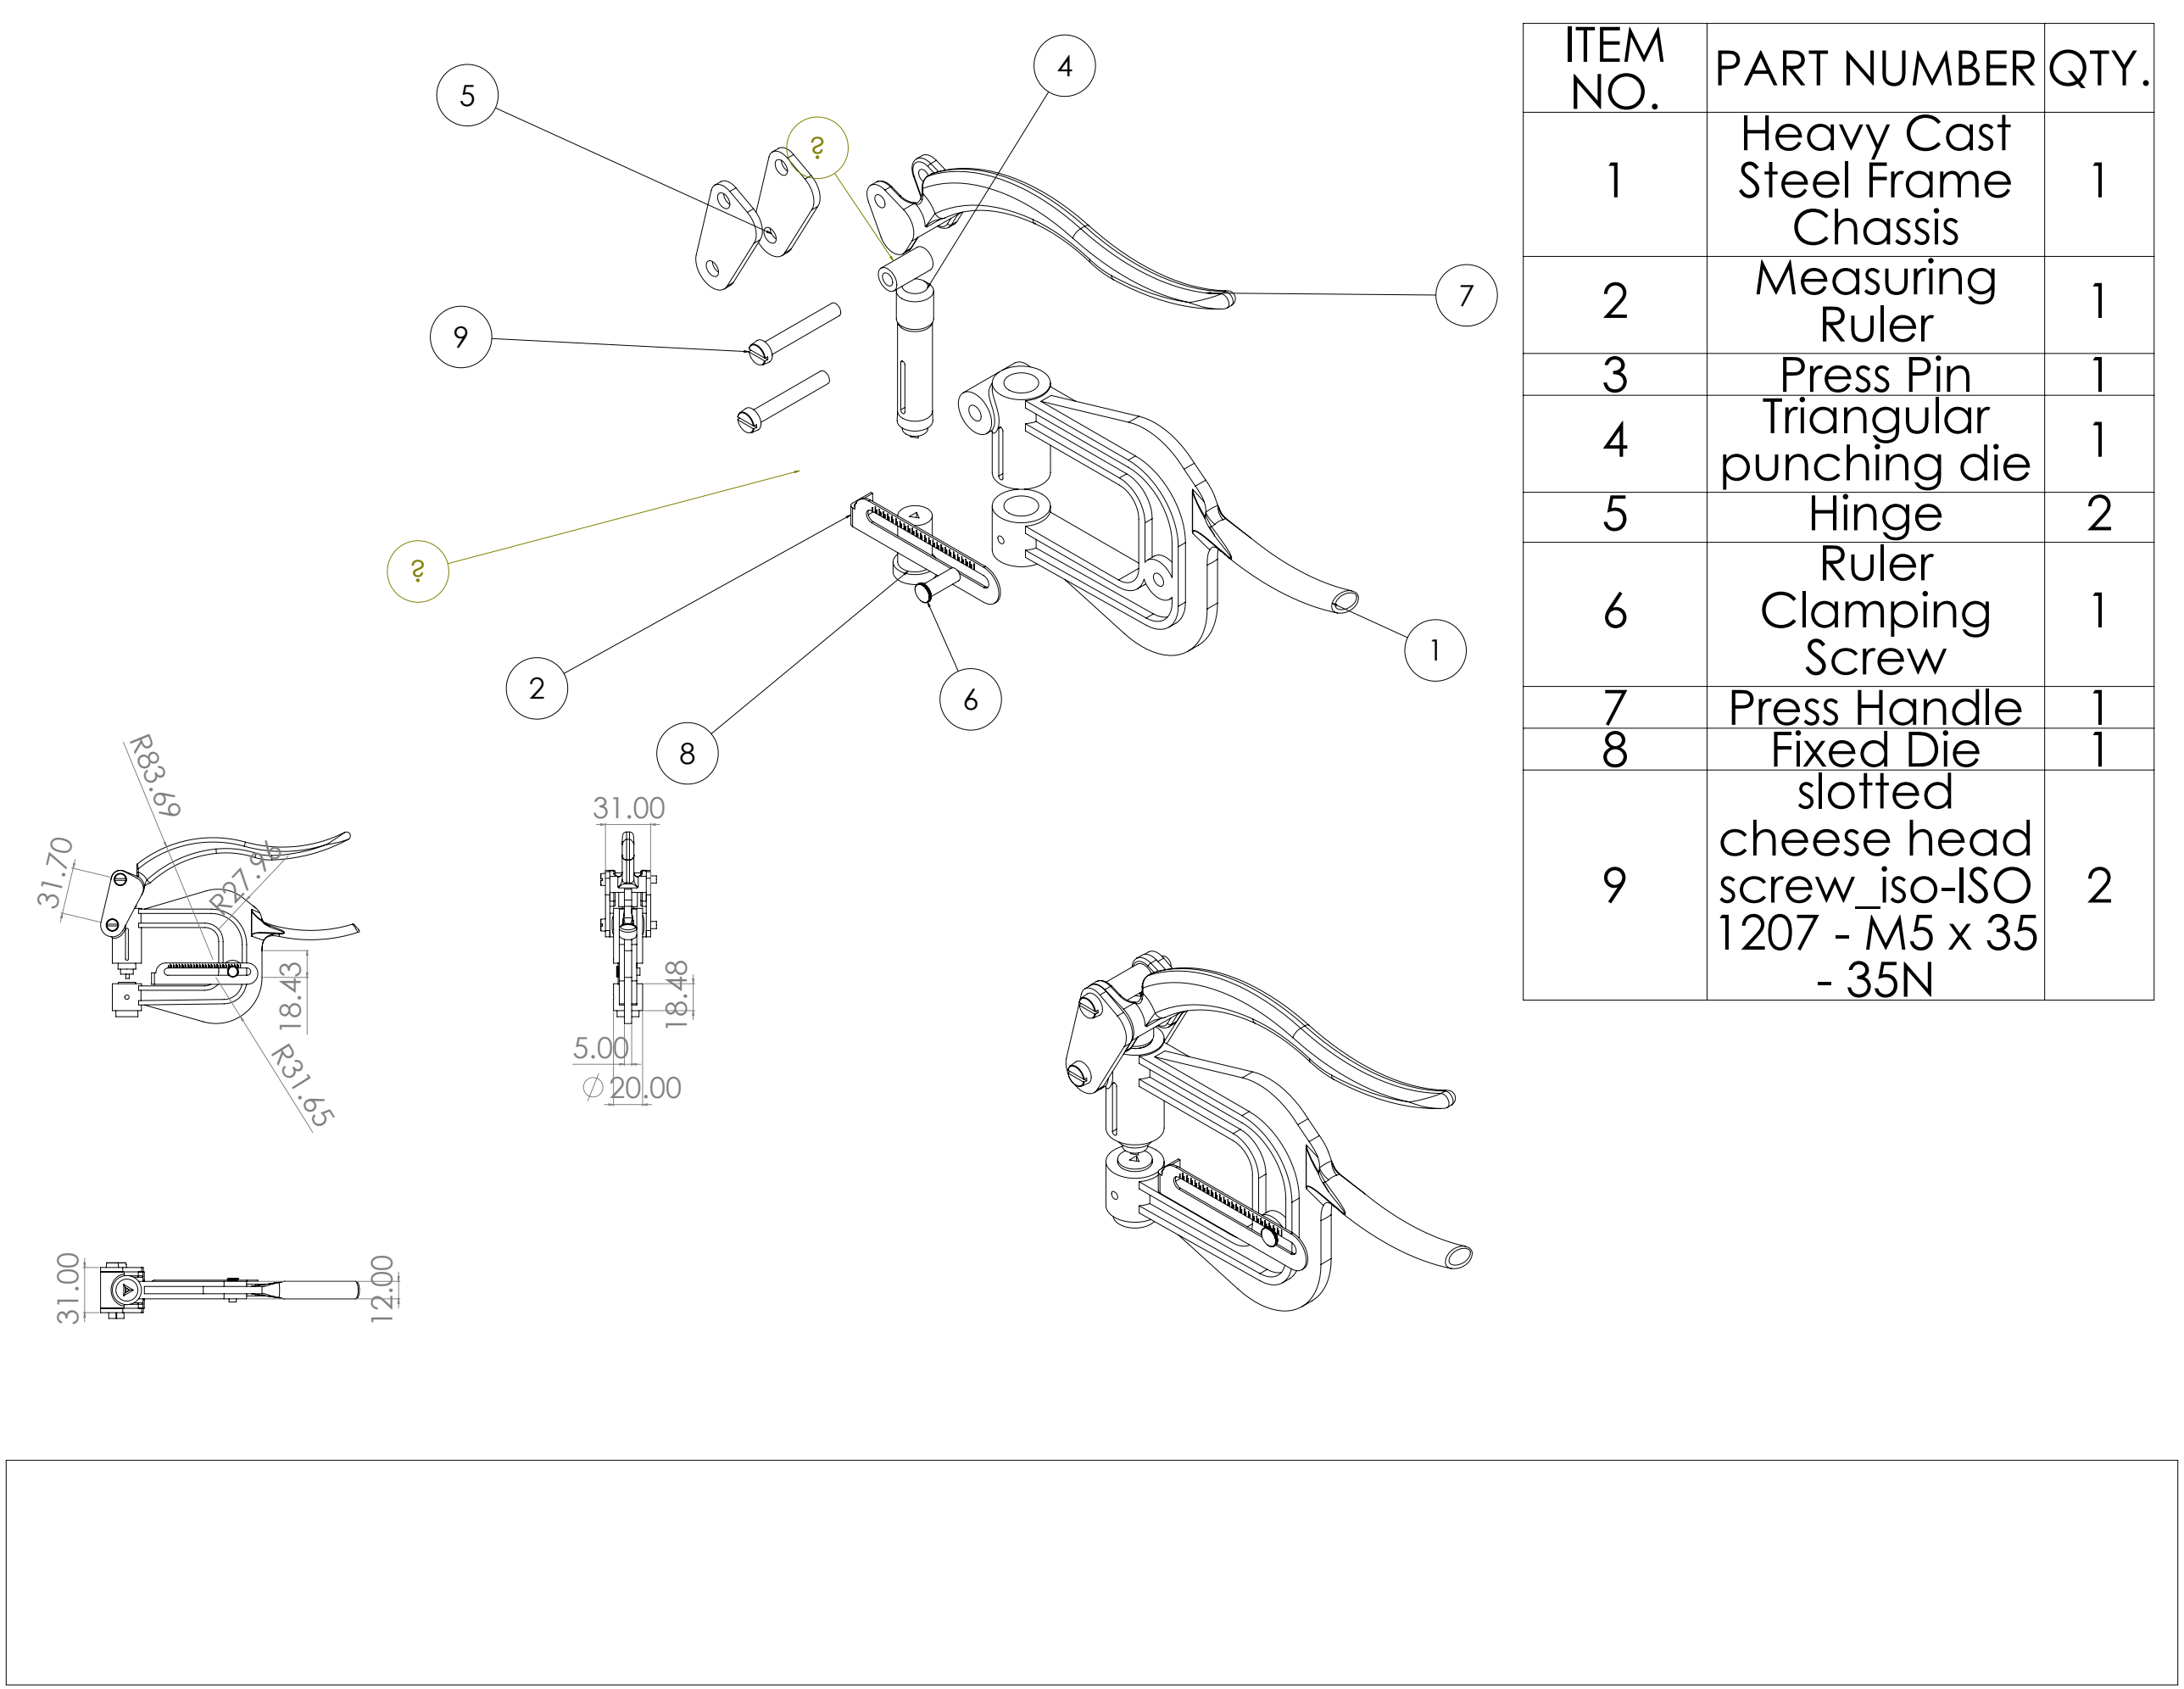
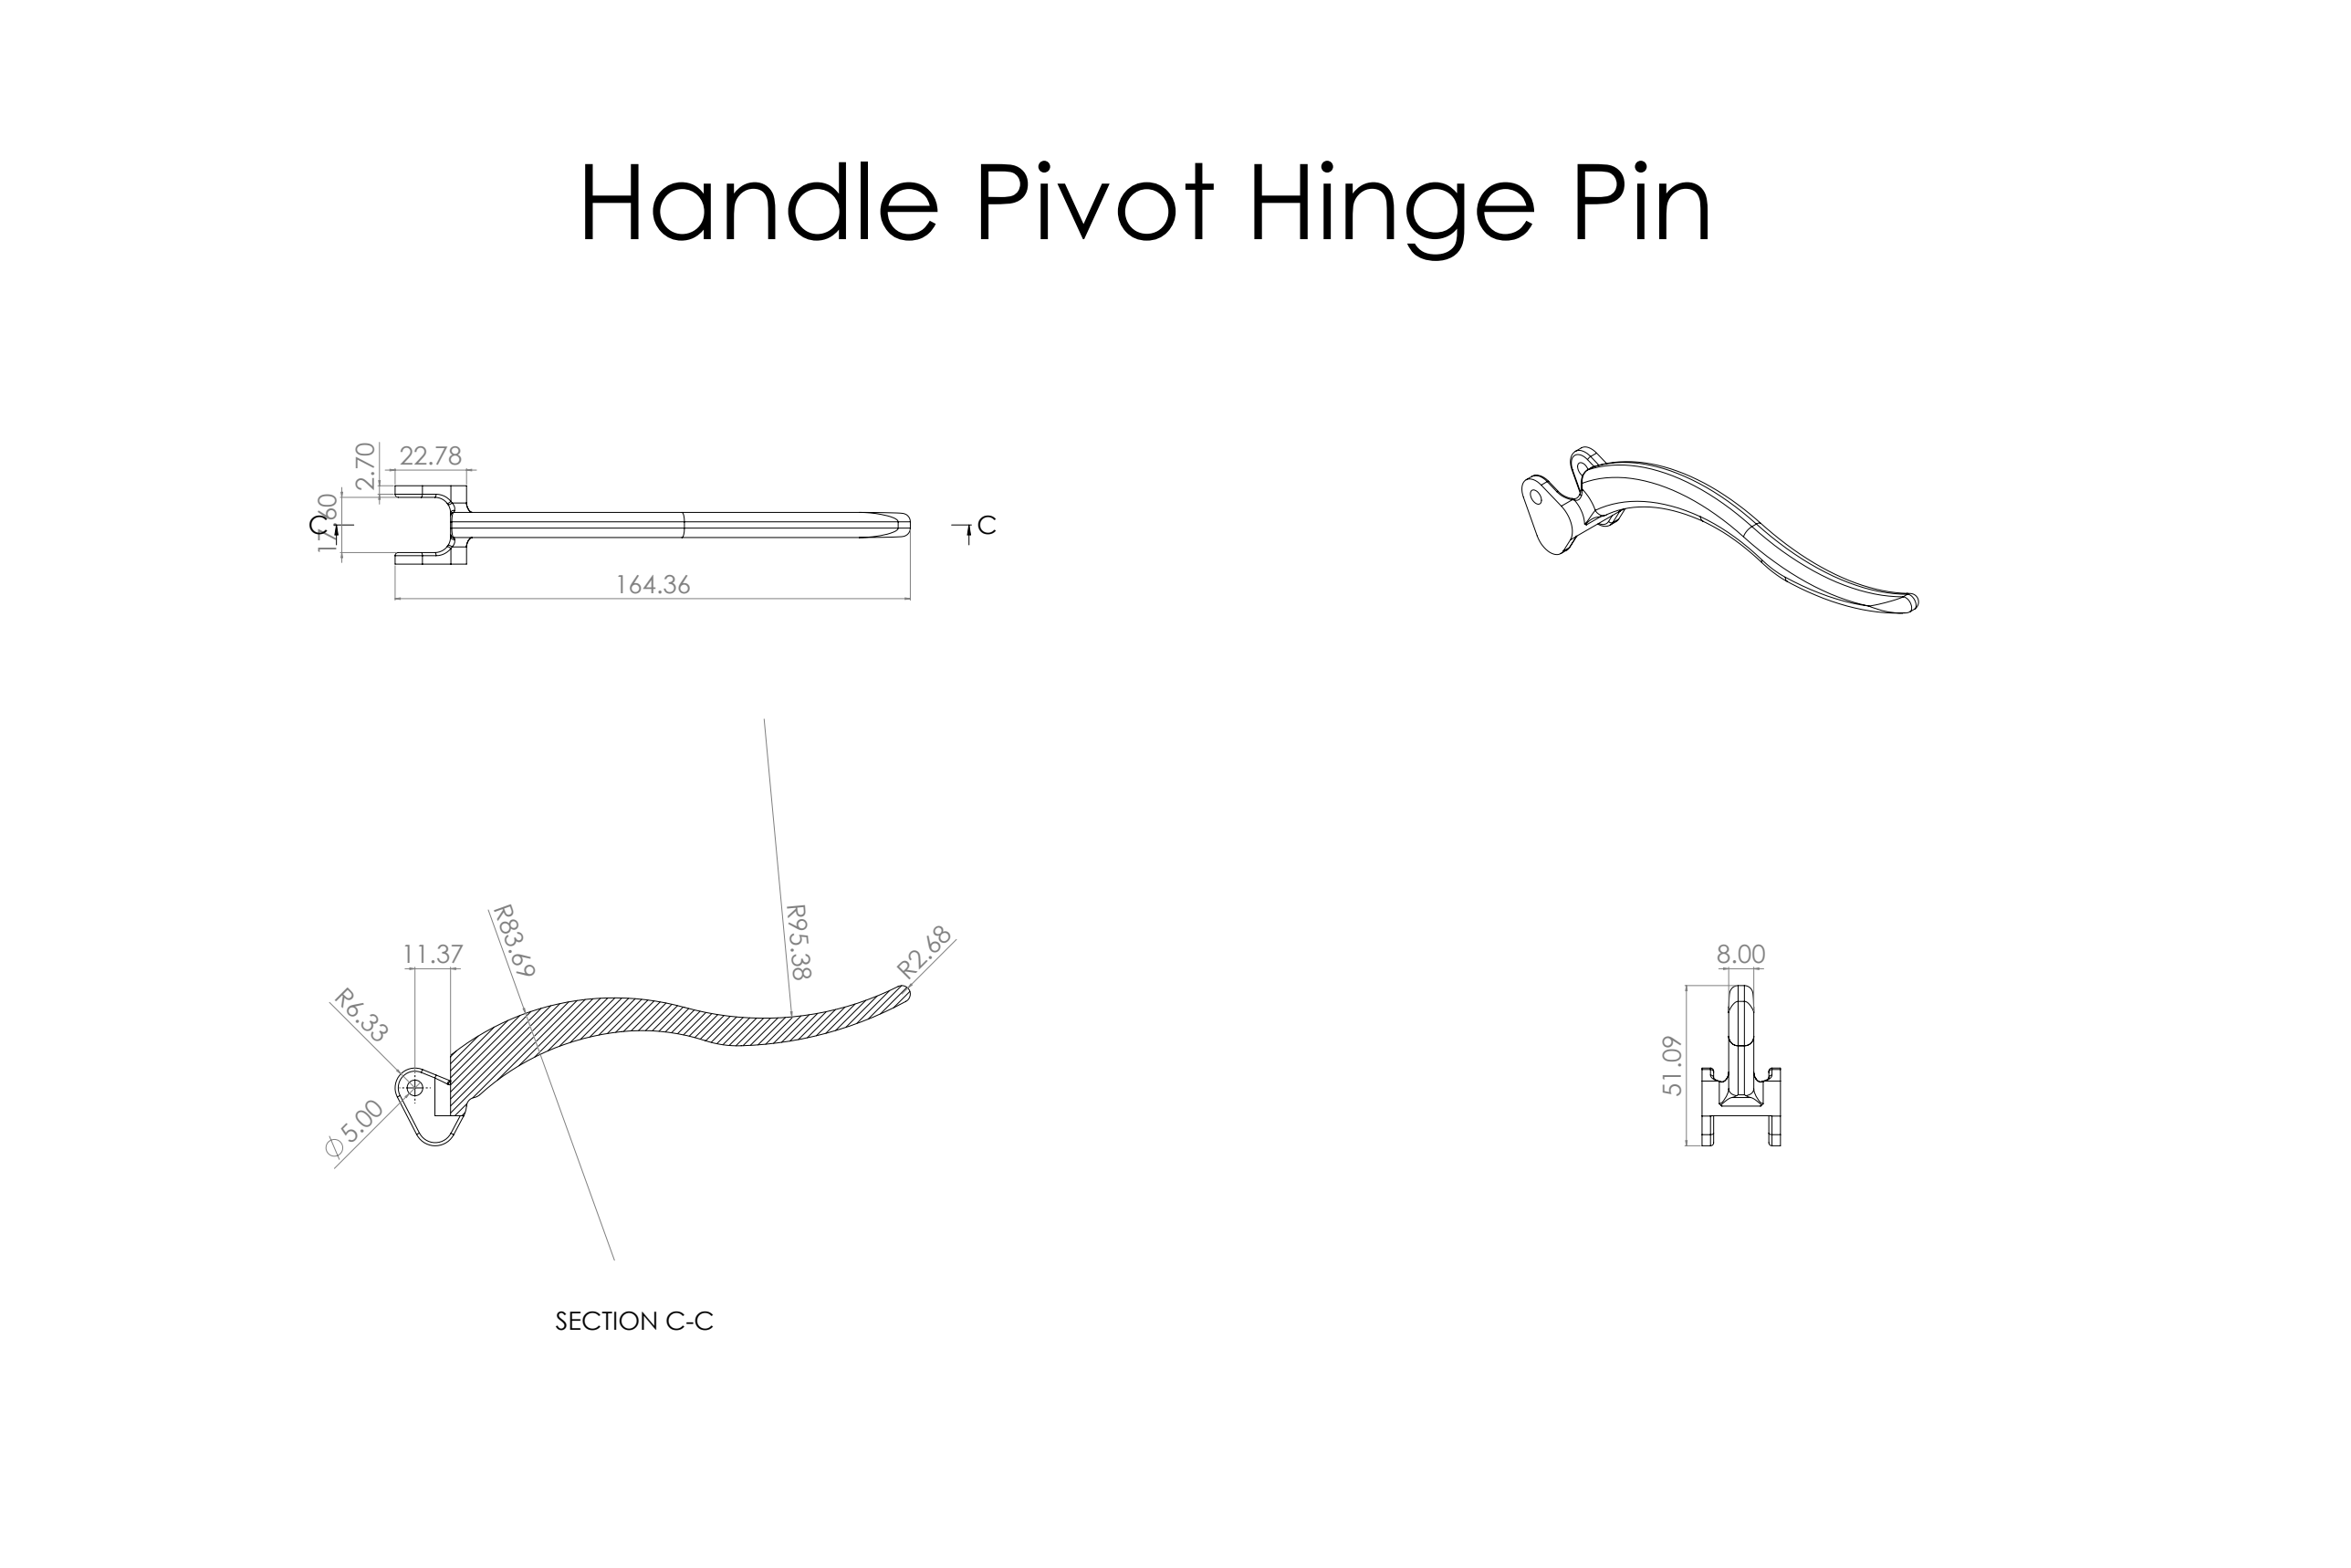
ISO-10303-21;
HEADER;
FILE_DESCRIPTION (('STEP AP214'),
    '1' );
FILE_NAME ('MAS-318',
    '2026-10-24T22:54:28',
    ( '' ),
    ( '' ),
    'SwSTEP 2.0',
    'SolidWorks 2025',
    '' );
FILE_SCHEMA (( 'AUTOMOTIVE_DESIGN' ));
ENDSEC;

DATA;
#1 = ORIENTED_EDGE ( 'NONE', *, *, #34988, .F. ) ;
#2 = CARTESIAN_POINT ( 'NONE',  ( 80.93548213101077238, 62.17232332437959030, -2.988136994358703724 ) ) ;
#3 = CARTESIAN_POINT ( 'NONE',  ( 35.84136525188217348, -3.161327592290550825, 5.800309892887216989 ) ) ;
#4 = EDGE_LOOP ( 'NONE', ( #11290, #35593, #8233, #19286 ) ) ;
#6 = DIRECTION ( 'NONE',  ( 0.000000000000000000, -1.000000000000000000, 0.000000000000000000 ) ) ;
#5 = CARTESIAN_POINT ( 'NONE',  ( 21.85645829928708039, 3.222455659797274663, 4.920547929353077166 ) ) ;
#7 = VERTEX_POINT ( 'NONE', #10173 ) ;
#8 = AXIS2_PLACEMENT_3D ( 'NONE', #5733, #22003, #2874 ) ;
#9 = CARTESIAN_POINT ( 'NONE',  ( -69.92837670882107659, -20.78299143688747819, 3.916079783099623679 ) ) ;
#10 =( BOUNDED_CURVE ( )  B_SPLINE_CURVE ( 3, ( #30460, #11695, #20771, #8817 ),
 .UNSPECIFIED., .F., .T. ) 
 B_SPLINE_CURVE_WITH_KNOTS ( ( 4, 4 ),
 ( 1.347909859412855349, 1.534781240595300522 ),
 .UNSPECIFIED. ) 
 CURVE ( )  GEOMETRIC_REPRESENTATION_ITEM ( )  RATIONAL_B_SPLINE_CURVE ( ( 1.000000000000000000, 0.9970920404276226723, 0.9970920404276226723, 1.000000000000000000 ) ) 
 REPRESENTATION_ITEM ( '' )  );
#11 = PRODUCT_DEFINITION_SHAPE ( 'NONE', 'NONE',  #40728 ) ;
#13 = CARTESIAN_POINT ( 'NONE',  ( -63.96477757089261473, 34.57625524247897175, 12.50000000000000000 ) ) ;
#12 = CARTESIAN_POINT ( 'NONE',  ( -71.92837670882107659, -20.78299143688747819, 38.00000000000000711 ) ) ;
#14 = LINE ( 'NONE', #31910, #38253 ) ;
#15 = CARTESIAN_POINT ( 'NONE',  ( -64.08758708074093136, 42.07456177326923097, -2.837280263138449943 ) ) ;
#16 = CARTESIAN_POINT ( 'NONE',  ( 73.82474952339838126, 59.08733682254641195, 3.476886323308218341 ) ) ;
#17 = EDGE_CURVE ( 'NONE', #19674, #35253, #14622, .T. ) ;
#18 = ORIENTED_EDGE ( 'NONE', *, *, #8070, .F. ) ;
#19 = CARTESIAN_POINT ( 'NONE',  ( 21.85695786933250062, 3.618345527896555058, -4.619311229777957273 ) ) ;
#20 = ORIENTED_EDGE ( 'NONE', *, *, #32884, .T. ) ;
#21 = CARTESIAN_POINT ( 'NONE',  ( 21.85643539959774273, 10.54442680926682208, -0.8960936389291185300 ) ) ;
#22 = CIRCLE ( 'NONE', #10506, 0.1000000000000028644 ) ;
#23 = CARTESIAN_POINT ( 'NONE',  ( 3.455257086698204194, -26.54807830652391587, 7.773839561854632763 ) ) ;
#24 = ORIENTED_EDGE ( 'NONE', *, *, #28416, .F. ) ;
#25 = ORIENTED_EDGE ( 'NONE', *, *, #12233, .F. ) ;
#26 = CARTESIAN_POINT ( 'NONE',  ( 1.060267149064800352, -26.12896262584469298, 7.720710062488891801 ) ) ;
#27 = CARTESIAN_POINT ( 'NONE',  ( 81.24504193829311305, 64.75648403698987465, 3.071899782094678066 ) ) ;
#28 = CARTESIAN_POINT ( 'NONE',  ( 84.98726364908050357, 2.895996327189970021, 0.3032432708941606436 ) ) ;
#29 = ORIENTED_EDGE ( 'NONE', *, *, #33251, .T. ) ;
#30 = EDGE_CURVE ( 'NONE', #25319, #33264, #34800, .T. ) ;
#31 = CARTESIAN_POINT ( 'NONE',  ( 0.5348300231373435132, -32.76390415370035214, 7.769368695748487319 ) ) ;
#32 = ORIENTED_EDGE ( 'NONE', *, *, #7574, .F. ) ;
#33 = CARTESIAN_POINT ( 'NONE',  ( 15.61026443024166888, -3.737113800699907618, 2.632854455050967157 ) ) ;
#34 = ADVANCED_FACE ( 'NONE', ( #40006 ), #27046, .T. ) ;
#35 = CARTESIAN_POINT ( 'NONE',  ( 34.13602976376383680, -3.136024335859604495, -5.534151046271431618 ) ) ;
#36 = CARTESIAN_POINT ( 'NONE',  ( 5.099449461929271621, -29.65043611971386639, 7.782034975670477195 ) ) ;
#37 = DIRECTION ( 'NONE',  ( 1.000000000000000000, 0.000000000000000000, 0.000000000000000000 ) ) ;
#38 = AXIS2_PLACEMENT_3D ( 'NONE', #3449, #15964, #28321 ) ;
#39 = CARTESIAN_POINT ( 'NONE',  ( -1.226608418644374421, -31.29986830985462376, 7.712764235869104645 ) ) ;
#40 = EDGE_CURVE ( 'NONE', #7218, #20784, #16731, .T. ) ;
#41 = ORIENTED_EDGE ( 'NONE', *, *, #18908, .F. ) ;
#42 = ORIENTED_EDGE ( 'NONE', *, *, #27798, .T. ) ;
#43 = CARTESIAN_POINT ( 'NONE',  ( 37.00808470818950013, -3.245065655003315896, 5.947274188226997715 ) ) ;
#44 = DIRECTION ( 'NONE',  ( -0.000000000000000000, -0.000000000000000000, 1.000000000000000000 ) ) ;
#45 = CARTESIAN_POINT ( 'NONE',  ( 66.41901733680204245, 57.79934748174496661, -4.000000000000019540 ) ) ;
#46 = CARTESIAN_POINT ( 'NONE',  ( 87.70627581785944926, -2.246752060737267964, -2.595469083058261184 ) ) ;
#47 = ORIENTED_EDGE ( 'NONE', *, *, #36430, .F. ) ;
#48 = CIRCLE ( 'NONE', #2012, 0.1000000000000028644 ) ;
#49 = CARTESIAN_POINT ( 'NONE',  ( -32.87867591359218977, -26.64985754041175525, 6.700000000000000178 ) ) ;
#50 = CARTESIAN_POINT ( 'NONE',  ( -70.92837670882107659, -23.80776546975053520, 0.000000000000000000 ) ) ;
#51 = ORIENTED_EDGE ( 'NONE', *, *, #25814, .F. ) ;
#52 = FACE_BOUND ( 'NONE', #30582, .T. ) ;
#53 = CARTESIAN_POINT ( 'NONE',  ( 3.926249267005272436, -32.27095793936597090, 6.894806418505347700 ) ) ;
#54 = EDGE_LOOP ( 'NONE', ( #15981, #402, #1244, #38858 ) ) ;
#55 = CARTESIAN_POINT ( 'NONE',  ( 24.04452188815935898, 3.332949059894338983, 3.268005727657652404 ) ) ;
#56 = CARTESIAN_POINT ( 'NONE',  ( 80.36293583174420974, 66.30725055998094319, -1.299258709309398130 ) ) ;
#57 = EDGE_CURVE ( 'NONE', #6790, #7577, #6515, .T. ) ;
#58 = CARTESIAN_POINT ( 'NONE',  ( 79.04990754624076033, 65.77731930041099417, 2.468641556982019925 ) ) ;
#59 = CARTESIAN_POINT ( 'NONE',  ( 2.829405163535268386, -26.36285597610873310, 7.703977250142849620 ) ) ;
#60 = ORIENTED_EDGE ( 'NONE', *, *, #39491, .F. ) ;
#61 = CARTESIAN_POINT ( 'NONE',  ( 76.46949791074162306, 63.77707083977483649, -3.308002540424319626 ) ) ;
#63 = CARTESIAN_POINT ( 'NONE',  ( -19.07867591359219972, -24.55319635012989110, 6.800000000000000711 ) ) ;
#62 = CARTESIAN_POINT ( 'NONE',  ( -71.02647992656017095, -45.61702805680359774, 6.000000000000006217 ) ) ;
#64 = CARTESIAN_POINT ( 'NONE',  ( 17.44489164598297748, 8.923283497490654526, -2.906184072486747816 ) ) ;
#65 = CARTESIAN_POINT ( 'NONE',  ( 81.32291525751645622, 62.59435864775878144, -3.036434590848177795 ) ) ;
#66 = CARTESIAN_POINT ( 'NONE',  ( 78.75717319332348154, 60.46956391627949756, 2.498359881428524609 ) ) ;
#67 = ORIENTED_EDGE ( 'NONE', *, *, #17962, .F. ) ;
#68 = VECTOR ( 'NONE', #23704, 1000.000000000000114 ) ;
#69 = DIRECTION ( 'NONE',  ( 0.000000000000000000, 0.000000000000000000, 1.000000000000000000 ) ) ;
#70 = CARTESIAN_POINT ( 'NONE',  ( 1.700390093233090871, -29.56993018339339940, 7.800000000000000711 ) ) ;
#71 = CARTESIAN_POINT ( 'NONE',  ( 80.25084519670748762, 66.24728552308215512, 1.725837398062988415 ) ) ;
#73 = CARTESIAN_POINT ( 'NONE',  ( -1.583170569706177977, -30.78163712919650052, 7.638132480492516585 ) ) ;
#72 = DIRECTION ( 'NONE',  ( -0.000000000000000000, 1.000000000000000000, -0.000000000000000000 ) ) ;
#74 = CARTESIAN_POINT ( 'NONE',  ( 27.93970670347097851, 2.313158937601060838, 2.612756796560576689 ) ) ;
#75 = ADVANCED_FACE ( 'NONE', ( #21079, #21280 ), #17552, .T. ) ;
#76 = EDGE_CURVE ( 'NONE', #14380, #23841, #36922, .T. ) ;
#77 = CARTESIAN_POINT ( 'NONE',  ( -1.419381273142192645, -31.15644416743037937, 6.921725064902950031 ) ) ;
#78 = CARTESIAN_POINT ( 'NONE',  ( 21.32819773538203734, -0.9284710762945487250, 4.803740791084685213 ) ) ;
#79 = CARTESIAN_POINT ( 'NONE',  ( -64.37872067649581709, 36.58503142451505141, 5.660009492437676037 ) ) ;
#80 = EDGE_CURVE ( 'NONE', #2391, #5443, #34066, .T. ) ;
#81 = DIRECTION ( 'NONE',  ( -0.000000000000000000, -0.000000000000000000, -1.000000000000000000 ) ) ;
#82 = ORIENTED_EDGE ( 'NONE', *, *, #9020, .T. ) ;
#83 = CARTESIAN_POINT ( 'NONE',  ( -0.6417018516168193631, -32.03460162637909292, 6.959317978105162616 ) ) ;
#84 = DIRECTION ( 'NONE',  ( 0.8660254037844393737, 0.000000000000000000, 0.4999999999999985567 ) ) ;
#85 = PLANE ( 'NONE',  #11053 ) ;
#86 = CARTESIAN_POINT ( 'NONE',  ( 33.43749314767592296, -3.587398716883661631, -5.336340041065867901 ) ) ;
#87 = CARTESIAN_POINT ( 'NONE',  ( -0.8882241849766865371, -31.77426936318072848, 7.740055089680403455 ) ) ;
#88 = CARTESIAN_POINT ( 'NONE',  ( 0.4809511200452799562, -32.83872382006634894, 7.781480525794716385 ) ) ;
#89 = DIRECTION ( 'NONE',  ( -0.000000000000000000, -0.000000000000000000, 1.000000000000000000 ) ) ;
#90 = CARTESIAN_POINT ( 'NONE',  ( 87.15505355144220800, 0.4610318193416703680, -5.246243280819175681 ) ) ;
#91 = CARTESIAN_POINT ( 'NONE',  ( 23.06594672544511582, -8.086844732617873177, 2.500000000000001332 ) ) ;
#92 = CARTESIAN_POINT ( 'NONE',  ( -14.44874870218064089, -26.64985754041175525, 6.700000000000000178 ) ) ;
#93 = ORIENTED_EDGE ( 'NONE', *, *, #2114, .F. ) ;
#94 = DIRECTION ( 'NONE',  ( -0.000000000000000000, -0.000000000000000000, -1.000000000000000000 ) ) ;
#95 = CARTESIAN_POINT ( 'NONE',  ( 68.04343099365841852, 58.34291608657256489, -3.996230182412897403 ) ) ;
#96 = AXIS2_PLACEMENT_3D ( 'NONE', #13585, #39295, #10487 ) ;
#97 = CARTESIAN_POINT ( 'NONE',  ( 2.985793545108982983, -26.31449737714283543, 6.863805608295730387 ) ) ;
#98 = ORIENTED_EDGE ( 'NONE', *, *, #35067, .F. ) ;
#99 = CARTESIAN_POINT ( 'NONE',  ( 8.290806648384990041, -33.63722727088462250, 6.000000000000001776 ) ) ;
#100 = CARTESIAN_POINT ( 'NONE',  ( 5.698101969243359655, -32.85371976261941285, 7.695279973900954751 ) ) ;
#101 = PRODUCT ( 'Press Handle', 'Press Handle', '', ( #4245 ) ) ;
#102 = CARTESIAN_POINT ( 'NONE',  ( 1.179471205431445346, -26.21005746276246029, 7.784476445165072533 ) ) ;
#103 = CARTESIAN_POINT ( 'NONE',  ( 5.054793046568992310, -30.12489038615697012, 7.703977250142847844 ) ) ;
#104 = ORIENTED_EDGE ( 'NONE', *, *, #1781, .F. ) ;
#105 = CARTESIAN_POINT ( 'NONE',  ( 24.41733686895641853, 3.169751135957838084, 3.243633740826553424 ) ) ;
#106 = CARTESIAN_POINT ( 'NONE',  ( 1.651639975615219580, -32.96958066925694908, 6.894806418505345036 ) ) ;
#107 = VECTOR ( 'NONE', #13832, 1000.000000000000000 ) ;
#108 = CARTESIAN_POINT ( 'NONE',  ( -1.333134932519906446, -31.10541900397473825, 7.013842709614101167 ) ) ;
#109 = VERTEX_POINT ( 'NONE', #17965 ) ;
#110 = CARTESIAN_POINT ( 'NONE',  ( 78.59948840878007559, 65.10367658859402695, -3.015657119755322579 ) ) ;
#112 = CARTESIAN_POINT ( 'NONE',  ( -40.44874870218063734, -26.64985754041175525, 6.700000000000000178 ) ) ;
#111 = CARTESIAN_POINT ( 'NONE',  ( 23.09356329134889663, 0.3660385851480518205, 5.918987391801470821 ) ) ;
#113 = B_SPLINE_CURVE_WITH_KNOTS ( 'NONE', 3,
 ( #29364, #35364, #7331, #3877, #28763, #574, #25671, #10213, #29561, #28964 ),
 .UNSPECIFIED., .F., .F.,
 ( 4, 3, 3, 4 ),
 ( 8.388765757908052086E-05, 0.0001053129305727058042, 0.0001360598016347105499, 0.0001612931755702039531 ),
 .UNSPECIFIED. ) ;
#114 = CARTESIAN_POINT ( 'NONE',  ( 81.64185025298566245, 61.96196063151609223, -2.170472567296702682 ) ) ;
#115 = CARTESIAN_POINT ( 'NONE',  ( 80.76516742887832834, 61.34548671587045021, 2.174061886842027391 ) ) ;
#116 = EDGE_CURVE ( 'NONE', #25222, #15928, #15693, .T. ) ;
#117 = EDGE_CURVE ( 'NONE', #23904, #23738, #12152, .T. ) ;
#118 = CARTESIAN_POINT ( 'NONE',  ( 82.55792188592127445, 63.20960171500894376, 1.000000000000000000 ) ) ;
#119 = CARTESIAN_POINT ( 'NONE',  ( 2.752162513012757827, -32.80316080117250266, 7.759451378593094084 ) ) ;
#120 = CARTESIAN_POINT ( 'NONE',  ( 21.85643539959779602, 4.838159542671753854, -10.55000746994157979 ) ) ;
#121 = EDGE_LOOP ( 'NONE', ( #23412, #22869, #10746, #16528 ) ) ;
#122 = CARTESIAN_POINT ( 'NONE',  ( -73.76321677170048474, 8.370041474172571938, 9.593160009199120708 ) ) ;
#123 = CARTESIAN_POINT ( 'NONE',  ( 37.18496992949054913, -2.918767381260244154, 5.998331359843706245 ) ) ;
#124 = ORIENTED_EDGE ( 'NONE', *, *, #26461, .T. ) ;
#125 = EDGE_CURVE ( 'NONE', #38679, #29790, #4804, .T. ) ;
#126 = CARTESIAN_POINT ( 'NONE',  ( -1.313163417236760111, -31.34995842213618999, 7.678495282201405203 ) ) ;
#127 = CARTESIAN_POINT ( 'NONE',  ( -80.34626650618338317, 10.54088118240301775, -3.386839445737261034 ) ) ;
#128 = CARTESIAN_POINT ( 'NONE',  ( 28.64320648638592104, -3.206774183960824587, -4.676863129512683237 ) ) ;
#129 = CARTESIAN_POINT ( 'NONE',  ( 37.18689723876565978, -2.963747097358016003, -6.000011646107364705 ) ) ;
#130 = CARTESIAN_POINT ( 'NONE',  ( -4.890026461918814071, -8.228598103685714525E-16, 6.000000000000000000 ) ) ;
#131 = SHAPE_REPRESENTATION ( 'Heavy Cast Steel Frame Chassis', ( #30744 ), #7710 ) ;
#132 = CARTESIAN_POINT ( 'NONE',  ( 21.48907598089328630, 5.617352746613489600, 3.514627525551620391 ) ) ;
#133 = CARTESIAN_POINT ( 'NONE',  ( -1.740904132959085304, -28.93157757802832819, 6.894806418505347700 ) ) ;
#134 = DIRECTION ( 'NONE',  ( 7.826543628040252284E-17, -1.000000000000000000, 0.000000000000000000 ) ) ;
#135 = DIRECTION ( 'NONE',  ( 0.000000000000000000, 0.000000000000000000, -1.000000000000000000 ) ) ;
#136 = DIRECTION ( 'NONE',  ( -1.000000000000000000, 0.000000000000000000, 0.000000000000000000 ) ) ;
#137 = CARTESIAN_POINT ( 'NONE',  ( 21.75356392267549310, 0.6818289899092313533, -8.045969637709488254 ) ) ;
#138 = VECTOR ( 'NONE', #4313, 1000.000000000000000 ) ;
#139 = CARTESIAN_POINT ( 'NONE',  ( 32.63483486068848549, -3.790703822822770075, -4.926795467402606654 ) ) ;
#140 = CARTESIAN_POINT ( 'NONE',  ( 25.39710067966193918, 2.282707499838438459, -4.082506721808119465 ) ) ;
#141 = VERTEX_POINT ( 'NONE', #15910 ) ;
#142 = VERTEX_POINT ( 'NONE', #21892 ) ;
#143 = CARTESIAN_POINT ( 'NONE',  ( 66.81418162778464875, 58.07599004166701206, 3.996206253860483226 ) ) ;
#144 = CARTESIAN_POINT ( 'NONE',  ( 35.79015163951060430, -3.279169341215469213, 5.792316770070685017 ) ) ;
#145 = DIRECTION ( 'NONE',  ( 0.7055275666422168301, -0.2567910337120241637, -0.6605219282605403475 ) ) ;
#146 = CARTESIAN_POINT ( 'NONE',  ( 87.19696342060086636, -0.1553247823698818142, -5.755373573531420206 ) ) ;
#148 = DIRECTION ( 'NONE',  ( 0.000000000000000000, 1.000000000000000000, 0.000000000000000000 ) ) ;
#147 = CARTESIAN_POINT ( 'NONE',  ( -83.92837670882109080, 2.429809908903242555, 15.50000000000000000 ) ) ;
#149 = ORIENTED_EDGE ( 'NONE', *, *, #27849, .F. ) ;
#150 = CARTESIAN_POINT ( 'NONE',  ( 24.34527755301806451, 2.925195485058063927, 3.749207160500627634 ) ) ;
#151 =( NAMED_UNIT ( * ) PLANE_ANGLE_UNIT ( ) SI_UNIT ( $, .RADIAN. ) );
#152 = CARTESIAN_POINT ( 'NONE',  ( -1.531573891984414848, -33.61112889622174293, 7.754798119455333705 ) ) ;
#153 = VERTEX_POINT ( 'NONE', #35081 ) ;
#154 = CARTESIAN_POINT ( 'NONE',  ( 3.979840844262043209, -26.93328804621895145, 7.785344483711591934 ) ) ;
#155 = ORIENTED_EDGE ( 'NONE', *, *, #18670, .T. ) ;
#156 = CARTESIAN_POINT ( 'NONE',  ( 80.09094484276194237, 63.40703332228277134, -3.714073935154547978 ) ) ;
#157 = CARTESIAN_POINT ( 'NONE',  ( 4.045228995182856835, -26.97152095390259063, 7.750000000000000888 ) ) ;
#158 = CARTESIAN_POINT ( 'NONE',  ( 80.96252947514877008, 61.71397308826822581, 2.561782662428527146 ) ) ;
#160 = VERTEX_POINT ( 'NONE', #28468 ) ;
#159 = CARTESIAN_POINT ( 'NONE',  ( -1.333134932519906446, -31.10541900397473825, 7.013842709614101167 ) ) ;
#161 = CARTESIAN_POINT ( 'NONE',  ( -56.74902312943272165, 30.60926302035622371, 3.177788716294913218 ) ) ;
#162 = DIRECTION ( 'NONE',  ( 1.000000000000000000, 0.000000000000000000, 0.000000000000000000 ) ) ;
#163 = CARTESIAN_POINT ( 'NONE',  ( -71.80187163192030653, -21.28714814314140469, 9.961904852117910991 ) ) ;
#164 = CARTESIAN_POINT ( 'NONE',  ( 5.401390093233090717, -29.58343279012807159, 7.635761828346577573 ) ) ;
#165 = CARTESIAN_POINT ( 'NONE',  ( 22.18865037645032601, 5.257466153314783064, -3.084642082178049360 ) ) ;
#166 = ORIENTED_EDGE ( 'NONE', *, *, #31920, .F. ) ;
#167 = CIRCLE ( 'NONE', #21192, 3.000000000000002665 ) ;
#168 = EDGE_CURVE ( 'NONE', #27559, #13108, #28679, .T. ) ;
#169 = VERTEX_POINT ( 'NONE', #9734 ) ;
#170 = ADVANCED_FACE ( 'NONE', ( #3587 ), #276, .T. ) ;
#171 = CARTESIAN_POINT ( 'NONE',  ( -1.621161547238496814, -30.32835594263312018, 7.139196562012270597 ) ) ;
#172 = ADVANCED_FACE ( 'NONE', ( #34882 ), #28059, .T. ) ;
#173 = CARTESIAN_POINT ( 'NONE',  ( -80.59724102483603758, -5.646254625739555166, -5.338710406051827562 ) ) ;
#174 = DIRECTION ( 'NONE',  ( 0.1736481776669273336, 0.9848077530122085754, -0.000000000000000000 ) ) ;
#175 = CARTESIAN_POINT ( 'NONE',  ( 80.63945418285952371, 64.43655742540516940, 3.486376426170536114 ) ) ;
#176 = CARTESIAN_POINT ( 'NONE',  ( 87.91343731185466481, -2.496140582104141359, -0.8634702502314072214 ) ) ;
#177 = CARTESIAN_POINT ( 'NONE',  ( -0.5626977249550375593, -26.90001753928526540, 7.750000000000002665 ) ) ;
#178 = ORIENTED_EDGE ( 'NONE', *, *, #20772, .F. ) ;
#179 = LINE ( 'NONE', #33956, #26669 ) ;
#180 = CARTESIAN_POINT ( 'NONE',  ( -2.184219888937934950, -32.98850935093154391, 7.754798119455333705 ) ) ;
#181 = CARTESIAN_POINT ( 'NONE',  ( 4.091040325523227494, -27.01360636453728503, 6.980586498568968956 ) ) ;
#182 = CARTESIAN_POINT ( 'NONE',  ( -32.44874870218063734, -26.64985754041175525, 6.700000000000000178 ) ) ;
#183 = CARTESIAN_POINT ( 'NONE',  ( 4.697270888919727660, -27.96407818295915249, 7.768425012602590662 ) ) ;
#184 = ORIENTED_EDGE ( 'NONE', *, *, #32019, .F. ) ;
#185 = CARTESIAN_POINT ( 'NONE',  ( 35.86808974331964350, -2.088826501973227057, 5.804480896110276511 ) ) ;
#186 = CARTESIAN_POINT ( 'NONE',  ( 4.308434419475116961, -31.75125399145456484, 7.763628509615286610 ) ) ;
#187 = CARTESIAN_POINT ( 'NONE',  ( 87.73528170195316989, -0.1907079786014589107, -4.255344914058586170 ) ) ;
#188 = EDGE_LOOP ( 'NONE', ( #27353, #29698, #8514, #37884 ) ) ;
#190 = CARTESIAN_POINT ( 'NONE',  ( -63.71197174466732349, 35.78007194159061299, 7.175960652854955768 ) ) ;
#189 = CARTESIAN_POINT ( 'NONE',  ( 81.06839910345442490, 62.80152057670051846, -3.286127602909473033 ) ) ;
#191 = DIRECTION ( 'NONE',  ( 1.000000000000000000, 0.000000000000000000, 0.000000000000000000 ) ) ;
#192 = AXIS2_PLACEMENT_3D ( 'NONE', #26818, #39356, #4992 ) ;
#193 = ORIENTED_EDGE ( 'NONE', *, *, #36678, .T. ) ;
#194 = DIRECTION ( 'NONE',  ( -0.000000000000000000, -1.000000000000000000, -0.000000000000000000 ) ) ;
#195 = ORIENTED_EDGE ( 'NONE', *, *, #21675, .F. ) ;
#196 = CARTESIAN_POINT ( 'NONE',  ( -72.40112826922974421, 5.951953399866846794, 9.891857903246553008 ) ) ;
#197 = ORIENTED_EDGE ( 'NONE', *, *, #37878, .T. ) ;
#198 = CARTESIAN_POINT ( 'NONE',  ( 81.07009230622234952, 61.73904331373559984, -2.506402126386314322 ) ) ;
#199 = CARTESIAN_POINT ( 'NONE',  ( 21.94883752246645514, 5.596572238070317340, 3.078924485188955895 ) ) ;
#201 = CARTESIAN_POINT ( 'NONE',  ( 27.23730700677205618, 2.045195204592743288, 3.801859922671973369 ) ) ;
#200 = CARTESIAN_POINT ( 'NONE',  ( 25.44397797946202289, 1.878947632829091274, 4.230557655479292301 ) ) ;
#203 = ORIENTED_EDGE ( 'NONE', *, *, #13724, .F. ) ;
#202 = ORIENTED_EDGE ( 'NONE', *, *, #26812, .F. ) ;
#204 = CARTESIAN_POINT ( 'NONE',  ( 4.710286264421988278, -27.98859379816425985, 6.865312560952602894 ) ) ;
#206 = CARTESIAN_POINT ( 'NONE',  ( 85.45774792847294066, 2.367526054045318240, -2.907096912194419236 ) ) ;
#205 = CARTESIAN_POINT ( 'NONE',  ( -31.07867591359219617, -26.64985754041175525, 6.700000000000000178 ) ) ;
#207 = CARTESIAN_POINT ( 'NONE',  ( -71.92837670882106238, -36.87473357531881391, 0.000000000000000000 ) ) ;
#208 = CARTESIAN_POINT ( 'NONE',  ( 1.090397816225958216, -0.6000000000000004219, 4.012069227840649788 ) ) ;
#209 = CARTESIAN_POINT ( 'NONE',  ( 69.48201546320520094, 59.78788955577742570, 3.863726395435664873 ) ) ;
#210 = VECTOR ( 'NONE', #7329, 1000.000000000000000 ) ;
#211 = CARTESIAN_POINT ( 'NONE',  ( 23.22388547762907507, 3.341220446849921366, -3.796200845986580141 ) ) ;
#212 = VERTEX_POINT ( 'NONE', #19008 ) ;
#213 = CARTESIAN_POINT ( 'NONE',  ( 21.85643539959774273, -10.14878426894149221, 9.991042268249278990 ) ) ;
#215 = EDGE_CURVE ( 'NONE', #29684, #24175, #38700, .T. ) ;
#214 = CARTESIAN_POINT ( 'NONE',  ( -58.99259650353461382, 28.71101865976197587, -6.736149549807849191 ) ) ;
#216 = CARTESIAN_POINT ( 'NONE',  ( 81.76017987128392406, 63.49575590176132067, 2.919551171211350216 ) ) ;
#217 = CARTESIAN_POINT ( 'NONE',  ( 88.07575545775937087, -0.5731442609823791390, 3.387043347726935050 ) ) ;
#218 = VERTEX_POINT ( 'NONE', #31772 ) ;
#219 = VECTOR ( 'NONE', #28713, 1000.000000000000000 ) ;
#220 = CARTESIAN_POINT ( 'NONE',  ( 14.77315594796442966, 13.19392823276588089, 2.499999999999996891 ) ) ;
#221 = ORIENTED_EDGE ( 'NONE', *, *, #39543, .T. ) ;
#222 = CARTESIAN_POINT ( 'NONE',  ( 26.28033317518049472, -2.868937434659071695, 4.308079602883402970 ) ) ;
#223 = CARTESIAN_POINT ( 'NONE',  ( 33.68713372036676645, -3.101946962961664500, -5.464089962110080911 ) ) ;
#224 = DIRECTION ( 'NONE',  ( 0.8660254037844378194, 0.000000000000000000, -0.5000000000000015543 ) ) ;
#225 = CARTESIAN_POINT ( 'NONE',  ( 0.9702812410957980527, -32.99293223504097483, 7.751599049952198506 ) ) ;
#226 = CARTESIAN_POINT ( 'NONE',  ( 4.404516770028685357, -31.79202354683301834, 7.697032948437507294 ) ) ;
#227 = CYLINDRICAL_SURFACE ( 'NONE', #21754, 6.681288188914807691 ) ;
#228 = CARTESIAN_POINT ( 'NONE',  ( -38.34874870218063592, -25.49307895267003587, 6.800000000000000711 ) ) ;
#229 = VECTOR ( 'NONE', #9739, 1000.000000000000000 ) ;
#230 = AXIS2_PLACEMENT_3D ( 'NONE', #30843, #30009, #20734 ) ;
#231 = CARTESIAN_POINT ( 'NONE',  ( 31.99965334531182393, -3.138902966780172665, 5.200717837716557490 ) ) ;
#232 = ORIENTED_EDGE ( 'NONE', *, *, #27570, .F. ) ;
#233 = EDGE_LOOP ( 'NONE', ( #32322, #27036, #31978, #32263 ) ) ;
#234 = CARTESIAN_POINT ( 'NONE',  ( 20.91779494910925052, 4.579615739114438533, 2.660980063663031636 ) ) ;
#235 = DIRECTION ( 'NONE',  ( 1.000000000000000000, -1.982541115402065307E-15, 0.000000000000000000 ) ) ;
#236 = EDGE_CURVE ( 'NONE', #37067, #38999, #489, .T. ) ;
#237 = CARTESIAN_POINT ( 'NONE',  ( 66.56396446968585678, 57.85070090013417854, -3.999903336036485957 ) ) ;
#238 = CARTESIAN_POINT ( 'NONE',  ( -0.4939712552137372481, -26.86236983215355778, 7.785593909369612931 ) ) ;
#239 = ORIENTED_EDGE ( 'NONE', *, *, #18400, .F. ) ;
#240 = CARTESIAN_POINT ( 'NONE',  ( 87.52056228721085063, 0.05047505923521825727, -4.363535012332786955 ) ) ;
#241 = CARTESIAN_POINT ( 'NONE',  ( -0.9807834779648342272, -31.66069757387703731, 7.754798119455333705 ) ) ;
#242 = CARTESIAN_POINT ( 'NONE',  ( 4.950332314942309964, -28.57099297037561314, 6.882085323592685988 ) ) ;
#243 = CARTESIAN_POINT ( 'NONE',  ( -0.8662471634088840799, -27.19035536265291242, 7.009310105710486738 ) ) ;
#244 =( BOUNDED_CURVE ( )  B_SPLINE_CURVE ( 3, ( #39857, #2200, #21130, #40056 ),
 .UNSPECIFIED., .F., .T. ) 
 B_SPLINE_CURVE_WITH_KNOTS ( ( 4, 4 ),
 ( 4.708531083176466403, 4.895802057644187855 ),
 .UNSPECIFIED. ) 
 CURVE ( )  GEOMETRIC_REPRESENTATION_ITEM ( )  RATIONAL_B_SPLINE_CURVE ( ( 1.000000000000000000, 0.9970795998553221295, 0.9970795998553221295, 1.000000000000000000 ) ) 
 REPRESENTATION_ITEM ( '' )  );
#245 = FACE_BOUND ( 'NONE', #8668, .T. ) ;
#246 = CARTESIAN_POINT ( 'NONE',  ( -59.00110696496997775, 28.68040728033255249, -6.999999999999999112 ) ) ;
#247 = ORIENTED_EDGE ( 'NONE', *, *, #38016, .F. ) ;
#248 = CARTESIAN_POINT ( 'NONE',  ( 23.42285139394776650, 3.710806655037595547, 3.268438641518027765 ) ) ;
#249 = CARTESIAN_POINT ( 'NONE',  ( 82.38651420471377662, 62.84168609110417236, -1.553473047276889840 ) ) ;
#250 = EDGE_CURVE ( 'NONE', #11656, #22420, #37713, .T. ) ;
#251 = CARTESIAN_POINT ( 'NONE',  ( 79.70909206057019958, 64.65202245283560956, 3.503057693382588322 ) ) ;
#252 = CARTESIAN_POINT ( 'NONE',  ( 2.835692379953925535, -26.36507494999243306, 7.730758795053811028 ) ) ;
#253 = ORIENTED_EDGE ( 'NONE', *, *, #18491, .F. ) ;
#254 = CARTESIAN_POINT ( 'NONE',  ( 76.25248298134039260, 64.19605381821561707, -2.844364419910041519 ) ) ;
#256 = CARTESIAN_POINT ( 'NONE',  ( -20.24874870218063805, -26.64985754041175525, 6.800000000000000711 ) ) ;
#255 = CARTESIAN_POINT ( 'NONE',  ( -72.12756863348978698, -46.19478142241662511, 5.880635833492268816 ) ) ;
#257 = CARTESIAN_POINT ( 'NONE',  ( 15.15950051851460145, 11.94258596470134215, -2.548869419651209611 ) ) ;
#258 = CARTESIAN_POINT ( 'NONE',  ( 80.74417485493692936, 64.10566034184273576, -3.509897338575004522 ) ) ;
#259 = CARTESIAN_POINT ( 'NONE',  ( 79.36485406729205749, 60.67242113316877550, 2.285396881590402440 ) ) ;
#260 = ORIENTED_EDGE ( 'NONE', *, *, #6620, .T. ) ;
#261 = CARTESIAN_POINT ( 'NONE',  ( -31.07867591359219617, -26.64985754041175525, 6.700000000000000178 ) ) ;
#262 = VECTOR ( 'NONE', #5403, 1000.000000000000000 ) ;
#264 = EDGE_CURVE ( 'NONE', #4144, #39141, #13023, .T. ) ;
#263 = CARTESIAN_POINT ( 'NONE',  ( -59.00110696496997775, 28.68040728033253473, 6.999999999999999112 ) ) ;
#265 = CARTESIAN_POINT ( 'NONE',  ( 81.68900298540742710, 61.66555023304469785, 1.322881339814628632 ) ) ;
#267 = CARTESIAN_POINT ( 'NONE',  ( 17.02720445904918023, 12.19482440094239273, 2.500000000000000444 ) ) ;
#266 = CARTESIAN_POINT ( 'NONE',  ( 4.319862405889217882, -31.89123791683478970, 6.863805608295729499 ) ) ;
#268 = CARTESIAN_POINT ( 'NONE',  ( 31.47838864403340509, -3.170179483860372738, -5.357953045474171283 ) ) ;
#269 = CARTESIAN_POINT ( 'NONE',  ( 0.000000000000000000, 0.000000000000000000, -2.500000000000000000 ) ) ;
#270 = DIRECTION ( 'NONE',  ( -0.000000000000000000, -0.000000000000000000, -1.000000000000000000 ) ) ;
#271 = CARTESIAN_POINT ( 'NONE',  ( -62.77932549131172379, 36.45562188509706658, 4.736925958236329670 ) ) ;
#272 = CIRCLE ( 'NONE', #25922, 10.00000000000000888 ) ;
#273 = VERTEX_POINT ( 'NONE', #6042 ) ;
#274 = CARTESIAN_POINT ( 'NONE',  ( -0.6367654070295342139, -32.03928316901375695, 6.988553391373221402 ) ) ;
#275 = DIRECTION ( 'NONE',  ( -0.000000000000000000, -0.000000000000000000, 1.000000000000000000 ) ) ;
#276 = PLANE ( 'NONE',  #38056 ) ;
#277 = CARTESIAN_POINT ( 'NONE',  ( 36.44537822125108306, -3.301946079842590365, -5.889618514196052423 ) ) ;
#278 = CARTESIAN_POINT ( 'NONE',  ( 76.65113373804888397, 59.82741887089902377, -3.005488744293225878 ) ) ;
#279 = DIRECTION ( 'NONE',  ( -0.3420201433256601642, -0.9396926207859115365, -0.000000000000000000 ) ) ;
#280 = CARTESIAN_POINT ( 'NONE',  ( 14.75904227071888108, -4.442295602227281037, -2.509903513768624972 ) ) ;
#281 = CARTESIAN_POINT ( 'NONE',  ( -0.6411629333918610341, -32.17099039281331585, 7.754798119455333705 ) ) ;
#282 = CARTESIAN_POINT ( 'NONE',  ( 2.085863669803346365, -32.94801029878254184, 6.979335674598006634 ) ) ;
#283 = CYLINDRICAL_SURFACE ( 'NONE', #22172, 0.09010775117052897965 ) ;
#284 = ADVANCED_FACE ( 'NONE', ( #25588 ), #38132, .T. ) ;
#285 = CARTESIAN_POINT ( 'NONE',  ( -1.450854365928797352, -28.29334945402236556, 7.754798119455333705 ) ) ;
#286 = CARTESIAN_POINT ( 'NONE',  ( 31.57897186779749887, -2.953369379551184171, 5.135060318927252787 ) ) ;
#287 = ORIENTED_EDGE ( 'NONE', *, *, #2540, .F. ) ;
#288 = CARTESIAN_POINT ( 'NONE',  ( -74.92283640148291113, 18.87330372387140187, 9.800414904976365804 ) ) ;
#289 = CARTESIAN_POINT ( 'NONE',  ( 67.79930094788625183, 58.10454462619039617, -3.992148460412407118 ) ) ;
#290 = B_SPLINE_CURVE_WITH_KNOTS ( 'NONE', 3,
 ( #31493, #201, #40324, #12739, #21411, #2492, #33986, #15014, #5760, #12117, #37245, #27977, #18300, #40525, #12334, #9037, #21615, #18711, #24908, #12538, #37442, #9240, #21817, #6170, #3114, #15632, #25110, #4461, #3513, #22239, #20275, #20084, #35749, #37849, #13504, #16983, #1375, #1769, #7523, #29956, #25318, #17182, #6583, #39002, #9654, #29158 ),
 .UNSPECIFIED., .F., .F.,
 ( 4, 2, 1, 1, 2, 2, 1, 1, 1, 2, 2, 2, 1, 1, 1, 2, 2, 1, 2, 2, 2, 2, 1, 1, 2, 2, 1, 2, 4 ),
 ( 0.1281237029900336166, 0.4747198910002122796, 0.4963821527508484044, 0.4990899354696787804, 0.4997668811493873875, 0.5004438268290958280, 0.5017977181885129312, 0.5072132836261800115, 0.5180444145015135060, 0.5613689380028479281, 0.6480179850055166613, 0.7346670320081853944, 0.7454981628835195551, 0.7482059456023534283, 0.7495598369617704204, 0.7498983098016249738, 0.7502367826414796381, 0.7509137283211883007, 0.7563292937588557141, 0.7779915555095239243, 0.7996538172601921346, 0.8104849481355265173, 0.8118388394949429543, 0.8121773123347969525, 0.8123465487547236741, 0.8125157851746505067, 0.8131927308543577260, 0.8159005135731869363, 0.8213160790108455789 ),
 .UNSPECIFIED. ) ;
#291 = VECTOR ( 'NONE', #8251, 1000.000000000000000 ) ;
#292 = ORIENTED_EDGE ( 'NONE', *, *, #32328, .T. ) ;
#293 = AXIS2_PLACEMENT_3D ( 'NONE', #5150, #36441, #8215 ) ;
#294 = CARTESIAN_POINT ( 'NONE',  ( -0.9541984736338051665, -27.30603911067314726, 7.781480525794718162 ) ) ;
#295 = CARTESIAN_POINT ( 'NONE',  ( -28.44874870218064444, -26.64985754041175525, 6.700000000000000178 ) ) ;
#296 = CARTESIAN_POINT ( 'NONE',  ( 23.06570227960076025, 3.126885040524279624, 4.061145912289076954 ) ) ;
#297 = EDGE_CURVE ( 'NONE', #31547, #18087, #3886, .T. ) ;
#298 = ADVANCED_FACE ( 'NONE', ( #28261 ), #85, .F. ) ;
#299 = CARTESIAN_POINT ( 'NONE',  ( 3.540652623597135840, -26.59276059082981547, 6.863784140767622333 ) ) ;
#300 = CARTESIAN_POINT ( 'NONE',  ( -1.499157785959173594, -28.41975916621540321, 7.635761828346577573 ) ) ;
#301 = VERTEX_POINT ( 'NONE', #29083 ) ;
#302 = EDGE_CURVE ( 'NONE', #31037, #37836, #19719, .T. ) ;
#303 = CARTESIAN_POINT ( 'NONE',  ( 23.43463349670878415, 3.790763441738238537, 3.110222249176512133 ) ) ;
#304 = CARTESIAN_POINT ( 'NONE',  ( 2.778259044425222868, -32.89982485500929954, 7.750000000000000888 ) ) ;
#305 = VECTOR ( 'NONE', #27454, 1000.000000000000000 ) ;
#306 = ORIENTED_EDGE ( 'NONE', *, *, #22254, .F. ) ;
#307 = CARTESIAN_POINT ( 'NONE',  ( 27.60344192425479193, 81.15229837709949834, -1.000000000000000000 ) ) ;
#308 = AXIS2_PLACEMENT_3D ( 'NONE', #26975, #18099, #31499 ) ;
#309 = VERTEX_POINT ( 'NONE', #39328 ) ;
#310 = CARTESIAN_POINT ( 'NONE',  ( 80.31443933487477693, 61.76769068803228180, -3.015657119755351889 ) ) ;
#312 = CARTESIAN_POINT ( 'NONE',  ( -1.482088180267139066, -30.76652202637871625, 7.693875151218754205 ) ) ;
#311 = CARTESIAN_POINT ( 'NONE',  ( 21.84880020533123002, 0.3448032378364013772, 8.036168467369821045 ) ) ;
#313 = CARTESIAN_POINT ( 'NONE',  ( 81.74528107327192572, 62.23958694028459604, -2.368810654844693442 ) ) ;
#314 = CARTESIAN_POINT ( 'NONE',  ( 80.80164418317316688, 61.17044828488889152, 1.584170212883420081 ) ) ;
#315 = EDGE_CURVE ( 'NONE', #9594, #14002, #20041, .T. ) ;
#316 = CARTESIAN_POINT ( 'NONE',  ( -20.24874870218063805, -25.49307895267003587, 6.800000000000000711 ) ) ;
#317 = CARTESIAN_POINT ( 'NONE',  ( 4.666500650180242182, -31.42793668606411117, 7.750000000000000888 ) ) ;
#318 = CARTESIAN_POINT ( 'NONE',  ( 22.67874324181232737, -4.030091496876125667, 7.802482278901700319 ) ) ;
#319 = CARTESIAN_POINT ( 'NONE',  ( 5.100040579096636328, -29.61868030101130245, 6.894806418505348589 ) ) ;
#320 = VERTEX_POINT ( 'NONE', #7642 ) ;
#321 = CARTESIAN_POINT ( 'NONE',  ( -75.51466614119452458, 10.05014096851642158, 8.892739820773797987 ) ) ;
#322 = CARTESIAN_POINT ( 'NONE',  ( 21.96835285544658944, 0.2152711931543893065, -7.743667062754403752 ) ) ;
#323 = ORIENTED_EDGE ( 'NONE', *, *, #28033, .F. ) ;
#324 = CIRCLE ( 'NONE', #4910, 0.1000000000000028644 ) ;
#325 = AXIS2_PLACEMENT_3D ( 'NONE', #22553, #3830, #34311 ) ;
#326 = CARTESIAN_POINT ( 'NONE',  ( 1.679836435472961131, -32.96988196360472756, 7.779495906702013741 ) ) ;
#327 = FACE_OUTER_BOUND ( 'NONE', #20175, .T. ) ;
#328 = CARTESIAN_POINT ( 'NONE',  ( 36.87196059928034941, -2.085890912122125407, -5.863601101037241747 ) ) ;
#329 = CYLINDRICAL_SURFACE ( 'NONE', #3480, 2.500000000000000444 ) ;
#330 = CARTESIAN_POINT ( 'NONE',  ( 3.410240285952196970, -32.62386096090719434, 6.880608371227951992 ) ) ;
#331 = DIRECTION ( 'NONE',  ( -0.7660444431189813441, 0.6427876096865353661, -0.000000000000000000 ) ) ;
#332 = CARTESIAN_POINT ( 'NONE',  ( 5.195448342531864050, -29.75585445294578690, 6.921725064902942925 ) ) ;
#333 = CARTESIAN_POINT ( 'NONE',  ( -40.87867591359218977, -26.64985754041175525, 6.700000000000000178 ) ) ;
#334 = LINE ( 'NONE', #37983, #38784 ) ;
#335 = VECTOR ( 'NONE', #17674, 1000.000000000000000 ) ;
#336 = EDGE_CURVE ( 'NONE', #19965, #16079, #3389, .T. ) ;
#337 = DIRECTION ( 'NONE',  ( -0.000000000000000000, -0.000000000000000000, 1.000000000000000000 ) ) ;
#338 = CARTESIAN_POINT ( 'NONE',  ( 30.66378199172083896, -3.777849468416345502, -4.533872787636463286 ) ) ;
#339 = CARTESIAN_POINT ( 'NONE',  ( -18.44874870218064089, -26.64985754041175525, 6.800000000000000711 ) ) ;
#340 = ORIENTED_EDGE ( 'NONE', *, *, #35850, .F. ) ;
#341 = CARTESIAN_POINT ( 'NONE',  ( 67.12475893546654504, 58.13278081555189658, 3.997693602769900156 ) ) ;
#342 = ADVANCED_FACE ( 'NONE', ( #36253 ), #23687, .F. ) ;
#343 = DIRECTION ( 'NONE',  ( 0.7877517966954343809, -0.6159927814537400348, 0.000000000000000000 ) ) ;
#345 = EDGE_CURVE ( 'NONE', #17688, #33823, #20191, .T. ) ;
#344 = CARTESIAN_POINT ( 'NONE',  ( 88.38642666631945133, -2.374919807968325358, 0.2172961577596721761 ) ) ;
#346 = CARTESIAN_POINT ( 'NONE',  ( 2.121967401070180337, -33.04444778638764291, 6.980586498568968068 ) ) ;
#347 = VERTEX_POINT ( 'NONE', #17486 ) ;
#348 = CARTESIAN_POINT ( 'NONE',  ( 24.52494981597524770, 2.752700276650007716, 3.867455811991591386 ) ) ;
#349 =( NAMED_UNIT ( * ) PLANE_ANGLE_UNIT ( ) SI_UNIT ( $, .RADIAN. ) );
#350 = CARTESIAN_POINT ( 'NONE',  ( -72.95330471031414277, 33.71485196875532608, 8.800414904976364028 ) ) ;
#351 = EDGE_CURVE ( 'NONE', #2784, #15795, #11729, .T. ) ;
#352 = CARTESIAN_POINT ( 'NONE',  ( 0.02261628322158271143, -32.52713990352308571, 7.652160403243382980 ) ) ;
#353 = ORIENTED_EDGE ( 'NONE', *, *, #28391, .T. ) ;
#354 = SURFACE_SIDE_STYLE ('',( #15787 ) ) ;
#355 = AXIS2_PLACEMENT_3D ( 'NONE', #34375, #21798, #3297 ) ;
#356 = AXIS2_PLACEMENT_3D ( 'NONE', #19003, #36206, #4906 ) ;
#357 = VERTEX_POINT ( 'NONE', #8227 ) ;
#358 = ORIENTED_EDGE ( 'NONE', *, *, #26602, .T. ) ;
#359 = CARTESIAN_POINT ( 'NONE',  ( 79.50008710437273862, 64.50769319364300713, -3.547878946066220340 ) ) ;
#360 = AXIS2_PLACEMENT_3D ( 'NONE', #5847, #22109, #33859 ) ;
#361 = CARTESIAN_POINT ( 'NONE',  ( -1.698669275463088990, -29.48942424707293242, 7.782034975670477195 ) ) ;
#362 = CARTESIAN_POINT ( 'NONE',  ( 79.01373585440697411, 65.47072129778472060, 2.830664096605183921 ) ) ;
#365 = ORIENTED_EDGE ( 'NONE', *, *, #29479, .F. ) ;
#364 = ORIENTED_EDGE ( 'NONE', *, *, #24881, .F. ) ;
#363 = CARTESIAN_POINT ( 'NONE',  ( -1.688708477085993920, -29.88419193628291382, 7.576089344240128476 ) ) ;
#366 = PLANE ( 'NONE',  #31779 ) ;
#367 =( BOUNDED_SURFACE ( )  B_SPLINE_SURFACE ( 3, 2, ( 
 ( #9527, #37331, #24992 ),
 ( #34282, #3403, #24575 ),
 ( #28067, #3199, #6052 ),
 ( #11995, #40408, #19015 ),
 ( #21902, #34688, #15098 ),
 ( #12423, #34889, #9127 ) ),
 .UNSPECIFIED., .F., .F., .F. ) 
 B_SPLINE_SURFACE_WITH_KNOTS ( ( 4, 2, 4 ),
 ( 3, 3 ),
 ( 0.000000000000000000, 0.001067213068434984691, 0.002134426136869969383 ),
 ( 0.000000000000000000, 1.000000000000000000 ),
 .UNSPECIFIED. ) 
 GEOMETRIC_REPRESENTATION_ITEM ( )  RATIONAL_B_SPLINE_SURFACE ( (
 ( 1.000000000000000000, 0.6872206705711639829, 1.000000000000000000),
 ( 1.000000000000000000, 0.6752582546153387266, 1.000000000000000000),
 ( 1.000000000000000000, 0.6623616715684274014, 1.000000000000000000),
 ( 1.000000000000000000, 0.6342435107462650601, 1.000000000000000000),
 ( 1.000000000000000000, 0.6188407181626371933, 1.000000000000000000),
 ( 1.000000000000000000, 0.6029302108204154242, 1.000000000000000000) ) ) 
 REPRESENTATION_ITEM ( '' )  SURFACE ( )  );
#368 = CARTESIAN_POINT ( 'NONE',  ( -0.5359795030213230227, -32.26226207767182785, 7.750000000000001776 ) ) ;
#369 = CARTESIAN_POINT ( 'NONE',  ( 3.424610526961022305, -26.52410162464354215, 7.660770905198775793 ) ) ;
#370 = CARTESIAN_POINT ( 'NONE',  ( 33.89815560913680059, -5.472034195326516581, 0.3552926572089393775 ) ) ;
#371 = CARTESIAN_POINT ( 'NONE',  ( 22.19574982338894031, 5.228104102381771590, -3.102888934201143201 ) ) ;
#372 = ORIENTED_EDGE ( 'NONE', *, *, #28540, .T. ) ;
#373 = DIRECTION ( 'NONE',  ( 0.3420201433256662704, 0.9396926207859093161, -0.000000000000000000 ) ) ;
#374 = EDGE_LOOP ( 'NONE', ( #7724, #13238, #35896, #104 ) ) ;
#375 = LINE ( 'NONE', #9824, #24005 ) ;
#376 = CARTESIAN_POINT ( 'NONE',  ( 4.296241352401964697, -27.37412594797728715, 7.635761828346577573 ) ) ;
#377 = CARTESIAN_POINT ( 'NONE',  ( -81.11285676435983305, -5.649961960633484104, -4.124376956758348811 ) ) ;
#378 = FACE_OUTER_BOUND ( 'NONE', #3984, .T. ) ;
#379 = CARTESIAN_POINT ( 'NONE',  ( 29.20860690094596634, 2.240472738085125037, 1.050758983225395848 ) ) ;
#380 = CARTESIAN_POINT ( 'NONE',  ( 81.32291525751649885, 62.59435864775880987, 3.036434590848157367 ) ) ;
#381 = CARTESIAN_POINT ( 'NONE',  ( 87.68638643695580015, -2.222987235672965411, -2.753905389729575326 ) ) ;
#382 = CARTESIAN_POINT ( 'NONE',  ( -0.01842261143103093163, -32.61881242066402820, 7.698786668945016842 ) ) ;
#383 = ORIENTED_EDGE ( 'NONE', *, *, #7114, .F. ) ;
#384 = CARTESIAN_POINT ( 'NONE',  ( 4.025803068412391106, -27.08951600530382464, 7.013842709614101167 ) ) ;
#385 = CARTESIAN_POINT ( 'NONE',  ( 24.97673583131591712, 3.396458356181121019, -1.647695864654638909 ) ) ;
#386 = EDGE_CURVE ( 'NONE', #34099, #38151, #20947, .T. ) ;
#387 = AXIS2_PLACEMENT_3D ( 'NONE', #30030, #29821, #1845 ) ;
#388 = AXIS2_PLACEMENT_3D ( 'NONE', #3065, #40471, #13104 ) ;
#389 = CARTESIAN_POINT ( 'NONE',  ( 1.750706304578934613, -26.17028763529686941, 7.785868773668302545 ) ) ;
#390 = CARTESIAN_POINT ( 'NONE',  ( -19.07867591359219972, -24.55319635012989110, 6.700000000000000178 ) ) ;
#391 = CARTESIAN_POINT ( 'NONE',  ( 25.11437021580303863, 164.7550792202006562, -1.000000000000000000 ) ) ;
#392 = DIRECTION ( 'NONE',  ( -1.000000000000000000, 0.000000000000000000, 0.000000000000000000 ) ) ;
#393 = VERTEX_POINT ( 'NONE', #4566 ) ;
#394 = CARTESIAN_POINT ( 'NONE',  ( 21.25246165869702253, 3.318379160498120761, 3.523358653204108570 ) ) ;
#395 = CIRCLE ( 'NONE', #29328, 6.406751979251626317 ) ;
#396 = CARTESIAN_POINT ( 'NONE',  ( 86.26657670271889344, 1.459011185482768314, -4.895973709007312991 ) ) ;
#397 = ORIENTED_EDGE ( 'NONE', *, *, #11518, .F. ) ;
#399 = CARTESIAN_POINT ( 'NONE',  ( 0.000000000000000000, -0.6000000000000003109, 3.730072921939604047 ) ) ;
#398 = CARTESIAN_POINT ( 'NONE',  ( 79.64354988242321554, 65.32830775696902492, -3.122598816540614663 ) ) ;
#400 = CARTESIAN_POINT ( 'NONE',  ( 5.197301300333582397, -29.56993018336890700, 7.767301406056524193 ) ) ;
#401 = CARTESIAN_POINT ( 'NONE',  ( 4.298799322723926508, -31.91476908534313850, 7.750000000000000888 ) ) ;
#402 = ORIENTED_EDGE ( 'NONE', *, *, #15855, .F. ) ;
#403 = CARTESIAN_POINT ( 'NONE',  ( -10.97867591359219475, -24.55319635012989110, 6.800000000000000711 ) ) ;
#404 = EDGE_CURVE ( 'NONE', #16945, #2799, #36230, .T. ) ;
#405 = ORIENTED_EDGE ( 'NONE', *, *, #6491, .T. ) ;
#406 = CARTESIAN_POINT ( 'NONE',  ( 0.9213240864078056092, -26.64985754041175525, 6.800000000000000711 ) ) ;
#407 = EDGE_CURVE ( 'NONE', #9686, #33055, #7841, .T. ) ;
#408 = VERTEX_POINT ( 'NONE', #26392 ) ;
#409 = CARTESIAN_POINT ( 'NONE',  ( 78.68112288793685138, 66.00442204571392324, -1.607835478472330548 ) ) ;
#410 = DIRECTION ( 'NONE',  ( 0.000000000000000000, -0.5555716052200797561, 0.8314686954258614371 ) ) ;
#411 = CARTESIAN_POINT ( 'NONE',  ( 23.70424450760806323, 1.818959193472196922, 4.681574839466135174 ) ) ;
#412 = CARTESIAN_POINT ( 'NONE',  ( 81.67793621607867749, 64.59267988934871596, -2.776691787112390397 ) ) ;
#413 = CIRCLE ( 'NONE', #30646, 12.38600677260393113 ) ;
#414 = VECTOR ( 'NONE', #27211, 1000.000000000000000 ) ;
#415 = CARTESIAN_POINT ( 'NONE',  ( 4.749297472835599443, -31.28869828601962766, 7.697032948437507294 ) ) ;
#417 = CARTESIAN_POINT ( 'NONE',  ( 85.87571968583984017, 1.898040338034475472, 4.108051227457266918 ) ) ;
#416 = CARTESIAN_POINT ( 'NONE',  ( 4.612110029931828059, -31.32547828874780649, 6.880147297696984410 ) ) ;
#418 = CARTESIAN_POINT ( 'NONE',  ( 4.390205000165592786, -31.80932647847912875, 7.635761828346570468 ) ) ;
#419 = CARTESIAN_POINT ( 'NONE',  ( 0.6185823884176052667, -26.24155567332487493, 7.754798119455333705 ) ) ;
#420 = CARTESIAN_POINT ( 'NONE',  ( 72.46216784064273497, 59.07243765930573431, 3.784404822033881288 ) ) ;
#421 = CARTESIAN_POINT ( 'NONE',  ( 22.18398091595247124, 4.302725770086238022, -3.814574538098304046 ) ) ;
#422 = VERTEX_POINT ( 'NONE', #38922 ) ;
#423 = VECTOR ( 'NONE', #27841, 1000.000000000000000 ) ;
#424 = EDGE_LOOP ( 'NONE', ( #10663, #22952, #33559, #23632 ) ) ;
#425 = CARTESIAN_POINT ( 'NONE',  ( 21.85643539959775339, -6.841675198209371977, -12.88699694080538549 ) ) ;
#426 = CARTESIAN_POINT ( 'NONE',  ( 3.444423122666314896, -26.53698764147170408, 7.762796336881262249 ) ) ;
#427 = CARTESIAN_POINT ( 'NONE',  ( 53.63043182916395324, -5.819003020824450978, 6.000000000000000888 ) ) ;
#428 = CARTESIAN_POINT ( 'NONE',  ( 81.28907188958037011, 64.38987696229567348, 3.179853676208927116 ) ) ;
#429 = CARTESIAN_POINT ( 'NONE',  ( 85.06055580697953644, 2.762169973306998205, -2.784126402610546780 ) ) ;
#430 = EDGE_LOOP ( 'NONE', ( #38499, #2239, #5855, #4124 ) ) ;
#431 = CARTESIAN_POINT ( 'NONE',  ( 14.69558838330753581, 12.33286846116140367, 2.499999999999996891 ) ) ;
#432 = CARTESIAN_POINT ( 'NONE',  ( 14.98566736410303868, -6.090311521776418324, 2.529564007200721054 ) ) ;
#433 = CARTESIAN_POINT ( 'NONE',  ( 33.62870426848748195, -1.228885055514358005, -5.454970633020429283 ) ) ;
#434 = PLANE ( 'NONE',  #17404 ) ;
#435 = CARTESIAN_POINT ( 'NONE',  ( -1.345091088867315765, -27.84509849030786555, 7.730015791551950954 ) ) ;
#436 = CARTESIAN_POINT ( 'NONE',  ( -74.18164544079856171, -2.036837289978346455, 10.73485733915913443 ) ) ;
#437 = EDGE_LOOP ( 'NONE', ( #28811, #8609, #22831, #13291, #24960 ) ) ;
#438 = DIRECTION ( 'NONE',  ( 1.000000000000000000, 0.000000000000000000, 0.000000000000000000 ) ) ;
#439 = FACE_OUTER_BOUND ( 'NONE', #33105, .T. ) ;
#440 = CARTESIAN_POINT ( 'NONE',  ( 33.46455574127770660, -3.089180930156425475, 5.429351285402141514 ) ) ;
#441 = ORIENTED_EDGE ( 'NONE', *, *, #31035, .T. ) ;
#442 = ORIENTED_EDGE ( 'NONE', *, *, #39133, .F. ) ;
#443 = CARTESIAN_POINT ( 'NONE',  ( 36.13178710339454369, -1.532094116269871797, 5.644416983045655201 ) ) ;
#444 = DIRECTION ( 'NONE',  ( 1.000000000000000000, 0.000000000000000000, 0.000000000000000000 ) ) ;
#445 = VECTOR ( 'NONE', #7320, 1000.000000000000000 ) ;
#446 = VERTEX_POINT ( 'NONE', #1684 ) ;
#447 = CARTESIAN_POINT ( 'NONE',  ( 66.42990020876152357, 57.76860247958598649, -4.000000000000009770 ) ) ;
#448 = VECTOR ( 'NONE', #1284, 1000.000000000000000 ) ;
#449 = EDGE_CURVE ( 'NONE', #15211, #25138, #33471, .T. ) ;
#450 = ORIENTED_EDGE ( 'NONE', *, *, #24702, .T. ) ;
#452 = EDGE_CURVE ( 'NONE', #38236, #38151, #37379, .T. ) ;
#451 = CARTESIAN_POINT ( 'NONE',  ( -80.82841455951717080, 11.46672392024627385, -1.471659699228122786 ) ) ;
#453 = CARTESIAN_POINT ( 'NONE',  ( 4.960875347057841722, -28.60596118244303199, 6.969307238440507035 ) ) ;
#454 = CARTESIAN_POINT ( 'NONE',  ( 8.290806648384990041, -10.90558813203967148, 6.000000000000000000 ) ) ;
#455 = ORIENTED_EDGE ( 'NONE', *, *, #8758, .F. ) ;
#456 = FACE_BOUND ( 'NONE', #19493, .T. ) ;
#457 = ORIENTED_EDGE ( 'NONE', *, *, #19911, .F. ) ;
#458 = CARTESIAN_POINT ( 'NONE',  ( 22.03184786808944651, 5.415838924531075627, 3.191312399929147059 ) ) ;
#459 = CARTESIAN_POINT ( 'NONE',  ( 81.58705100058459436, 65.69127060146935548, -1.444831904610020645 ) ) ;
#460 = CARTESIAN_POINT ( 'NONE',  ( 81.07747211222739736, 61.58128768033702727, 2.227525437860359947 ) ) ;
#461 = CARTESIAN_POINT ( 'NONE',  ( -1.749742372765484610, -28.98121160874161006, 7.747520101777647383 ) ) ;
#462 = VERTEX_POINT ( 'NONE', #32769 ) ;
#463 = VERTEX_POINT ( 'NONE', #26182 ) ;
#464 = CARTESIAN_POINT ( 'NONE',  ( 75.27909492816711179, 60.48191808705185224, -3.786335567263138469 ) ) ;
#466 = CARTESIAN_POINT ( 'NONE',  ( 1.123253381486050140, -26.11784194350818211, 6.894806418505347700 ) ) ;
#465 = CARTESIAN_POINT ( 'NONE',  ( 2.480201502389029589, -26.15790714162507413, 7.006248344249653037 ) ) ;
#467 = CARTESIAN_POINT ( 'NONE',  ( 19.96934150597399693, 6.745664378534328876, -3.285863046672279353 ) ) ;
#468 = CARTESIAN_POINT ( 'NONE',  ( 79.68360889523899004, 65.64663933523164019, -2.797238656122822409 ) ) ;
#469 = DIRECTION ( 'NONE',  ( 1.000000000000000000, 0.000000000000000000, -0.000000000000000000 ) ) ;
#470 = CARTESIAN_POINT ( 'NONE',  ( 75.74534653887745606, 63.84344576921726144, 2.970791854430534062 ) ) ;
#471 = ORIENTED_EDGE ( 'NONE', *, *, #26054, .F. ) ;
#472 = CARTESIAN_POINT ( 'NONE',  ( 7.021324086407807030, -26.64985754041175525, 6.800000000000000711 ) ) ;
#473 = CARTESIAN_POINT ( 'NONE',  ( -70.92837670882107659, 26.72470171467712063, 0.000000000000000000 ) ) ;
#474 = B_SPLINE_CURVE_WITH_KNOTS ( 'NONE', 3,
 ( #7514, #16768, #32255, #7119, #4054, #35545, #13493, #35147, #38993, #16570, #10598, #20074, #26464, #32851, #19480, #29350, #16376, #29150, #32651, #13092, #19682, #7315, #32054, #38600, #4451, #22979, #28950, #10792, #32446, #13285, #25857, #25653, #3860, #1170, #753, #1365 ),
 .UNSPECIFIED., .F., .F.,
 ( 4, 2, 2, 2, 2, 2, 2, 2, 2, 2, 2, 2, 2, 2, 2, 2, 2, 4 ),
 ( 0.07948797976893491601, 0.08078140541914788364, 0.08207483106936083739, 0.08336825671957380501, 0.08466168236978677264, 0.08595510801999974027, 0.08724853367021269401, 0.08854195932042566164, 0.08983538497063862927, 0.09112881062085158301, 0.09242223627106455064, 0.09371566192127751826, 0.09500908757149048589, 0.09630251322170343964, 0.09759593887191640726, 0.09888936452212937489, 0.09953607734723585176, 0.1001827901723423425 ),
 .UNSPECIFIED. ) ;
#475 = CARTESIAN_POINT ( 'NONE',  ( 82.09661666296835847, 62.69434707785895000, 2.190303691588293855 ) ) ;
#477 = CARTESIAN_POINT ( 'NONE',  ( -36.44874870218064444, -26.64985754041175525, 6.800000000000000711 ) ) ;
#476 = CARTESIAN_POINT ( 'NONE',  ( -0.1957518678886271957, -32.51180877674722325, 7.011627023500184741 ) ) ;
#478 = CARTESIAN_POINT ( 'NONE',  ( 26.73479038929921359, 2.133517298515754668, 4.055905576634827092 ) ) ;
#479 = CIRCLE ( 'NONE', #7686, 6.329987104167475565 ) ;
#480 = EDGE_CURVE ( 'NONE', #34939, #11908, #22301, .T. ) ;
#481 = CARTESIAN_POINT ( 'NONE',  ( -1.421733872515562824, -31.15181216911474493, 6.971170733404102648 ) ) ;
#482 = VECTOR ( 'NONE', #26893, 1000.000000000000000 ) ;
#483 = CARTESIAN_POINT ( 'NONE',  ( 3.559755418260376114, -26.72339534466646427, 7.013842709614101167 ) ) ;
#484 = AXIS2_PLACEMENT_3D ( 'NONE', #25294, #37829, #22816 ) ;
#485 = FACE_OUTER_BOUND ( 'NONE', #18032, .T. ) ;
#486 = VERTEX_POINT ( 'NONE', #10706 ) ;
#487 = CARTESIAN_POINT ( 'NONE',  ( -0.6086181687031891885, -32.06563633890338139, 6.876076431790004939 ) ) ;
#488 = FACE_OUTER_BOUND ( 'NONE', #13400, .T. ) ;
#489 = LINE ( 'NONE', #19409, #17633 ) ;
#490 = CARTESIAN_POINT ( 'NONE',  ( 30.66842703005120185, 0.2949493320676357944, -4.962900476310909248 ) ) ;
#491 = CARTESIAN_POINT ( 'NONE',  ( 2.850561110411099275, -26.37038230420113649, 7.635761828346577573 ) ) ;
#492 = CARTESIAN_POINT ( 'NONE',  ( 3.121324086407806231, -24.55319635012989110, 6.800000000000000711 ) ) ;
#493 = DIRECTION ( 'NONE',  ( -0.000000000000000000, -0.000000000000000000, -1.000000000000000000 ) ) ;
#494 = CARTESIAN_POINT ( 'NONE',  ( 1.123253381486050140, -26.11784194350818211, 6.894806418505347700 ) ) ;
#495 = CARTESIAN_POINT ( 'NONE',  ( 22.49821043992852410, -9.358482552309803637, -2.500000000000000000 ) ) ;
#496 = EDGE_CURVE ( 'NONE', #31349, #11061, #19543, .T. ) ;
#497 = CARTESIAN_POINT ( 'NONE',  ( 21.89440445940014257, -12.98914838499760549, 2.499999999999999556 ) ) ;
#498 = ORIENTED_EDGE ( 'NONE', *, *, #29293, .F. ) ;
#499 = ORIENTED_EDGE ( 'NONE', *, *, #31706, .F. ) ;
#500 = CARTESIAN_POINT ( 'NONE',  ( 3.037211893591657219, -26.44376520468768632, 7.013842709614101167 ) ) ;
#501 = CARTESIAN_POINT ( 'NONE',  ( 68.15116243724637002, 58.05457144382717871, -3.974537232972704892 ) ) ;
#502 = CARTESIAN_POINT ( 'NONE',  ( 2.926619159346142141, -26.29176571567377607, 6.894806418505347700 ) ) ;
#503 = VECTOR ( 'NONE', #9003, 1000.000000000000000 ) ;
#504 = ORIENTED_EDGE ( 'NONE', *, *, #40555, .F. ) ;
#505 = CARTESIAN_POINT ( 'NONE',  ( -0.9006701161811203615, -27.22837715677322379, 7.754798119455333705 ) ) ;
#507 = EDGE_CURVE ( 'NONE', #30375, #12399, #25450, .T. ) ;
#506 = CARTESIAN_POINT ( 'NONE',  ( 30.31548945822549967, -3.037691172068890388, 4.938150023066174121 ) ) ;
#508 = CARTESIAN_POINT ( 'NONE',  ( 21.85677098809243546, 3.668375465701176896, 4.582786065448858359 ) ) ;
#509 = CARTESIAN_POINT ( 'NONE',  ( 3.531565352711682149, -26.58716268337259336, 6.863805608295729499 ) ) ;
#510 = CIRCLE ( 'NONE', #40591, 0.1000000000000028644 ) ;
#511 = AXIS2_PLACEMENT_3D ( 'NONE', #33114, #5508, #36395 ) ;
#512 = DIRECTION ( 'NONE',  ( 1.000000000000000000, -0.000000000000000000, 0.000000000000000000 ) ) ;
#513 = VERTEX_POINT ( 'NONE', #23285 ) ;
#514 = CARTESIAN_POINT ( 'NONE',  ( 24.40645114936911853, 3.164002126677583959, 3.269146773302918696 ) ) ;
#515 = FACE_OUTER_BOUND ( 'NONE', #22231, .T. ) ;
#516 = CARTESIAN_POINT ( 'NONE',  ( 79.64354988242320132, 65.32830775696902492, 3.122598816540617328 ) ) ;
#517 = CARTESIAN_POINT ( 'NONE',  ( 1.105923466014343548, -33.01907637181788147, 7.635761828346575797 ) ) ;
#518 = EDGE_LOOP ( 'NONE', ( #5397, #1910, #16353, #3651, #24693, #26966, #34035 ) ) ;
#519 = CARTESIAN_POINT ( 'NONE',  ( 79.72787136111028872, 62.61980214589642202, -3.627744115730416219 ) ) ;
#521 = CARTESIAN_POINT ( 'NONE',  ( -1.668836025287037783, -30.02645519570809185, 6.865312560952603782 ) ) ;
#520 = CARTESIAN_POINT ( 'NONE',  ( 24.12512118317265930, 0.5285243960147255615, 5.092426130416875196 ) ) ;
#522 = CARTESIAN_POINT ( 'NONE',  ( 81.36150051724392540, 64.03901721961885585, -3.243459512787965515 ) ) ;
#523 = CARTESIAN_POINT ( 'NONE',  ( 78.40723131619293440, 65.41550730244513545, 2.551437666014014560 ) ) ;
#524 = CARTESIAN_POINT ( 'NONE',  ( -1.629071066768614129, -30.64913839573838317, 7.751599049952198506 ) ) ;
#525 = CARTESIAN_POINT ( 'NONE',  ( -28.44874870218064444, -26.64985754041175525, 6.800000000000000711 ) ) ;
#526 = CARTESIAN_POINT ( 'NONE',  ( -64.08758708074093136, 42.86825253631505461, 2.416740206856579753 ) ) ;
#527 = CARTESIAN_POINT ( 'NONE',  ( 24.99455384622441301, -2.608472216378299180, -6.027016329390949778 ) ) ;
#528 = EDGE_CURVE ( 'NONE', #40182, #12066, #7030, .T. ) ;
#529 = DIRECTION ( 'NONE',  ( 0.000000000000000000, 1.000000000000000000, 0.000000000000000000 ) ) ;
#530 = VERTEX_POINT ( 'NONE', #38113 ) ;
#531 = CARTESIAN_POINT ( 'NONE',  ( -72.64281072204887835, 6.529755665022496380, 9.854046603058758791 ) ) ;
#532 = CARTESIAN_POINT ( 'NONE',  ( 20.40287464734031531, 10.75613383782063970, 2.500000000000000000 ) ) ;
#533 = EDGE_LOOP ( 'NONE', ( #33702, #7118, #20763, #32067, #12346, #35016, #16297 ) ) ;
#534 = DIRECTION ( 'NONE',  ( 0.000000000000000000, 1.000000000000000000, 0.000000000000000000 ) ) ;
#535 = VECTOR ( 'NONE', #9009, 1000.000000000000114 ) ;
#536 = CARTESIAN_POINT ( 'NONE',  ( -0.3903772972505400451, -26.88875661219547553, 7.754798119455333705 ) ) ;
#537 = CARTESIAN_POINT ( 'NONE',  ( 33.45805083109267741, -3.829395647111636602, -5.093820334410049000 ) ) ;
#538 = CARTESIAN_POINT ( 'NONE',  ( 27.81621687972488033, 1.844493567162720948, -3.906584444767790654 ) ) ;
#539 = PLANE ( 'NONE',  #36059 ) ;
#540 = CARTESIAN_POINT ( 'NONE',  ( 16.53760894254279634, 10.03315526601902619, 2.737223308667571242 ) ) ;
#541 = CARTESIAN_POINT ( 'NONE',  ( 0.7201709579117279159, -51.60714625320436255, 6.000000000000000000 ) ) ;
#542 = CARTESIAN_POINT ( 'NONE',  ( 5.123097946374971734, -30.30141562551846235, 7.750000000000000888 ) ) ;
#543 = EDGE_CURVE ( 'NONE', #29781, #29208, #27533, .T. ) ;
#544 = AXIS2_PLACEMENT_3D ( 'NONE', #1556, #29351, #16977 ) ;
#545 = VECTOR ( 'NONE', #23483, 1000.000000000000114 ) ;
#546 = ADVANCED_FACE ( 'NONE', ( #1471 ), #22891, .T. ) ;
#547 = CARTESIAN_POINT ( 'NONE',  ( -31.07867591359219617, -26.64985754041175525, 6.700000000000000178 ) ) ;
#548 = CARTESIAN_POINT ( 'NONE',  ( 35.51269972589511070, -1.199312315519171834, -5.486990563529896114 ) ) ;
#549 = CARTESIAN_POINT ( 'NONE',  ( 3.364053381479577443, -33.98248085747043490, 7.695279973900954751 ) ) ;
#550 = ORIENTED_EDGE ( 'NONE', *, *, #14859, .T. ) ;
#551 = CARTESIAN_POINT ( 'NONE',  ( 66.74992980603514070, 57.79401841677491092, 3.997717836767872512 ) ) ;
#552 = CARTESIAN_POINT ( 'NONE',  ( 2.274693159464038050, -26.11736939636621813, 7.714178352335855138 ) ) ;
#553 = CARTESIAN_POINT ( 'NONE',  ( 87.30284416890829391, -1.044652313481390760, -5.185858056390752147 ) ) ;
#554 = ADVANCED_FACE ( 'NONE', ( #16885 ), #25774, .F. ) ;
#555 = VECTOR ( 'NONE', #26285, 1000.000000000000000 ) ;
#556 = ORIENTED_EDGE ( 'NONE', *, *, #29793, .F. ) ;
#557 = CARTESIAN_POINT ( 'NONE',  ( 24.53045243809206255, 2.749270639064558708, 3.869256640630484689 ) ) ;
#558 = DIRECTION ( 'NONE',  ( 1.000000000000000000, 0.000000000000000000, 0.000000000000000000 ) ) ;
#559 = DIRECTION ( 'NONE',  ( 0.000000000000000000, 1.000000000000000000, 0.000000000000000000 ) ) ;
#560 = CARTESIAN_POINT ( 'NONE',  ( 1.187115290808829382, -26.11501310037670009, 7.776484688137383472 ) ) ;
#561 = VERTEX_POINT ( 'NONE', #26383 ) ;
#562 = SURFACE_STYLE_USAGE ( .BOTH. , #354 ) ;
#563 = CIRCLE ( 'NONE', #18272, 0.1000000000000028644 ) ;
#564 = ORIENTED_EDGE ( 'NONE', *, *, #36948, .F. ) ;
#565 = CARTESIAN_POINT ( 'NONE',  ( 80.74625401487976717, 62.12052764141679262, -3.052025427726072326 ) ) ;
#566 = CARTESIAN_POINT ( 'NONE',  ( -0.9271279775035500270, -27.41211907304282036, 7.695279973900954751 ) ) ;
#567 = CARTESIAN_POINT ( 'NONE',  ( 81.02662073326128223, 61.25180701697230035, 1.364493914842159539 ) ) ;
#569 = ORIENTED_EDGE ( 'NONE', *, *, #7114, .T. ) ;
#568 = ORIENTED_EDGE ( 'NONE', *, *, #13622, .T. ) ;
#570 = AXIS2_PLACEMENT_3D ( 'NONE', #16960, #5023, #19858 ) ;
#571 = ADVANCED_FACE ( 'NONE', ( #22696 ), #35460, .T. ) ;
#572 = CARTESIAN_POINT ( 'NONE',  ( -58.88620717884589340, 28.60568668665318270, 6.105166739222743111 ) ) ;
#573 = CARTESIAN_POINT ( 'NONE',  ( 1.043287501142265317, -33.00769343636290643, 6.878641987404677138 ) ) ;
#574 = CARTESIAN_POINT ( 'NONE',  ( -1.791168270219405168, -29.47546713279042052, 7.776484688137385248 ) ) ;
#575 = CARTESIAN_POINT ( 'NONE',  ( 33.79783626363753513, -4.901490921675078383, -3.331131011404923736 ) ) ;
#576 = CARTESIAN_POINT ( 'NONE',  ( 21.84698693888098120, 5.866571965567933589, -3.176918204583274452 ) ) ;
#577 = ORIENTED_EDGE ( 'NONE', *, *, #16277, .T. ) ;
#578 = DIRECTION ( 'NONE',  ( -0.000000000000000000, -0.000000000000000000, 1.000000000000000000 ) ) ;
#579 = VERTEX_POINT ( 'NONE', #22497 ) ;
#580 = CARTESIAN_POINT ( 'NONE',  ( 2.910139986571841586, -32.85421171754464353, 7.635761828346577573 ) ) ;
#581 = CARTESIAN_POINT ( 'NONE',  ( -0.5918003806487183160, -32.19643581148406497, 7.784725160561907664 ) ) ;
#582 = CARTESIAN_POINT ( 'NONE',  ( -81.25348608327379907, -5.644728239778403989, -3.708980196009161290 ) ) ;
#583 = DIRECTION ( 'NONE',  ( -0.7541618601367610086, 0.000000000000000000, -0.6566885781822769941 ) ) ;
#584 = FACE_OUTER_BOUND ( 'NONE', #9272, .T. ) ;
#585 = CARTESIAN_POINT ( 'NONE',  ( 79.76270496343317973, 65.40180735727545880, 3.071811904357677037 ) ) ;
#586 = CARTESIAN_POINT ( 'NONE',  ( 87.11462257552980759, -1.147413441766115039, -5.140310012396687611 ) ) ;
#587 = CARTESIAN_POINT ( 'NONE',  ( -0.5766758124320290335, -26.91192889271322031, 7.700536657684223130 ) ) ;
#588 = CARTESIAN_POINT ( 'NONE',  ( 2.931185808669444448, -32.84638282411071941, 7.695279973900954751 ) ) ;
#589 = CARTESIAN_POINT ( 'NONE',  ( 4.585610243088643401, -31.36868105187616607, 7.761597726988854085 ) ) ;
#590 = ADVANCED_FACE ( 'NONE', ( #35261 ), #24902, .T. ) ;
#591 = EDGE_CURVE ( 'NONE', #40022, #24258, #30271, .T. ) ;
#592 = LINE ( 'NONE', #16805, #19092 ) ;
#593 = CARTESIAN_POINT ( 'NONE',  ( -0.3224798742589583544, -26.83716377573245637, 6.979335674598003969 ) ) ;
#594 = CARTESIAN_POINT ( 'NONE',  ( -26.87867591359219333, -26.64985754041175525, 6.700000000000000178 ) ) ;
#595 = CARTESIAN_POINT ( 'NONE',  ( 69.29807964942261833, 58.55307042757259950, 3.976370928559292750 ) ) ;
#596 = CARTESIAN_POINT ( 'NONE',  ( 36.91143285253476591, -2.638629310656217530, 5.967319821651744682 ) ) ;
#597 = CARTESIAN_POINT ( 'NONE',  ( 72.90994289418092933, 61.20204674871914818, -3.824679913472085246 ) ) ;
#598 = B_SPLINE_CURVE_WITH_KNOTS ( 'NONE', 3,
 ( #2240, #37206, #5108, #40291 ),
 .UNSPECIFIED., .F., .F.,
 ( 4, 4 ),
 ( 0.000000000000000000, 6.391136169993505180E-06 ),
 .UNSPECIFIED. ) ;
#599 = CARTESIAN_POINT ( 'NONE',  ( 87.87162303905448368, -0.3438530395839958231, 3.959040383187740542 ) ) ;
#600 = ORIENTED_EDGE ( 'NONE', *, *, #11873, .T. ) ;
#601 = CARTESIAN_POINT ( 'NONE',  ( 14.61802081865034530, -4.584627643820613052, 2.500000000000000000 ) ) ;
#602 = CARTESIAN_POINT ( 'NONE',  ( -69.43819311319896315, -46.91958326716831351, 9.888363374916961490 ) ) ;
#603 = ORIENTED_EDGE ( 'NONE', *, *, #22140, .F. ) ;
#604 = CARTESIAN_POINT ( 'NONE',  ( -1.625093378867604521, -28.86200076037926721, 7.757178535559534183 ) ) ;
#605 = ORIENTED_EDGE ( 'NONE', *, *, #39024, .T. ) ;
#606 = CARTESIAN_POINT ( 'NONE',  ( -74.34312302644391934, -4.176925768793524618, 9.403213700939037523 ) ) ;
#607 = ORIENTED_EDGE ( 'NONE', *, *, #26724, .T. ) ;
#608 = VECTOR ( 'NONE', #5163, 1000.000000000000000 ) ;
#609 = CARTESIAN_POINT ( 'NONE',  ( 80.08517677095778708, 64.13476336867732641, -3.668443954219269720 ) ) ;
#610 =( BOUNDED_SURFACE ( )  B_SPLINE_SURFACE ( 3, 2, ( 
 ( #27283, #33689, #29569 ),
 ( #11415, #17802, #7936 ),
 ( #2192, #24196, #39423 ),
 ( #20486, #1385, #20907 ),
 ( #33070, #11616, #10817 ),
 ( #23392, #32870, #8123 ),
 ( #23982, #14709, #17593 ),
 ( #36357, #35958, #20286 ),
 ( #4659, #14512, #17387 ),
 ( #26688, #11213, #36755 ),
 ( #1994, #8331, #33493 ),
 ( #17195, #39221, #4853 ),
 ( #39849, #30387, #30172 ),
 ( #1782, #29763, #21121 ),
 ( #1577, #11012, #14109 ),
 ( #23593, #33279, #14311 ),
 ( #26880, #23778, #20696 ),
 ( #5059, #27086, #39632 ) ),
 .UNSPECIFIED., .F., .F., .T. ) 
 B_SPLINE_SURFACE_WITH_KNOTS ( ( 4, 2, 2, 2, 2, 2, 2, 2, 4 ),
 ( 3, 3 ),
 ( 0.000000000000000000, 9.251198296377863305E-05, 0.0001850239659275572661, 0.0003700479318551145322, 0.0005550718977826718525, 0.0006475838807464504585, 0.0006938398722283398157, 0.0007169678679692844401, 0.0007400958637102290644 ),
 ( 0.000000000000000000, 1.000000000000000000 ),
 .UNSPECIFIED. ) 
 GEOMETRIC_REPRESENTATION_ITEM ( )  RATIONAL_B_SPLINE_SURFACE ( (
 ( 1.000000000000000000, 0.9970051441236916778, 1.000000000000000000),
 ( 1.000000000000000000, 0.9970374898934499797, 1.000000000000000000),
 ( 1.000000000000000000, 0.9972378587227352931, 1.000000000000000000),
 ( 1.000000000000000000, 0.9976285232392927416, 1.000000000000000000),
 ( 1.000000000000000000, 0.9978377992949450936, 1.000000000000000000),
 ( 1.000000000000000000, 0.9984458866281191725, 1.000000000000000000),
 ( 1.000000000000000000, 0.9988290234017360714, 1.000000000000000000),
 ( 1.000000000000000000, 0.9994403397046758286, 1.000000000000000000),
 ( 1.000000000000000000, 0.9996688303162680755, 1.000000000000000000),
 ( 1.000000000000000000, 0.9998817225008336251, 1.000000000000000000),
 ( 1.000000000000000000, 0.9999314634536117241, 1.000000000000000000),
 ( 1.000000000000000000, 0.9999767510700310336, 1.000000000000000000),
 ( 1.000000000000000000, 0.9999869665867011648, 1.000000000000000000),
 ( 1.000000000000000000, 0.9999959687235325800, 1.000000000000000000),
 ( 1.000000000000000000, 0.9999979380867456413, 1.000000000000000000),
 ( 1.000000000000000000, 0.9999998520708384131, 1.000000000000000000),
 ( 1.000000000000000000, 0.9999995175495077770, 1.000000000000000000),
 ( 1.000000000000000000, 0.9999995739621224677, 1.000000000000000000) ) ) 
 REPRESENTATION_ITEM ( '' )  SURFACE ( )  );
#611 = CARTESIAN_POINT ( 'NONE',  ( -71.90198294515647603, -0.5205283187954542479, 5.920697336060230853 ) ) ;
#612 = B_SPLINE_CURVE_WITH_KNOTS ( 'NONE', 3,
 ( #9768, #21164, #13060, #34714, #9561, #5509, #17845, #2236, #31810, #18829, #11664, #30427, #25622, #3019, #6493, #15941, #14757, #38165, #28506 ),
 .UNSPECIFIED., .F., .F.,
 ( 4, 3, 3, 3, 3, 3, 4 ),
 ( 0.000000000000000000, 2.546128104244683795E-05, 5.711050680483705015E-05, 8.113074941675759084E-05, 0.0001053129305727034461, 0.0001360598016347089778, 0.0001612931755702011070 ),
 .UNSPECIFIED. ) ;
#613 = CARTESIAN_POINT ( 'NONE',  ( 25.37055851336592838, 2.296153116583149689, 4.076656671453694258 ) ) ;
#615 = VERTEX_POINT ( 'NONE', #39728 ) ;
#614 = VERTEX_POINT ( 'NONE', #36444 ) ;
#616 = CARTESIAN_POINT ( 'NONE',  ( 4.734418770087374106, -28.03542604781803504, 6.895222827070020877 ) ) ;
#618 = DIRECTION ( 'NONE',  ( -0.000000000000000000, -0.000000000000000000, -1.000000000000000000 ) ) ;
#617 = CARTESIAN_POINT ( 'NONE',  ( -59.01448254578837549, 27.97260867553151442, -6.241456863628584095 ) ) ;
#619 = DIRECTION ( 'NONE',  ( 0.000000000000000000, 0.000000000000000000, -1.000000000000000000 ) ) ;
#620 = CARTESIAN_POINT ( 'NONE',  ( -64.08758708074093136, 43.28737448534269561, -1.986914326913568507 ) ) ;
#621 = CARTESIAN_POINT ( 'NONE',  ( 71.06822368831490166, 59.17031991972731930, 3.954977122261625233 ) ) ;
#622 = CARTESIAN_POINT ( 'NONE',  ( 24.35698045111728760, 2.890171444508740084, -3.780454612355467425 ) ) ;
#623 = EDGE_LOOP ( 'NONE', ( #17672, #40325, #5137, #17035, #31443 ) ) ;
#624 = EDGE_CURVE ( 'NONE', #9599, #28854, #17535, .T. ) ;
#625 = EDGE_LOOP ( 'NONE', ( #4883, #27978 ) ) ;
#626 = VECTOR ( 'NONE', #14878, 1000.000000000000114 ) ;
#627 = CARTESIAN_POINT ( 'NONE',  ( 21.85643539959780313, -7.722266916079949972, 9.821539774841749448 ) ) ;
#628 = EDGE_CURVE ( 'NONE', #3707, #4251, #20578, .T. ) ;
#629 = CARTESIAN_POINT ( 'NONE',  ( 21.83106932671409339, 5.061056560966107121, -3.908462188292611383 ) ) ;
#630 = EDGE_LOOP ( 'NONE', ( #15162, #24602, #9016, #12961 ) ) ;
#631 = CARTESIAN_POINT ( 'NONE',  ( 2.338742698598151204, -26.12863595720122234, 6.894806418505347700 ) ) ;
#632 = CARTESIAN_POINT ( 'NONE',  ( 81.50569694085116623, 63.36683741554951865, 3.125353918848690515 ) ) ;
#633 = CARTESIAN_POINT ( 'NONE',  ( 84.79809517660038409, 3.058972130929652256, -0.4747855469284483210 ) ) ;
#634 = ORIENTED_EDGE ( 'NONE', *, *, #35348, .T. ) ;
#635 = EDGE_CURVE ( 'NONE', #4065, #23718, #31879, .T. ) ;
#636 = CARTESIAN_POINT ( 'NONE',  ( 0.5000100785294406824, -32.75099641114868376, 7.784838882742140420 ) ) ;
#637 = VERTEX_POINT ( 'NONE', #15225 ) ;
#638 = CARTESIAN_POINT ( 'NONE',  ( 14.78598032573992072, -5.967041118660810106, 2.514107848754160823 ) ) ;
#639 = CARTESIAN_POINT ( 'NONE',  ( 37.03752275446304054, -3.000583964048129104, 5.986999200343480432 ) ) ;
#640 = CYLINDRICAL_SURFACE ( 'NONE', #18375, 0.09010775117052950700 ) ;
#641 = ADVANCED_FACE ( 'NONE', ( #18306 ), #6386, .T. ) ;
#642 = AXIS2_PLACEMENT_3D ( 'NONE', #18718, #9661, #9043 ) ;
#643 = CARTESIAN_POINT ( 'NONE',  ( 32.78033889701190873, -0.9298251412089901802, -5.322562699007520770 ) ) ;
#644 = FACE_OUTER_BOUND ( 'NONE', #40034, .T. ) ;
#645 = CARTESIAN_POINT ( 'NONE',  ( -0.7996099067669091287, -29.56993018339339940, -8.199999999999999289 ) ) ;
#646 = CARTESIAN_POINT ( 'NONE',  ( -73.95647868120518353, -1.676906216185754417, 10.78713444449159553 ) ) ;
#647 = DIRECTION ( 'NONE',  ( -1.000000000000000000, 0.000000000000000000, 0.000000000000000000 ) ) ;
#648 = CARTESIAN_POINT ( 'NONE',  ( -1.263904303455110734, -31.23517888999192138, 7.784838882742139532 ) ) ;
#649 = CARTESIAN_POINT ( 'NONE',  ( 28.64411823881500041, -3.206366735157959003, 4.677005430563262678 ) ) ;
#650 = VERTEX_POINT ( 'NONE', #31702 ) ;
#651 = VERTEX_POINT ( 'NONE', #34201 ) ;
#652 = CARTESIAN_POINT ( 'NONE',  ( 29.48743188508317914, 1.218356524489477177, 4.224828210317064681 ) ) ;
#653 = CARTESIAN_POINT ( 'NONE',  ( -8.448748702180639114, -26.64985754041175525, 6.700000000000000178 ) ) ;
#654 = CARTESIAN_POINT ( 'NONE',  ( 66.42693215277256513, 57.77698748017479602, -4.000000000000012434 ) ) ;
#655 = AXIS2_PLACEMENT_3D ( 'NONE', #39482, #36815, #24042 ) ;
#656 = EDGE_LOOP ( 'NONE', ( #16676, #14194, #23824, #26128 ) ) ;
#657 = CARTESIAN_POINT ( 'NONE',  ( 3.012471863950764828, -26.32525666483178384, 7.753200566781599079 ) ) ;
#658 = CARTESIAN_POINT ( 'NONE',  ( 2.277726599503935745, -26.11787535206076427, 7.665454363767879364 ) ) ;
#659 = ORIENTED_EDGE ( 'NONE', *, *, #28607, .F. ) ;
#660 = LINE ( 'NONE', #26374, #16175 ) ;
#661 = CARTESIAN_POINT ( 'NONE',  ( -4.978675913592189417, -26.64985754041175525, 6.800000000000000711 ) ) ;
#662 = ORIENTED_EDGE ( 'NONE', *, *, #39276, .T. ) ;
#663 = CARTESIAN_POINT ( 'NONE',  ( 81.85052347209619938, 65.46610162458726734, -1.468380750528963663 ) ) ;
#664 = VECTOR ( 'NONE', #23686, 999.9999999999998863 ) ;
#665 = LINE ( 'NONE', #13201, #39699 ) ;
#666 = ORIENTED_EDGE ( 'NONE', *, *, #24110, .T. ) ;
#667 = CARTESIAN_POINT ( 'NONE',  ( 76.46948511138614890, 60.90388096812819896, -3.723120700756775481 ) ) ;
#669 = CARTESIAN_POINT ( 'NONE',  ( 4.435798653882254250, -27.39796262386320080, 7.776484688137385248 ) ) ;
#668 = CARTESIAN_POINT ( 'NONE',  ( 9.703489126596464232, 56.50623631086179444, -4.000000000000000000 ) ) ;
#670 = CARTESIAN_POINT ( 'NONE',  ( 17.70185162816926194, 8.503195812862719194, -2.969200086112000037 ) ) ;
#671 = CARTESIAN_POINT ( 'NONE',  ( 76.39232039721480305, 61.07121484735989014, 3.784676997173924917 ) ) ;
#672 = ORIENTED_EDGE ( 'NONE', *, *, #6663, .F. ) ;
#673 = CARTESIAN_POINT ( 'NONE',  ( 4.431287826448039979, -27.54454009300915018, 6.920489980334473934 ) ) ;
#674 = CARTESIAN_POINT ( 'NONE',  ( 1.751749777469023384, -26.08494242606548141, 7.785344483711591934 ) ) ;
#675 = CARTESIAN_POINT ( 'NONE',  ( 24.20710697820493706, 2.664667655643908617, -3.984502513680244107 ) ) ;
#676 = CARTESIAN_POINT ( 'NONE',  ( 81.92450911876647979, 64.33049094056644890, 2.665107514500538066 ) ) ;
#678 = CARTESIAN_POINT ( 'NONE',  ( 15.85384028848737792, 7.981620951995479274, 3.484773800359201701 ) ) ;
#677 = CARTESIAN_POINT ( 'NONE',  ( -0.9615818451583477700, -31.84235468436096639, 7.660770905198781122 ) ) ;
#679 = CARTESIAN_POINT ( 'NONE',  ( 29.75545004716739683, -3.157578436209982353, 4.923334784591472335 ) ) ;
#680 = CARTESIAN_POINT ( 'NONE',  ( 2.278142440318064565, -26.21937241936939245, 7.756377446753164762 ) ) ;
#681 = CARTESIAN_POINT ( 'NONE',  ( -1.149815663681586608, -27.52689394563671854, 7.501983001166817822 ) ) ;
#682 = ADVANCED_FACE ( 'NONE', ( #22247 ), #28186, .F. ) ;
#683 = AXIS2_PLACEMENT_3D ( 'NONE', #24668, #40497, #3294 ) ;
#684 = ADVANCED_FACE ( 'NONE', ( #21823 ), #31095, .T. ) ;
#685 = CARTESIAN_POINT ( 'NONE',  ( 0.5325725529551263993, -26.27050565893173228, 6.894806418505347700 ) ) ;
#686 = CARTESIAN_POINT ( 'NONE',  ( -0.5871382310426926932, -32.08534543543891004, 6.865312560952603782 ) ) ;
#687 = CARTESIAN_POINT ( 'NONE',  ( 5.121324086407808451, -26.64985754041175525, 6.800000000000000711 ) ) ;
#688 = ADVANCED_FACE ( 'NONE', ( #37252 ), #40049, .T. ) ;
#689 = CARTESIAN_POINT ( 'NONE',  ( 35.33682791254538103, -3.445753084594619153, -5.710983022405980769 ) ) ;
#690 = DIRECTION ( 'NONE',  ( -0.8660254037844344888, -0.5000000000000069944, -0.000000000000000000 ) ) ;
#691 = CARTESIAN_POINT ( 'NONE',  ( 4.360293939584222400, -27.29508367342402408, 7.720710062488894465 ) ) ;
#692 = DIRECTION ( 'NONE',  ( -0.9267318687906771491, 0.3757233601570964532, -0.000000000000000000 ) ) ;
#693 = CARTESIAN_POINT ( 'NONE',  ( 2.086269118658516497, -32.94796176668813104, 6.929923840112066635 ) ) ;
#694 = B_SPLINE_CURVE_WITH_KNOTS ( 'NONE', 3,
 ( #33425, #8670, #33002, #32808, #27015, #17125, #17517, #39773, #29697, #14043 ),
 .UNSPECIFIED., .F., .F.,
 ( 4, 3, 3, 4 ),
 ( 0.0001477827378591783816, 0.0001512763324577387676, 0.0001815301820994196414, 0.0002056071264154448830 ),
 .UNSPECIFIED. ) ;
#695 = DIRECTION ( 'NONE',  ( -0.9848077530122067991, -0.1736481776669374644, -0.000000000000000000 ) ) ;
#696 = CARTESIAN_POINT ( 'NONE',  ( 21.86866938121569603, -13.71747586059087709, 2.499999999999999112 ) ) ;
#697 = AXIS2_PLACEMENT_3D ( 'NONE', #25369, #6431, #21672 ) ;
#698 = CARTESIAN_POINT ( 'NONE',  ( 31.82733904959990312, -2.965273931086898962, 5.173824024430509816 ) ) ;
#699 = VERTEX_POINT ( 'NONE', #31500 ) ;
#700 = DIRECTION ( 'NONE',  ( 1.000000000000000000, 8.966158204770716457E-16, 0.000000000000000000 ) ) ;
#701 = CARTESIAN_POINT ( 'NONE',  ( 68.67947939959147163, 58.42312895491860303, -3.988324671431326962 ) ) ;
#702 = ORIENTED_EDGE ( 'NONE', *, *, #27883, .T. ) ;
#703 = CARTESIAN_POINT ( 'NONE',  ( -0.9362520439413681839, -27.29047943236446372, 7.785344483711591934 ) ) ;
#704 = DIRECTION ( 'NONE',  ( -0.6427876096865430267, 0.7660444431189749048, -0.000000000000000000 ) ) ;
#705 = CARTESIAN_POINT ( 'NONE',  ( 23.67813930011643464, 3.094851216756080436, 3.803410633069329361 ) ) ;
#706 = CARTESIAN_POINT ( 'NONE',  ( 2.921324086407800280, -26.64985754041175525, 6.700000000000000178 ) ) ;
#707 = LINE ( 'NONE', #9951, #21414 ) ;
#708 = CARTESIAN_POINT ( 'NONE',  ( -1.771784689607549979, -30.01038707958819174, 7.013842709614101167 ) ) ;
#709 = ORIENTED_EDGE ( 'NONE', *, *, #911, .F. ) ;
#710 = CARTESIAN_POINT ( 'NONE',  ( -24.87867591359218977, -26.64985754041175525, 6.700000000000000178 ) ) ;
#711 = CARTESIAN_POINT ( 'NONE',  ( 81.26572199898306792, 62.02204868734986576, 2.661900242191197474 ) ) ;
#712 = CARTESIAN_POINT ( 'NONE',  ( 0.4869470754961160996, -26.28701135364670805, 7.750000000000001776 ) ) ;
#713 = VERTEX_POINT ( 'NONE', #13 ) ;
#714 = CARTESIAN_POINT ( 'NONE',  ( 79.75127500915171197, 61.39906162938307688, -2.976941560848460178 ) ) ;
#716 = CARTESIAN_POINT ( 'NONE',  ( -1.708141087249497758, -28.77499324473749809, 6.936703618422972006 ) ) ;
#715 = CARTESIAN_POINT ( 'NONE',  ( 22.31539195409567355, 0.2712039597043285344, 7.065721357752317466 ) ) ;
#717 = CARTESIAN_POINT ( 'NONE',  ( 81.65590348737067927, 63.08388229442042672, -2.971291902545804664 ) ) ;
#718 = CARTESIAN_POINT ( 'NONE',  ( 80.00843888008158444, 62.42993222482912330, 3.516968106976306796 ) ) ;
#719 = AXIS2_PLACEMENT_3D ( 'NONE', #16756, #1542, #11181 ) ;
#720 = CARTESIAN_POINT ( 'NONE',  ( 79.34209122208885390, 66.30884595491197331, 1.045691535380374182 ) ) ;
#721 = DIRECTION ( 'NONE',  ( -1.000000000000000000, 0.000000000000000000, 0.000000000000000000 ) ) ;
#722 = CARTESIAN_POINT ( 'NONE',  ( 25.51676067120702740, -4.685157242005201006, -0.9133679171623337867 ) ) ;
#723 = CARTESIAN_POINT ( 'NONE',  ( 1.700390093233090871, -29.56993018339339940, 7.750000000000000888 ) ) ;
#724 = ORIENTED_EDGE ( 'NONE', *, *, #737, .F. ) ;
#725 = CARTESIAN_POINT ( 'NONE',  ( -74.08736391206848282, -1.888185831823766314, 10.75649061611074764 ) ) ;
#726 = CARTESIAN_POINT ( 'NONE',  ( 4.668540769505296950, -31.42424039273510061, 7.754798119455333705 ) ) ;
#727 = B_SPLINE_CURVE_WITH_KNOTS ( 'NONE', 3,
 ( #13029, #25593, #38137, #22519, #282, #22110, #34687, #2990, #28884, #693, #38330, #6050, #15509, #6252, #28066, #12421, #18799, #3197, #6462, #19014, #31575, #38534, #7052, #26000, #32193, #10340, #29287, #13636, #29493, #1696, #16912 ),
 .UNSPECIFIED., .F., .F.,
 ( 4, 3, 3, 3, 3, 3, 3, 3, 3, 3, 4 ),
 ( 0.000000000000000000, 2.999644130997628625E-05, 6.002588995694725670E-05, 8.960886084587959242E-05, 0.0001190604700446492963, 0.0001489538463052720186, 0.0001796139255493969062, 0.0002109707048517083796, 0.0002426195318110367931, 0.0002740640997890067261, 0.0002849778069099888106 ),
 .UNSPECIFIED. ) ;
#728 = LINE ( 'NONE', #13680, #33363 ) ;
#729 = CARTESIAN_POINT ( 'NONE',  ( -73.45070404594234503, 38.65432087843067421, 8.800414904976364028 ) ) ;
#730 = EDGE_CURVE ( 'NONE', #28082, #6110, #14379, .T. ) ;
#731 = CARTESIAN_POINT ( 'NONE',  ( 32.01241132122780897, -3.694368527175160288, -4.883964182103501805 ) ) ;
#732 = CARTESIAN_POINT ( 'NONE',  ( 35.73033373643165334, -1.304506732970901028, -5.538159404137515729 ) ) ;
#733 = CARTESIAN_POINT ( 'NONE',  ( 3.376940742481379321, -32.64225469758540044, 6.865554069792297653 ) ) ;
#734 = CARTESIAN_POINT ( 'NONE',  ( 19.77034930170943738, 6.504725764514479813, 3.292039174873226060 ) ) ;
#735 = DIRECTION ( 'NONE',  ( 0.1736481776669273613, 0.9848077530122086864, -0.000000000000000000 ) ) ;
#736 = CARTESIAN_POINT ( 'NONE',  ( -57.33218521099392717, 34.44152469268617978, 4.000000000000000000 ) ) ;
#737 = EDGE_CURVE ( 'NONE', #21561, #15320, #31300, .T. ) ;
#738 = CARTESIAN_POINT ( 'NONE',  ( -59.89982099243562885, 24.84364830758654463, -9.562162450795215207 ) ) ;
#739 = VECTOR ( 'NONE', #13481, 1000.000000000000000 ) ;
#740 = DIRECTION ( 'NONE',  ( 1.000000000000000000, 0.000000000000000000, -0.000000000000000000 ) ) ;
#741 = CARTESIAN_POINT ( 'NONE',  ( 21.92110598244980935, 0.6179470853736169778, -7.522509096894697045 ) ) ;
#742 = CARTESIAN_POINT ( 'NONE',  ( 33.54628729347086846, -0.3308921759967717868, -5.040328079186997101 ) ) ;
#743 = CARTESIAN_POINT ( 'NONE',  ( -80.92837670882107659, 2.429809908903242555, 15.50000000000000000 ) ) ;
#744 = VERTEX_POINT ( 'NONE', #2705 ) ;
#745 = AXIS2_PLACEMENT_3D ( 'NONE', #8431, #24083, #11717 ) ;
#746 = ORIENTED_EDGE ( 'NONE', *, *, #18980, .F. ) ;
#747 = CARTESIAN_POINT ( 'NONE',  ( 66.69989039061726999, 57.93340768760646142, 3.999416444362183576 ) ) ;
#748 = CARTESIAN_POINT ( 'NONE',  ( -63.08758708074093136, 38.76906266698302517, 3.999999999999999112 ) ) ;
#749 = CARTESIAN_POINT ( 'NONE',  ( 85.85763368383675243, 1.114829962406831410, -5.799110970849834068 ) ) ;
#750 = TOROIDAL_SURFACE ( 'NONE', #1396, 82.54614097552274643, 3.000000000000000000 ) ;
#751 = CARTESIAN_POINT ( 'NONE',  ( 2.117690421663379841, -33.04496407602081121, 6.961115707816238007 ) ) ;
#752 = ORIENTED_EDGE ( 'NONE', *, *, #26701, .T. ) ;
#753 = CARTESIAN_POINT ( 'NONE',  ( -72.84815947045235873, 2.644610850572383320, -10.96147798754375202 ) ) ;
#754 = EDGE_CURVE ( 'NONE', #9594, #8017, #12125, .T. ) ;
#755 = DIRECTION ( 'NONE',  ( 0.000000000000000000, 0.000000000000000000, 1.000000000000000000 ) ) ;
#756 = CYLINDRICAL_SURFACE ( 'NONE', #23191, 0.1000000000000028644 ) ;
#757 = DIRECTION ( 'NONE',  ( 0.8660254037844450359, -0.4999999999999888978, -0.000000000000000000 ) ) ;
#758 = ORIENTED_EDGE ( 'NONE', *, *, #22196, .T. ) ;
#759 = CARTESIAN_POINT ( 'NONE',  ( 6.921324086407803833, -24.55319635012989110, 6.800000000000000711 ) ) ;
#760 = ORIENTED_EDGE ( 'NONE', *, *, #18864, .T. ) ;
#761 = CARTESIAN_POINT ( 'NONE',  ( 80.85057025077259141, 61.36744894077061474, -2.123311106147459437 ) ) ;
#762 = CARTESIAN_POINT ( 'NONE',  ( -1.723126226492296853, -28.85479948634039360, 7.766640943994350010 ) ) ;
#763 = CARTESIAN_POINT ( 'NONE',  ( 80.09094484276241133, 63.40703332228300582, 3.714073935154433403 ) ) ;
#765 = ORIENTED_EDGE ( 'NONE', *, *, #16076, .T. ) ;
#764 = LINE ( 'NONE', #38611, #21033 ) ;
#766 = EDGE_CURVE ( 'NONE', #17308, #38743, #18493, .T. ) ;
#767 = CARTESIAN_POINT ( 'NONE',  ( 1.531218635892081847, -33.06583936671340496, 7.013842709614101167 ) ) ;
#768 = CARTESIAN_POINT ( 'NONE',  ( 0.9171018672454774867, -32.98115864172326184, 6.906857269533146493 ) ) ;
#769 = CARTESIAN_POINT ( 'NONE',  ( 3.015109609237833332, -26.32624206733842698, 7.750000000000000888 ) ) ;
#770 = CARTESIAN_POINT ( 'NONE',  ( 21.85643539959776760, -0.9922589305345951294, -16.01828770219436393 ) ) ;
#771 = CARTESIAN_POINT ( 'NONE',  ( 24.04398671587223291, 3.332573078807886446, -3.269442169970088408 ) ) ;
#772 = EDGE_LOOP ( 'NONE', ( #34997, #39847, #32312, #40232, #11861 ) ) ;
#773 = CARTESIAN_POINT ( 'NONE',  ( 5.200265217546576224, -29.54023460135108436, 7.660770905198780234 ) ) ;
#774 = VERTEX_POINT ( 'NONE', #22842 ) ;
#775 = CARTESIAN_POINT ( 'NONE',  ( -0.9509358128338576410, -31.69844278021870210, 6.874555630061443878 ) ) ;
#776 = LINE ( 'NONE', #7142, #14906 ) ;
#777 = AXIS2_PLACEMENT_3D ( 'NONE', #21400, #36426, #4928 ) ;
#778 = CARTESIAN_POINT ( 'NONE',  ( -74.68647436060540201, -2.705062680926989316, -10.58800659810225220 ) ) ;
#779 = ADVANCED_FACE ( 'NONE', ( #28815 ), #25521, .F. ) ;
#780 = DIRECTION ( 'NONE',  ( -0.000000000000000000, -0.000000000000000000, -1.000000000000000000 ) ) ;
#781 = DIRECTION ( 'NONE',  ( 0.4999999999999979461, 0.8660254037844397068, -0.000000000000000000 ) ) ;
#782 = CARTESIAN_POINT ( 'NONE',  ( 80.84834833306135238, 63.77578157039150142, 3.533418250979425856 ) ) ;
#783 = CARTESIAN_POINT ( 'NONE',  ( 84.50243033367722489, 2.523019330700893903, 3.504063919878146027 ) ) ;
#784 = DIRECTION ( 'NONE',  ( 0.000000000000000000, -1.000000000000000000, 0.000000000000000000 ) ) ;
#785 = CARTESIAN_POINT ( 'NONE',  ( -1.272073826050460932, -27.72701560212543725, 7.766640943994650215 ) ) ;
#786 = CARTESIAN_POINT ( 'NONE',  ( -64.08758708074093136, 38.76906266698303227, 3.000000000000000000 ) ) ;
#787 = CARTESIAN_POINT ( 'NONE',  ( 32.07395207475902055, -0.6787058776523876569, 5.212313951365143083 ) ) ;
#788 = CARTESIAN_POINT ( 'NONE',  ( -64.95171866297675933, 36.28765213650434163, 6.629387290673633970 ) ) ;
#789 = CARTESIAN_POINT ( 'NONE',  ( -0.3256050783848223329, -26.83948268077026711, 6.988553391373221402 ) ) ;
#790 = CARTESIAN_POINT ( 'NONE',  ( 35.94200923520244828, 151.3264224549853907, -1.000000000000000000 ) ) ;
#791 = CARTESIAN_POINT ( 'NONE',  ( 0.6185823884176052667, -26.24155567332487493, 7.754798119455333705 ) ) ;
#792 = CARTESIAN_POINT ( 'NONE',  ( 25.29738944813237467, 1.738831336413337203, 4.154667461693681396 ) ) ;
#793 = EDGE_CURVE ( 'NONE', #37191, #15824, #9816, .T. ) ;
#794 = LINE ( 'NONE', #22821, #9570 ) ;
#795 = CARTESIAN_POINT ( 'NONE',  ( 87.05466826895010968, 0.5737893332097195875, -5.097061431219924721 ) ) ;
#796 = ORIENTED_EDGE ( 'NONE', *, *, #39201, .T. ) ;
#798 = CARTESIAN_POINT ( 'NONE',  ( 4.821723147117300989, -30.91800106084867394, 6.997764925645181044 ) ) ;
#797 = CARTESIAN_POINT ( 'NONE',  ( 81.21900516562017458, 61.35514353465740101, -1.483717294826000455 ) ) ;
#799 = B_SPLINE_CURVE_WITH_KNOTS ( 'NONE', 3,
 ( #35004, #6778, #10055, #6976, #15414, #27973, #40522, #31289, #24905, #37438 ),
 .UNSPECIFIED., .F., .F.,
 ( 4, 3, 3, 4 ),
 ( 8.940560153363745023E-19, 3.025570593003111997E-05, 6.051145698344058784E-05, 6.468151674593778733E-05 ),
 .UNSPECIFIED. ) ;
#800 = DIRECTION ( 'NONE',  ( -0.9506097019758704691, 0.3103887796125160414, 0.000000000000000000 ) ) ;
#801 = ORIENTED_EDGE ( 'NONE', *, *, #26499, .T. ) ;
#802 = CARTESIAN_POINT ( 'NONE',  ( 0.000000000000000000, 10.37661300689600097, 6.000000000000000000 ) ) ;
#803 = ORIENTED_EDGE ( 'NONE', *, *, #28324, .T. ) ;
#804 = CARTESIAN_POINT ( 'NONE',  ( -73.13398320254746920, 7.456860240122096251, 9.756630903624417428 ) ) ;
#805 = AXIS2_PLACEMENT_3D ( 'NONE', #17898, #40334, #36246 ) ;
#807 = ORIENTED_EDGE ( 'NONE', *, *, #15906, .F. ) ;
#806 = ORIENTED_EDGE ( 'NONE', *, *, #32982, .T. ) ;
#808 = CARTESIAN_POINT ( 'NONE',  ( 81.01565502672981722, 61.93906859853276359, -2.769656700700041885 ) ) ;
#809 = ADVANCED_FACE ( 'NONE', ( #1232 ), #9869, .F. ) ;
#810 = LINE ( 'NONE', #13343, #16776 ) ;
#811 = EDGE_CURVE ( 'NONE', #38080, #11405, #6983, .T. ) ;
#812 = CARTESIAN_POINT ( 'NONE',  ( 22.74182454973798073, 2.295841465708973850, 4.886361631232980507 ) ) ;
#815 = ORIENTED_EDGE ( 'NONE', *, *, #10557, .T. ) ;
#814 = ORIENTED_EDGE ( 'NONE', *, *, #31306, .F. ) ;
#813 = AXIS2_PLACEMENT_3D ( 'NONE', #2939, #28428, #28639 ) ;
#816 = EDGE_CURVE ( 'NONE', #10909, #29634, #27831, .T. ) ;
#817 = CARTESIAN_POINT ( 'NONE',  ( 5.751251297819365504, -25.49307895267003587, 6.700000000000000178 ) ) ;
#818 = CARTESIAN_POINT ( 'NONE',  ( 0.03162470699431383508, -32.53223031769636009, 7.703977250142849620 ) ) ;
#820 = CARTESIAN_POINT ( 'NONE',  ( 3.962066057316325551, -32.24103972498801340, 7.638132480492515697 ) ) ;
#819 = CARTESIAN_POINT ( 'NONE',  ( 4.580489648044480333, -31.37689880320810332, 6.863904403958575706 ) ) ;
#821 = CYLINDRICAL_SURFACE ( 'NONE', #26427, 0.1000000000000028644 ) ;
#822 = CARTESIAN_POINT ( 'NONE',  ( -64.08758708074093136, 43.19303868977686989, -2.106422863670424306 ) ) ;
#823 = CARTESIAN_POINT ( 'NONE',  ( 70.70040249450607917, 60.07892802134021792, 3.908768822720051883 ) ) ;
#824 = CARTESIAN_POINT ( 'NONE',  ( 22.00320784554085662, 4.481518016395985349, -3.871533879853490845 ) ) ;
#825 = ORIENTED_EDGE ( 'NONE', *, *, #17697, .T. ) ;
#826 = VERTEX_POINT ( 'NONE', #19549 ) ;
#827 = CARTESIAN_POINT ( 'NONE',  ( 21.85643539959772497, -13.01485165473748573, 3.478087416278500932 ) ) ;
#828 = CARTESIAN_POINT ( 'NONE',  ( 21.86697325015170890, 4.291357277895272659, 2.119771864001716910 ) ) ;
#829 = ORIENTED_EDGE ( 'NONE', *, *, #15859, .F. ) ;
#830 = CARTESIAN_POINT ( 'NONE',  ( 0.4404571835168948346, -32.72788522653752352, 6.864651958020304257 ) ) ;
#831 = CARTESIAN_POINT ( 'NONE',  ( 79.91673984738221748, 65.77987873796179485, 2.647945256410967563 ) ) ;
#832 = CARTESIAN_POINT ( 'NONE',  ( 87.01296019436635731, 0.4868102506410553754, -5.723292304581113044 ) ) ;
#833 = VERTEX_POINT ( 'NONE', #26333 ) ;
#834 = CARTESIAN_POINT ( 'NONE',  ( 0.5495968526122669839, -32.76925980410539552, 7.756377446753163873 ) ) ;
#835 = EDGE_LOOP ( 'NONE', ( #34028, #35440, #19587, #33373, #11686 ) ) ;
#836 = CARTESIAN_POINT ( 'NONE',  ( 14.77222812468937363, 12.33286846116137347, 2.511961485181785747 ) ) ;
#837 = CARTESIAN_POINT ( 'NONE',  ( 35.94401475533869927, -2.118279520774572600, 5.816330830489228276 ) ) ;
#838 = CARTESIAN_POINT ( 'NONE',  ( 5.072211240599806104, -29.13298902044168415, 6.871394612369934762 ) ) ;
#839 = CARTESIAN_POINT ( 'NONE',  ( 36.64572461763481215, -2.462317435528831755, -5.925849625417530575 ) ) ;
#840 = CYLINDRICAL_SURFACE ( 'NONE', #9559, 0.1000000000000028644 ) ;
#841 = CARTESIAN_POINT ( 'NONE',  ( 84.16515158064987645, 2.938904301663770369, -1.440371321264852122 ) ) ;
#842 = CARTESIAN_POINT ( 'NONE',  ( 4.402564028851855937, -31.79440116261879368, 7.720710062488891801 ) ) ;
#843 = ORIENTED_EDGE ( 'NONE', *, *, #8264, .F. ) ;
#844 = CARTESIAN_POINT ( 'NONE',  ( 5.751251297819365504, -26.64985754041175525, 6.700000000000000178 ) ) ;
#845 = AXIS2_PLACEMENT_3D ( 'NONE', #34297, #6066, #28080 ) ;
#846 = LINE ( 'NONE', #13981, #2059 ) ;
#847 = CARTESIAN_POINT ( 'NONE',  ( 28.41948456483106256, -4.023518219021338993, 4.166478601093604794 ) ) ;
#848 = EDGE_LOOP ( 'NONE', ( #12316, #20240, #26085, #37691 ) ) ;
#849 = ORIENTED_EDGE ( 'NONE', *, *, #22675, .F. ) ;
#850 = CARTESIAN_POINT ( 'NONE',  ( 21.73904118813925379, 4.235523336977800035, 2.801162882007421029 ) ) ;
#851 =( BOUNDED_CURVE ( )  B_SPLINE_CURVE ( 3, ( #21836, #427, #38077, #9879 ),
 .UNSPECIFIED., .F., .F. ) 
 B_SPLINE_CURVE_WITH_KNOTS ( ( 4, 4 ),
 ( 0.3200567789910438443, 0.9848974682458135899 ),
 .UNSPECIFIED. ) 
 CURVE ( )  GEOMETRIC_REPRESENTATION_ITEM ( )  RATIONAL_B_SPLINE_CURVE ( ( 0.9715283101266052324, 0.9610937201533095164, 0.9699355995880819536, 0.9980539484309227660 ) ) 
 REPRESENTATION_ITEM ( '' )  );
#852 = DIRECTION ( 'NONE',  ( 1.000000000000000000, 0.000000000000000000, 0.000000000000000000 ) ) ;
#853 = CARTESIAN_POINT ( 'NONE',  ( -70.92837670882107659, -27.85319909218681644, 0.000000000000000000 ) ) ;
#854 = EDGE_CURVE ( 'NONE', #36422, #301, #38867, .T. ) ;
#855 = CARTESIAN_POINT ( 'NONE',  ( 86.80810971983586910, -1.084991844513179204, 5.287006610588839806 ) ) ;
#856 = ORIENTED_EDGE ( 'NONE', *, *, #2258, .T. ) ;
#857 = ADVANCED_FACE ( 'NONE', ( #8582 ), #23435, .F. ) ;
#858 = CARTESIAN_POINT ( 'NONE',  ( -12.99139449055068596, 10.37661300689600097, -6.000000000000000000 ) ) ;
#859 = DIRECTION ( 'NONE',  ( 0.000000000000000000, 0.000000000000000000, -1.000000000000000000 ) ) ;
#860 = ORIENTED_EDGE ( 'NONE', *, *, #25488, .F. ) ;
#861 = FACE_BOUND ( 'NONE', #37475, .T. ) ;
#862 = CARTESIAN_POINT ( 'NONE',  ( 3.884973724021333119, -32.30444921973087702, 6.865554069792297653 ) ) ;
#863 = VERTEX_POINT ( 'NONE', #8375 ) ;
#864 = CARTESIAN_POINT ( 'NONE',  ( 21.74862740251015580, 5.983917815004713425, 3.320825558061557103 ) ) ;
#865 = EDGE_CURVE ( 'NONE', #14656, #4406, #26525, .T. ) ;
#866 = CARTESIAN_POINT ( 'NONE',  ( 80.96936403957134587, 66.06451342975866226, -1.623788564014418512 ) ) ;
#867 = CARTESIAN_POINT ( 'NONE',  ( 4.459949229015542471, -27.41706340682027232, 7.751599049952173637 ) ) ;
#868 = ORIENTED_EDGE ( 'NONE', *, *, #20775, .T. ) ;
#869 = CARTESIAN_POINT ( 'NONE',  ( 75.23821009641447688, 63.49083772021889160, -3.097219288950977312 ) ) ;
#871 = CARTESIAN_POINT ( 'NONE',  ( 4.398191130436243768, -27.36279617112402462, 7.785096263473211486 ) ) ;
#870 = FACE_OUTER_BOUND ( 'NONE', #24325, .T. ) ;
#872 = DIRECTION ( 'NONE',  ( 0.000000000000000000, 0.7126435865141270698, -0.7015262779114420644 ) ) ;
#873 = CARTESIAN_POINT ( 'NONE',  ( 76.98341904138483471, 61.29654188154451333, 3.753756190332411258 ) ) ;
#874 = PRESENTATION_LAYER_ASSIGNMENT (  '', '', ( #2880 ) ) ;
#875 = CARTESIAN_POINT ( 'NONE',  ( -81.07947155388369254, 30.81399289130168384, -9.800414904976365804 ) ) ;
#876 = LINE ( 'NONE', #31758, #28712 ) ;
#877 = EDGE_CURVE ( 'NONE', #28154, #25277, #11252, .T. ) ;
#878 = CARTESIAN_POINT ( 'NONE',  ( 22.90829551299158240, 3.597247491013313425, -3.781791572659710443 ) ) ;
#879 = CARTESIAN_POINT ( 'NONE',  ( 82.22785179944530398, 62.76084426383168591, 1.971256063808052739 ) ) ;
#880 = CARTESIAN_POINT ( 'NONE',  ( -0.1940712780794633940, -32.51289061680132875, 7.013842709614101167 ) ) ;
#881 = B_SPLINE_CURVE_WITH_KNOTS ( 'NONE', 3,
 ( #6575, #34996, #12940, #40517, #31896, #12730, #25309, #34187, #9231, #37841, #3102, #21809, #9644, #28803, #22229, #38052, #9852, #28594, #34389, #6773, #37631, #3308, #5092, #604, #13146 ),
 .UNSPECIFIED., .F., .F.,
 ( 4, 3, 3, 3, 3, 3, 3, 3, 4 ),
 ( 6.468151674593807193E-05, 9.076621574721745937E-05, 0.0001210204262067965164, 0.0001512763324577425352, 0.0001815301820994146811, 0.0002117781465860671007, 0.0002420274594459666966, 0.0002722905548971137285, 0.0002816827545175591132 ),
 .UNSPECIFIED. ) ;
#882 = CARTESIAN_POINT ( 'NONE',  ( 28.73718198699435433, 0.3327373454474676917, -5.564570571917969666 ) ) ;
#883 = CARTESIAN_POINT ( 'NONE',  ( 2.396593935003837661, -26.24196453429818732, 7.768425012602593327 ) ) ;
#884 = FACE_OUTER_BOUND ( 'NONE', #21957, .T. ) ;
#885 = DIRECTION ( 'NONE',  ( -1.000000000000000000, 0.000000000000000000, 0.000000000000000000 ) ) ;
#886 = CARTESIAN_POINT ( 'NONE',  ( -0.5483518474143298516, -32.12005952999000868, 6.870716933885664623 ) ) ;
#887 = CARTESIAN_POINT ( 'NONE',  ( 37.06596529586517619, -2.656456832825214498, -5.990207561623762444 ) ) ;
#888 = CARTESIAN_POINT ( 'NONE',  ( 1.122637746148142490, -32.92048794741741347, 7.756377446753163873 ) ) ;
#889 = PLANE ( 'NONE',  #1673 ) ;
#890 = CARTESIAN_POINT ( 'NONE',  ( 4.938390203311415748E-15, -42.37473357531882101, 6.000000000000000000 ) ) ;
#891 = CARTESIAN_POINT ( 'NONE',  ( 22.05611991773309555, -11.37525250134437016, -2.500000000000000000 ) ) ;
#892 = CARTESIAN_POINT ( 'NONE',  ( -1.466146261265031558, -28.33173257664969213, 7.782034975670477195 ) ) ;
#893 = FACE_OUTER_BOUND ( 'NONE', #28439, .T. ) ;
#894 = ORIENTED_EDGE ( 'NONE', *, *, #2902, .T. ) ;
#895 = CARTESIAN_POINT ( 'NONE',  ( 33.45000747465049074, -3.250805911200664866, 5.427080676543816651 ) ) ;
#896 = DIRECTION ( 'NONE',  ( -0.000000000000000000, -0.000000000000000000, -1.000000000000000000 ) ) ;
#897 = CARTESIAN_POINT ( 'NONE',  ( 68.47014483779531702, 58.97518246833449496, -3.964410623303926684 ) ) ;
#898 = COLOUR_RGB ( '',0.7921568627450980005, 0.8196078431372548767, 0.9333333333333333481 ) ;
#899 = CARTESIAN_POINT ( 'NONE',  ( -54.01549048184568846, -38.28842912540938670, 4.800000000000000711 ) ) ;
#900 = ORIENTED_EDGE ( 'NONE', *, *, #14039, .T. ) ;
#901 = CYLINDRICAL_SURFACE ( 'NONE', #8152, 0.1000000000000028644 ) ;
#902 = LINE ( 'NONE', #25603, #35773 ) ;
#903 = CARTESIAN_POINT ( 'NONE',  ( 23.43999384881404069, 3.253530542321768859, 3.760554638137439287 ) ) ;
#904 = CARTESIAN_POINT ( 'NONE',  ( 5.049772904672250817, -28.55423167660719841, 6.971170733404099984 ) ) ;
#905 = CARTESIAN_POINT ( 'NONE',  ( 1.120974760640235823, -26.21965457890690132, 7.775108481317163367 ) ) ;
#907 = EDGE_CURVE ( 'NONE', #5789, #22409, #33321, .T. ) ;
#906 = CARTESIAN_POINT ( 'NONE',  ( 1.226940962756493336, -26.10208781839716252, 6.870724624169668004 ) ) ;
#908 = VERTEX_POINT ( 'NONE', #17636 ) ;
#909 = CARTESIAN_POINT ( 'NONE',  ( 22.18569188669614434, 5.274102994114218568, 3.071853425151234607 ) ) ;
#910 = EDGE_CURVE ( 'NONE', #15868, #38802, #3918, .T. ) ;
#911 = EDGE_CURVE ( 'NONE', #4342, #17714, #30011, .T. ) ;
#912 = SURFACE_STYLE_USAGE ( .BOTH. , #38954 ) ;
#914 = VECTOR ( 'NONE', #6048, 1000.000000000000000 ) ;
#913 = CARTESIAN_POINT ( 'NONE',  ( 78.66037426029973290, 66.03727662354840788, 1.183438861787456942 ) ) ;
#915 = AXIS2_PLACEMENT_3D ( 'NONE', #29380, #4276, #4480 ) ;
#916 = EDGE_CURVE ( 'NONE', #8305, #24066, #39886, .T. ) ;
#917 = ORIENTED_EDGE ( 'NONE', *, *, #25735, .T. ) ;
#918 = CARTESIAN_POINT ( 'NONE',  ( 77.99157368707381011, 64.87245838797727515, -2.976941560848442414 ) ) ;
#920 = CARTESIAN_POINT ( 'NONE',  ( 14.77222415230653318, -4.492512959436772313, -2.511960865195376424 ) ) ;
#919 = CARTESIAN_POINT ( 'NONE',  ( 27.39979242429538786, 1.046165008357551329, 4.482586396029306641 ) ) ;
#921 = CARTESIAN_POINT ( 'NONE',  ( 79.28168835806300763, 66.11151980551120744, -1.907437723456246736 ) ) ;
#922 = CARTESIAN_POINT ( 'NONE',  ( 78.69960226590261243, 64.59913094042720161, 3.401284978681007765 ) ) ;
#923 = FACE_BOUND ( 'NONE', #15811, .T. ) ;
#924 = ORIENTED_EDGE ( 'NONE', *, *, #32559, .T. ) ;
#925 = CARTESIAN_POINT ( 'NONE',  ( 82.41652906543031065, 64.58603266165646062, 1.328060019257126356 ) ) ;
#927 = ORIENTED_EDGE ( 'NONE', *, *, #964, .F. ) ;
#926 = CARTESIAN_POINT ( 'NONE',  ( -64.08758708074093136, 43.97762867865598935, 1.773567450131052770 ) ) ;
#928 = CARTESIAN_POINT ( 'NONE',  ( 23.99854160108877110, 3.116918725036224025, -4.608611027060286247 ) ) ;
#929 = CARTESIAN_POINT ( 'NONE',  ( -64.12639773666757037, 35.29406715002951245, -4.430479139283492351 ) ) ;
#930 = ORIENTED_EDGE ( 'NONE', *, *, #27699, .T. ) ;
#931 = CARTESIAN_POINT ( 'NONE',  ( -79.85848762145901958, -6.650571597313232886, 4.518583439907962074 ) ) ;
#932 = FACE_OUTER_BOUND ( 'NONE', #28199, .T. ) ;
#933 = CARTESIAN_POINT ( 'NONE',  ( -0.1271964900342822669, -32.54647689963780977, 7.776484688137386136 ) ) ;
#934 = DIRECTION ( 'NONE',  ( -0.000000000000000000, -0.000000000000000000, -1.000000000000000000 ) ) ;
#935 = EDGE_LOOP ( 'NONE', ( #34001, #29049, #22823, #20751 ) ) ;
#936 = CARTESIAN_POINT ( 'NONE',  ( 37.00823095920353722, -3.245628662103481776, -5.947143878220320978 ) ) ;
#937 = DIRECTION ( 'NONE',  ( 1.165409145176970240E-16, -1.000000000000000000, 0.000000000000000000 ) ) ;
#938 = CARTESIAN_POINT ( 'NONE',  ( -4.890026461918814071, -8.228598103685714525E-16, -6.000000000000000000 ) ) ;
#939 = CARTESIAN_POINT ( 'NONE',  ( 5.119051991949654656, -30.32009737959945284, 6.875780273367530171 ) ) ;
#940 = LINE ( 'NONE', #6709, #6812 ) ;
#941 = CARTESIAN_POINT ( 'NONE',  ( -4.878675913592187108, -26.64985754041175525, 6.700000000000000178 ) ) ;
#942 = DIRECTION ( 'NONE',  ( 1.000000000000000000, 0.000000000000000000, -0.000000000000000000 ) ) ;
#943 = CIRCLE ( 'NONE', #6193, 0.1000000000000028644 ) ;
#944 = LINE ( 'NONE', #37986, #7913 ) ;
#945 = AXIS2_PLACEMENT_3D ( 'NONE', #27776, #14403, #26973 ) ;
#946 = VECTOR ( 'NONE', #20283, 1000.000000000000000 ) ;
#947 = CARTESIAN_POINT ( 'NONE',  ( 24.52892761326155835, 0.9676208338128078346, -4.779935416704812035 ) ) ;
#948 = CARTESIAN_POINT ( 'NONE',  ( 36.44367235456785892, -1.740113775189354506, -5.733408591441955693 ) ) ;
#949 = LINE ( 'NONE', #28530, #9128 ) ;
#950 = ORIENTED_EDGE ( 'NONE', *, *, #18826, .T. ) ;
#951 = CARTESIAN_POINT ( 'NONE',  ( 66.74110339505794798, 57.81860698948682398, 3.998609561963397674 ) ) ;
#952 = VECTOR ( 'NONE', #26317, 999.9999999999998863 ) ;
#953 = CYLINDRICAL_SURFACE ( 'NONE', #22759, 0.09010775117052971517 ) ;
#954 = CARTESIAN_POINT ( 'NONE',  ( 84.14932678670007249, 2.958124188176427083, -1.306863746360770184 ) ) ;
#955 = CIRCLE ( 'NONE', #2272, 6.406751979251626317 ) ;
#956 = CARTESIAN_POINT ( 'NONE',  ( -34.34874870218063592, -26.64985754041175525, 6.700000000000000178 ) ) ;
#957 = ORIENTED_EDGE ( 'NONE', *, *, #23789, .T. ) ;
#958 = CARTESIAN_POINT ( 'NONE',  ( -75.45330471031414277, 33.71485196875532608, 15.50000000000000000 ) ) ;
#959 = SHAPE_DEFINITION_REPRESENTATION ( #39464, #28236 ) ;
#960 = CARTESIAN_POINT ( 'NONE',  ( -2.628911188892000261, -29.52345495559962885, 6.954324564059724878 ) ) ;
#961 = CARTESIAN_POINT ( 'NONE',  ( 1.086859017207900235, -26.12551858065138077, 7.762796336881262249 ) ) ;
#962 = ORIENTED_EDGE ( 'NONE', *, *, #2526, .F. ) ;
#963 = CARTESIAN_POINT ( 'NONE',  ( -1.748913751257205051, -28.97637829014552580, 7.636816916992232862 ) ) ;
#964 = EDGE_CURVE ( 'NONE', #14571, #23320, #17842, .T. ) ;
#965 = ORIENTED_EDGE ( 'NONE', *, *, #8161, .F. ) ;
#966 = CARTESIAN_POINT ( 'NONE',  ( 80.30026770407522463, 62.83227110018524542, -3.557377001560567020 ) ) ;
#967 = CARTESIAN_POINT ( 'NONE',  ( -26.34874870218063947, -25.49307895267003587, 6.700000000000000178 ) ) ;
#968 = CARTESIAN_POINT ( 'NONE',  ( 80.23164863169043315, 63.12273326640292481, 3.657510014241676988 ) ) ;
#970 = EDGE_LOOP ( 'NONE', ( #15579, #17607, #22271, #8008 ) ) ;
#969 = CARTESIAN_POINT ( 'NONE',  ( -1.268168650321787716, -31.22753658603060956, 6.894806418505346812 ) ) ;
#971 = AXIS2_PLACEMENT_3D ( 'NONE', #36507, #21274, #21481 ) ;
#972 = LINE ( 'NONE', #29558, #210 ) ;
#973 = CARTESIAN_POINT ( 'NONE',  ( 1.005809635450030548, -33.00033240446269645, 6.864368109219936009 ) ) ;
#974 = CARTESIAN_POINT ( 'NONE',  ( 3.235878913814441038, -32.60345520914638939, 7.013842709614101167 ) ) ;
#975 = CARTESIAN_POINT ( 'NONE',  ( 21.85643539959777826, -5.920441741711214512, 15.33489310402742234 ) ) ;
#976 = CARTESIAN_POINT ( 'NONE',  ( 3.501122161660540577, -26.68594518542784044, 7.759451378593094084 ) ) ;
#977 = CARTESIAN_POINT ( 'NONE',  ( 24.75846013112230537, 3.019289815473042093, -3.350249464038115743 ) ) ;
#978 = ORIENTED_EDGE ( 'NONE', *, *, #38162, .F. ) ;
#979 = CARTESIAN_POINT ( 'NONE',  ( 5.172564876073734830, -29.12947328719863194, 7.013842709614101167 ) ) ;
#980 = ORIENTED_EDGE ( 'NONE', *, *, #4879, .T. ) ;
#981 = VECTOR ( 'NONE', #27050, 1000.000000000000114 ) ;
#982 = CARTESIAN_POINT ( 'NONE',  ( -1.034439892636894731, -31.59000574243066950, 6.949473656533220023 ) ) ;
#983 = CARTESIAN_POINT ( 'NONE',  ( -0.5790606577958476997, -32.20657232056785091, 7.785344483711592822 ) ) ;
#984 = CARTESIAN_POINT ( 'NONE',  ( -72.89865255728501836, 3.415802629356370801, -10.95661767982553414 ) ) ;
#985 = DIRECTION ( 'NONE',  ( 1.000000000000000000, 6.938893903907229167E-15, 0.000000000000000000 ) ) ;
#986 = CARTESIAN_POINT ( 'NONE',  ( -26.34874870218063947, -26.64985754041175525, 6.700000000000000178 ) ) ;
#987 = CARTESIAN_POINT ( 'NONE',  ( 79.42405716688907091, 65.78352207363050752, 2.615128354545391165 ) ) ;
#988 = CARTESIAN_POINT ( 'NONE',  ( 86.62140889132389532, -0.8164050916001737157, 5.580443680875508683 ) ) ;
#989 = CARTESIAN_POINT ( 'NONE',  ( -0.5767923600352571345, -26.91202874155497682, 7.697032948437509958 ) ) ;
#990 = CARTESIAN_POINT ( 'NONE',  ( 2.931185808669443116, -32.84638282411072652, 7.697032948437507294 ) ) ;
#991 = CARTESIAN_POINT ( 'NONE',  ( -1.643416196941662077, -30.18553864676747622, 7.652160403243382980 ) ) ;
#992 = EDGE_CURVE ( 'NONE', #8047, #13934, #24934, .T. ) ;
#993 = CARTESIAN_POINT ( 'NONE',  ( -32.87867591359218977, -24.55319635012989110, 6.700000000000000178 ) ) ;
#994 = CARTESIAN_POINT ( 'NONE',  ( 16.66444302124740418, 9.373703860693387568, -2.807287383179874585 ) ) ;
#995 = CARTESIAN_POINT ( 'NONE',  ( 4.912218266805315814, -28.45446572434498478, 7.785868773668302545 ) ) ;
#996 = CARTESIAN_POINT ( 'NONE',  ( -70.92837670882107659, -23.80776546975053165, 0.000000000000000000 ) ) ;
#997 = ORIENTED_EDGE ( 'NONE', *, *, #14340, .F. ) ;
#998 = CARTESIAN_POINT ( 'NONE',  ( 69.03381461298826594, 59.23726071663833181, 3.954017255840780454 ) ) ;
#999 = CARTESIAN_POINT ( 'NONE',  ( 35.45370152372439065, -1.914224272725399745, 5.739805592425503811 ) ) ;
#1000 = ADVANCED_FACE ( 'NONE', ( #27123 ), #39673, .F. ) ;
#1001 = AXIS2_PLACEMENT_3D ( 'NONE', #28881, #26404, #13835 ) ;
#1002 = CARTESIAN_POINT ( 'NONE',  ( -64.08758708074094557, 43.19303869255161743, -2.106422866370387226 ) ) ;
#1003 = AXIS2_PLACEMENT_3D ( 'NONE', #22810, #7149, #38030 ) ;
#1004 = CARTESIAN_POINT ( 'NONE',  ( 88.13490256179494509, -0.6395810955261213016, -2.488665338685403849 ) ) ;
#1006 = CARTESIAN_POINT ( 'NONE',  ( 4.817698917275965442, -30.92727803983277113, 6.939395833800437785 ) ) ;
#1005 = CARTESIAN_POINT ( 'NONE',  ( 81.11292571623972947, 62.23233742369612997, -2.923497156821700305 ) ) ;
#1007 = VECTOR ( 'NONE', #40210, 1000.000000000000000 ) ;
#1008 = CARTESIAN_POINT ( 'NONE',  ( -1.276779499330499945, -27.72966765302937020, 6.863784140767622333 ) ) ;
#1009 = CARTESIAN_POINT ( 'NONE',  ( 88.14657295384911606, -0.6526898337915518766, -2.384354617864239856 ) ) ;
#1010 = VERTEX_POINT ( 'NONE', #1619 ) ;
#1011 = CARTESIAN_POINT ( 'NONE',  ( -60.36144324275490902, 24.84364830758653397, -8.926047827505314558 ) ) ;
#1012 = AXIS2_PLACEMENT_3D ( 'NONE', #16573, #16185, #22383 ) ;
#1013 = ORIENTED_EDGE ( 'NONE', *, *, #7946, .T. ) ;
#1014 = CARTESIAN_POINT ( 'NONE',  ( -72.53312289749355557, -1.419736944430859849, 9.872087320082300721 ) ) ;
#1015 = VERTEX_POINT ( 'NONE', #14154 ) ;
#1016 = EDGE_CURVE ( 'NONE', #7067, #19825, #28357, .T. ) ;
#1017 = CARTESIAN_POINT ( 'NONE',  ( 80.89004220740235951, 62.15918302697183151, -3.003915454719715772 ) ) ;
#1018 = FACE_OUTER_BOUND ( 'NONE', #9894, .T. ) ;
#1019 = CARTESIAN_POINT ( 'NONE',  ( 22.80245925209617397, 1.698177091178224130, 5.311506672424976649 ) ) ;
#1021 = ORIENTED_EDGE ( 'NONE', *, *, #22573, .F. ) ;
#1020 = EDGE_LOOP ( 'NONE', ( #6917, #5481, #6006, #10397 ) ) ;
#1022 = CARTESIAN_POINT ( 'NONE',  ( 5.026281758278582146, -30.27593629695115496, 6.864216812889196717 ) ) ;
#1024 = CARTESIAN_POINT ( 'NONE',  ( 86.45541607342296686, 1.246897841450794298, 4.891341099398129444 ) ) ;
#1023 = CARTESIAN_POINT ( 'NONE',  ( 4.550261139223147566, -31.42419555005044529, 6.887945620086119547 ) ) ;
#1025 = CARTESIAN_POINT ( 'NONE',  ( -1.256369394170508080, -27.89135685030788281, 7.740055089680399014 ) ) ;
#1026 = CARTESIAN_POINT ( 'NONE',  ( -63.60792738000480284, 43.84705609857426367, -2.659634298586695422 ) ) ;
#1027 = CARTESIAN_POINT ( 'NONE',  ( 71.74426859761079811, 60.78783288850196698, 3.823636340558493885 ) ) ;
#1028 = CARTESIAN_POINT ( 'NONE',  ( 22.79970795871216183, 3.574398117813434528, -3.863569992082448668 ) ) ;
#1029 = ORIENTED_EDGE ( 'NONE', *, *, #23203, .T. ) ;
#1030 = CARTESIAN_POINT ( 'NONE',  ( 2.340513037401407814, -33.01089774094209872, 7.720710062488891801 ) ) ;
#1031 = ORIENTED_EDGE ( 'NONE', *, *, #32756, .T. ) ;
#1032 = EDGE_CURVE ( 'NONE', #11431, #579, #22616, .T. ) ;
#1033 = AXIS2_PLACEMENT_3D ( 'NONE', #29881, #20807, #8445 ) ;
#1034 = CARTESIAN_POINT ( 'NONE',  ( 21.85643539959776049, -10.96491163060450802, -3.419414754301954851 ) ) ;
#1035 = AXIS2_PLACEMENT_3D ( 'NONE', #17718, #30302, #39763 ) ;
#1036 = B_SPLINE_CURVE_WITH_KNOTS ( 'NONE', 3,
 ( #712, #38554, #16533, #12844, #26023, #25214, #25413, #37743, #22941, #22131 ),
 .UNSPECIFIED., .F., .F.,
 ( 4, 3, 3, 4 ),
 ( 0.0001585009270395677274, 0.0001815657551981830287, 0.0002118214035944111502, 0.0002170292169044726665 ),
 .UNSPECIFIED. ) ;
#1037 = CARTESIAN_POINT ( 'NONE',  ( 20.16883043526225805, 11.76570021213147932, -3.257865388785521787 ) ) ;
#1038 = CARTESIAN_POINT ( 'NONE',  ( 4.043087352902885456, -26.96969281642315863, 7.753200566781576875 ) ) ;
#1039 = CARTESIAN_POINT ( 'NONE',  ( 80.78189192730862089, 64.90162691771338643, 3.235508711566409179 ) ) ;
#1040 = CARTESIAN_POINT ( 'NONE',  ( 88.05979627311084812, -0.5552181473167765446, -3.927858985986737661 ) ) ;
#1041 = ORIENTED_EDGE ( 'NONE', *, *, #23793, .F. ) ;
#1042 = CARTESIAN_POINT ( 'NONE',  ( 14.67409684075444609, -5.611220017537962512, 2.496645725009577266 ) ) ;
#1043 = CARTESIAN_POINT ( 'NONE',  ( 31.19756578357611332, -3.761128863170072112, 4.642324994556521922 ) ) ;
#1044 = CARTESIAN_POINT ( 'NONE',  ( 33.95934880225217967, -3.272301304683462142, -5.506575709182617295 ) ) ;
#1045 = CARTESIAN_POINT ( 'NONE',  ( 33.46266692859374103, -3.084164941913754898, -5.429056490501709575 ) ) ;
#1046 = CARTESIAN_POINT ( 'NONE',  ( 4.921324086407802056, -26.64985754041175525, 6.800000000000000711 ) ) ;
#1047 = CARTESIAN_POINT ( 'NONE',  ( 84.10804491527638049, 3.008217574094829594, -0.3805531846457105294 ) ) ;
#1048 = ADVANCED_FACE ( 'NONE', ( #36597 ), #30425, .F. ) ;
#1049 = EDGE_CURVE ( 'NONE', #35752, #27725, #24236, .T. ) ;
#1050 = CARTESIAN_POINT ( 'NONE',  ( 4.395707693226862389, -31.80270533321202819, 7.743886751744248897 ) ) ;
#1051 = B_SPLINE_CURVE_WITH_KNOTS ( 'NONE', 3,
 ( #27385, #22205, #6549, #12707, #11927, #24087, #39946, #8228, #25281, #11722 ),
 .UNSPECIFIED., .F., .F.,
 ( 4, 3, 3, 4 ),
 ( 1.748223473168675632E-18, 3.025570593002983587E-05, 6.051145698343930035E-05, 6.468151674593807193E-05 ),
 .UNSPECIFIED. ) ;
#1052 = ADVANCED_FACE ( 'NONE', ( #32716 ), #35248, .T. ) ;
#1053 = DIRECTION ( 'NONE',  ( 0.000000000000000000, 0.000000000000000000, 1.000000000000000000 ) ) ;
#1054 = CARTESIAN_POINT ( 'NONE',  ( 30.73573697167703855, -3.645023302247464070, 4.721775058918869838 ) ) ;
#1055 = ORIENTED_EDGE ( 'NONE', *, *, #816, .T. ) ;
#1056 = ORIENTED_EDGE ( 'NONE', *, *, #36941, .T. ) ;
#1057 = CARTESIAN_POINT ( 'NONE',  ( 36.71904603859049843, -3.458174413421041038, 5.860823370863815995 ) ) ;
#1058 = CARTESIAN_POINT ( 'NONE',  ( 1.706484455665669753, -33.06855198763274473, 7.762796336881262249 ) ) ;
#1059 = ORIENTED_EDGE ( 'NONE', *, *, #32997, .F. ) ;
#1060 = CARTESIAN_POINT ( 'NONE',  ( 2.185047844817765483, -33.03621188651298723, 7.751599049952199394 ) ) ;
#1061 = CARTESIAN_POINT ( 'NONE',  ( 87.17674554246272578, -1.585054265969757958, 4.548888058249088040 ) ) ;
#1062 = CIRCLE ( 'NONE', #24030, 0.1000000000000028644 ) ;
#1063 = ORIENTED_EDGE ( 'NONE', *, *, #31441, .T. ) ;
#1064 = AXIS2_PLACEMENT_3D ( 'NONE', #40573, #37291, #8465 ) ;
#1065 = DIRECTION ( 'NONE',  ( 0.000000000000000000, 0.000000000000000000, 1.000000000000000000 ) ) ;
#1066 = ADVANCED_FACE ( 'NONE', ( #18462 ), #18664, .F. ) ;
#1067 =( LENGTH_UNIT ( ) NAMED_UNIT ( * ) SI_UNIT ( .MILLI., .METRE. ) );
#1068 = ORIENTED_EDGE ( 'NONE', *, *, #28555, .F. ) ;
#1069 = CARTESIAN_POINT ( 'NONE',  ( -55.71184120586743660, 30.71742687230106839, -1.474814583819865632 ) ) ;
#1070 = CARTESIAN_POINT ( 'NONE',  ( 8.290806648384990041, 0.000000000000000000, 6.000000000000000000 ) ) ;
#1071 = EDGE_LOOP ( 'NONE', ( #24906, #31817, #31731, #18549, #40271, #17938, #12859, #23182 ) ) ;
#1072 = VECTOR ( 'NONE', #38963, 1000.000000000000000 ) ;
#1073 = CARTESIAN_POINT ( 'NONE',  ( 79.98571111508536546, 66.33520038980104516, -1.398807481800599772 ) ) ;
#1074 = CARTESIAN_POINT ( 'NONE',  ( -40.44874870218063734, -25.49307895267003587, 6.700000000000000178 ) ) ;
#1075 = ORIENTED_EDGE ( 'NONE', *, *, #31430, .F. ) ;
#1076 = CARTESIAN_POINT ( 'NONE',  ( 75.68633765818296411, 59.56198246982955169, -3.184487947857408408 ) ) ;
#1078 = CARTESIAN_POINT ( 'NONE',  ( 0.3454438073187036107, 0.5999999999999995337, -3.946157045896960369 ) ) ;
#1077 = CARTESIAN_POINT ( 'NONE',  ( 2.463123297529182132, -26.15404171320399485, 6.883550009118462931 ) ) ;
#1079 = DIRECTION ( 'NONE',  ( -1.000000000000000000, -0.000000000000000000, -0.000000000000000000 ) ) ;
#1080 = CARTESIAN_POINT ( 'NONE',  ( 75.51044298776176333, 62.93595297499960139, 3.562065002326824992 ) ) ;
#1081 = ORIENTED_EDGE ( 'NONE', *, *, #31234, .T. ) ;
#1082 = CARTESIAN_POINT ( 'NONE',  ( -64.08758708074093136, 37.77454521956559574, 3.093244392761053785 ) ) ;
#1083 = EDGE_CURVE ( 'NONE', #19523, #19287, #35465, .T. ) ;
#1084 = CARTESIAN_POINT ( 'NONE',  ( 4.315404545797473013, -33.85565925846036350, 7.754798119455333705 ) ) ;
#1085 = CARTESIAN_POINT ( 'NONE',  ( 1.217126534916886937, -26.10345411493373291, 7.750000000000000888 ) ) ;
#1086 = LINE ( 'NONE', #32373, #21513 ) ;
#1087 = CARTESIAN_POINT ( 'NONE',  ( 80.30040509403158921, 65.99001427540439124, 2.270757614041262418 ) ) ;
#1088 = CARTESIAN_POINT ( 'NONE',  ( -0.9694501004374326270, -31.83310420932945206, 7.640616322432100205 ) ) ;
#1089 = CARTESIAN_POINT ( 'NONE',  ( 28.53445731760455573, 0.6922391713037714389, -5.301755952056612209 ) ) ;
#1090 = CARTESIAN_POINT ( 'NONE',  ( -70.92837670882107659, -56.35932253828836025, -7.538952224936807056 ) ) ;
#1091 = DIRECTION ( 'NONE',  ( -0.000000000000000000, -0.000000000000000000, -1.000000000000000000 ) ) ;
#1092 = CARTESIAN_POINT ( 'NONE',  ( -80.24641704084613991, -5.629453946137603637, -6.035434990652555953 ) ) ;
#1093 = EDGE_LOOP ( 'NONE', ( #23116, #22958, #9931 ) ) ;
#1094 = CARTESIAN_POINT ( 'NONE',  ( -0.5792506522025446802, -32.09249774648650089, 6.863904403958575706 ) ) ;
#1095 = CARTESIAN_POINT ( 'NONE',  ( 66.93722180744200045, 57.81789296588414118, 3.995856122844018810 ) ) ;
#1096 = EDGE_CURVE ( 'NONE', #25156, #27940, #9398, .T. ) ;
#1097 = CARTESIAN_POINT ( 'NONE',  ( 36.02633504632637340, -1.730128226848125950, -5.776816043798858047 ) ) ;
#1098 = CARTESIAN_POINT ( 'NONE',  ( 1.012709997867073053, -32.89967220964104655, 7.774064877406528851 ) ) ;
#1099 = CARTESIAN_POINT ( 'NONE',  ( 4.979285396424428356, -28.34565668833202778, 7.730015791551950954 ) ) ;
#1100 =( BOUNDED_CURVE ( )  B_SPLINE_CURVE ( 3, ( #29336, #4230, #16755, #22564 ),
 .UNSPECIFIED., .F., .T. ) 
 B_SPLINE_CURVE_WITH_KNOTS ( ( 4, 4 ),
 ( 1.381924640371168467, 1.574767692156076482 ),
 .UNSPECIFIED. ) 
 CURVE ( )  GEOMETRIC_REPRESENTATION_ITEM ( )  RATIONAL_B_SPLINE_CURVE ( ( 1.000000000000000000, 0.9969033633783032089, 0.9969033633783032089, 1.000000000000000000 ) ) 
 REPRESENTATION_ITEM ( '' )  );
#1101 = CARTESIAN_POINT ( 'NONE',  ( 3.295664264696410495, -32.57244657952615086, 7.757178535559533294 ) ) ;
#1102 = CARTESIAN_POINT ( 'NONE',  ( -1.585292354492739975, -28.37344205933749208, 7.767720160662274331 ) ) ;
#1103 = CIRCLE ( 'NONE', #32653, 67.42751648247021024 ) ;
#1104 = EDGE_CURVE ( 'NONE', #38102, #33506, #2654, .T. ) ;
#1105 = CARTESIAN_POINT ( 'NONE',  ( 21.85643539959776760, -15.11427361947482062, -2.500000000000000000 ) ) ;
#1106 = CARTESIAN_POINT ( 'NONE',  ( -63.99293516169446150, 35.89893413629672381, 12.49999999999999645 ) ) ;
#1107 = CARTESIAN_POINT ( 'NONE',  ( 31.81222844470352840, -2.964472128955970121, 5.171465649085067895 ) ) ;
#1108 = CIRCLE ( 'NONE', #9635, 0.1000000000000028644 ) ;
#1109 = EDGE_LOOP ( 'NONE', ( #22255, #22599 ) ) ;
#1110 = CARTESIAN_POINT ( 'NONE',  ( 36.54090531688899546, -2.167697392235706566, 5.903356262276473032 ) ) ;
#1111 = CARTESIAN_POINT ( 'NONE',  ( -34.44874870218064444, -26.64985754041175525, 6.800000000000000711 ) ) ;
#1112 = CARTESIAN_POINT ( 'NONE',  ( 67.36808046129075933, 58.37408278799862416, -3.989212576213368333 ) ) ;
#1113 = CARTESIAN_POINT ( 'NONE',  ( 3.075873696215302378, -26.35153850715824575, 6.941203072598471913 ) ) ;
#1114 = VERTEX_POINT ( 'NONE', #9198 ) ;
#1115 = CARTESIAN_POINT ( 'NONE',  ( -18.27651686900387418, -64.04014080848075707, 2.500000000000000000 ) ) ;
#1116 = CARTESIAN_POINT ( 'NONE',  ( 30.87880611384830587, -3.486100459600208090, 4.898406253664910892 ) ) ;
#1117 = CARTESIAN_POINT ( 'NONE',  ( -59.99245622168610481, 24.84364830758654463, 9.341017543843767257 ) ) ;
#1118 = CARTESIAN_POINT ( 'NONE',  ( 0.9577497276855772013, -32.88784831336140968, 6.871394612369935651 ) ) ;
#1119 =( REPRESENTATION_RELATIONSHIP ('NONE','NONE', #24012, #27999 ) REPRESENTATION_RELATIONSHIP_WITH_TRANSFORMATION ( #18196 )SHAPE_REPRESENTATION_RELATIONSHIP( ) );
#1120 = ADVANCED_FACE ( 'NONE', ( #27731 ), #11866, .T. ) ;
#1121 = CARTESIAN_POINT ( 'NONE',  ( 0.4628871221125078761, -32.84386297521798070, 6.883108633650832253 ) ) ;
#1122 = CARTESIAN_POINT ( 'NONE',  ( -0.000000000000000000, 10.37661300689600097, -2.500000000000000000 ) ) ;
#1123 = VERTEX_POINT ( 'NONE', #40087 ) ;
#1124 = CARTESIAN_POINT ( 'NONE',  ( 24.75831320048713735, 3.019228828327055858, 3.350538031934082284 ) ) ;
#1125 = CARTESIAN_POINT ( 'NONE',  ( -40.44874870218063734, -25.49307895267003587, 6.700000000000000178 ) ) ;
#1126 = CARTESIAN_POINT ( 'NONE',  ( 79.14790672806259408, 65.85151465993942566, 2.407735119910381361 ) ) ;
#1127 = CARTESIAN_POINT ( 'NONE',  ( 25.22329213065313169, -5.090999687581535760, -2.500000000044154014 ) ) ;
#1128 = VERTEX_POINT ( 'NONE', #31251 ) ;
#1129 = CARTESIAN_POINT ( 'NONE',  ( 79.02450826907198689, 62.91033389078318550, -3.791687334209853599 ) ) ;
#1131 = CARTESIAN_POINT ( 'NONE',  ( -1.709556888978058131, -28.78108823880591416, 6.917411966759697606 ) ) ;
#1130 = CARTESIAN_POINT ( 'NONE',  ( 24.12373500254816605, 0.4971700199039688073, 5.094523214884540074 ) ) ;
#1132 = VECTOR ( 'NONE', #3813, 1000.000000000000000 ) ;
#1133 = CARTESIAN_POINT ( 'NONE',  ( 79.91673984739684045, 65.77987873796998031, -2.647945256399896419 ) ) ;
#1134 = CARTESIAN_POINT ( 'NONE',  ( 78.83212471655066622, 64.69929012837440041, 3.375657603866063727 ) ) ;
#1135 = CIRCLE ( 'NONE', #6382, 0.1000000000000028644 ) ;
#1136 = ADVANCED_FACE ( 'NONE', ( #21366 ), #40284, .T. ) ;
#1137 = CARTESIAN_POINT ( 'NONE',  ( -1.432293644835494373, -27.47664038617742577, 1.000000000000000000 ) ) ;
#1138 = CARTESIAN_POINT ( 'NONE',  ( 81.88789819931513136, 65.48572365615882518, 1.161365684106807850 ) ) ;
#1139 = CARTESIAN_POINT ( 'NONE',  ( -63.70251272992033620, 44.36816940802074782, 1.449983087898546463 ) ) ;
#1140 = CARTESIAN_POINT ( 'NONE',  ( 22.31759743831440090, 6.226164879696757026, 1.431367841762869686 ) ) ;
#1141 = CARTESIAN_POINT ( 'NONE',  ( -63.15778550246169232, 35.55392038829429424, -6.471101796987086985 ) ) ;
#1142 = VERTEX_POINT ( 'NONE', #37201 ) ;
#1143 = CARTESIAN_POINT ( 'NONE',  ( -76.06876986340937208, -4.053555619469175753, 8.607033718690072277 ) ) ;
#1144 = CARTESIAN_POINT ( 'NONE',  ( -12.99139449055068241, 13.37661300689600097, 6.000000000000000000 ) ) ;
#1145 = ADVANCED_FACE ( 'NONE', ( #40479 ), #21777, .F. ) ;
#1146 = CARTESIAN_POINT ( 'NONE',  ( -0.07982934255991593064, -32.56666002521691183, 7.785096263473210598 ) ) ;
#1147 = CARTESIAN_POINT ( 'NONE',  ( -0.9728551256764975674, -31.82908634522761560, 7.756742906098587298 ) ) ;
#1148 = EDGE_CURVE ( 'NONE', #7017, #3657, #26261, .T. ) ;
#1149 = VERTEX_POINT ( 'NONE', #37403 ) ;
#1150 = CARTESIAN_POINT ( 'NONE',  ( 37.01014894729547677, -2.248942906826801202, -5.913016239383465766 ) ) ;
#1151 = CARTESIAN_POINT ( 'NONE',  ( 30.76700883330015301, -3.320931493643032084, -4.963836536440328295 ) ) ;
#1152 = DIRECTION ( 'NONE',  ( -0.000000000000000000, -0.000000000000000000, 1.000000000000000000 ) ) ;
#1153 = CARTESIAN_POINT ( 'NONE',  ( -1.097841762937593613, -31.67228564313648320, 6.980586498568973397 ) ) ;
#1154 = CARTESIAN_POINT ( 'NONE',  ( 5.195112791980205813, -29.76205841885524350, 6.951256099901581997 ) ) ;
#1155 = CARTESIAN_POINT ( 'NONE',  ( -0.5686205303572778869, -26.90504279848119040, 7.651421919295151142 ) ) ;
#1156 = DIRECTION ( 'NONE',  ( -0.4826092789263672911, 0.5751513419797894544, 0.6605219282605377940 ) ) ;
#1157 = EDGE_CURVE ( 'NONE', #22987, #8010, #30329, .T. ) ;
#1158 = VECTOR ( 'NONE', #8175, 1000.000000000000000 ) ;
#1159 = CARTESIAN_POINT ( 'NONE',  ( 4.296241352401964697, -27.37412594797728715, 7.635761828346577573 ) ) ;
#1160 = CARTESIAN_POINT ( 'NONE',  ( 22.83119761409040294, 1.181603121085857078, -5.687369041816118909 ) ) ;
#1161 = EDGE_CURVE ( 'NONE', #12672, #5311, #17051, .T. ) ;
#1162 = ORIENTED_EDGE ( 'NONE', *, *, #19712, .F. ) ;
#1163 = VECTOR ( 'NONE', #24219, 1000.000000000000000 ) ;
#1164 = CARTESIAN_POINT ( 'NONE',  ( 66.83382626670835691, 58.02146702699413794, 3.998465113256441050 ) ) ;
#1165 = VECTOR ( 'NONE', #34063, 1000.000000000000000 ) ;
#1166 = CIRCLE ( 'NONE', #39261, 0.1000000000000028644 ) ;
#1167 = DIRECTION ( 'NONE',  ( 0.4999999999999980016, 0.8660254037844398178, -0.000000000000000000 ) ) ;
#1168 = CARTESIAN_POINT ( 'NONE',  ( 84.24490603200722205, 3.007448030680667017, 1.128815683486722454 ) ) ;
#1169 = ORIENTED_EDGE ( 'NONE', *, *, #23859, .F. ) ;
#1170 = CARTESIAN_POINT ( 'NONE',  ( -72.85671063792464963, 2.859724406437386346, -10.96068470457861999 ) ) ;
#1171 = B_SPLINE_CURVE_WITH_KNOTS ( 'NONE', 3,
 ( #13418, #35872, #19809, #10123, #22712, #32187, #32584, #32384, #3985, #4178, #16695, #16504, #29081, #29485, #7651, #29281, #20202, #26200, #38731, #23106, #8441, #27599, #11935, #39537, #15037, #8039, #17298, #36263, #1691, #20596, #11323 ),
 .UNSPECIFIED., .F., .F.,
 ( 4, 3, 3, 3, 3, 3, 3, 3, 3, 3, 4 ),
 ( 1.022834283856302764E-18, 2.999644130997711973E-05, 6.002588995694830702E-05, 8.960886084587982281E-05, 0.0001190604700446476022, 0.0001489538463052710970, 0.0001796139255493959305, 0.0002109707048517047475, 0.0002426195318110325918, 0.0002740640997890037445, 0.0002849778069099849075 ),
 .UNSPECIFIED. ) ;
#1172 = CARTESIAN_POINT ( 'NONE',  ( 2.963766215430877260, -26.31911081783852779, 7.782861076432730840 ) ) ;
#1173 = DIRECTION ( 'NONE',  ( -0.000000000000000000, -0.000000000000000000, 1.000000000000000000 ) ) ;
#1174 = ORIENTED_EDGE ( 'NONE', *, *, #2356, .F. ) ;
#1175 = CARTESIAN_POINT ( 'NONE',  ( 5.052185455143900938, -30.14046697283304255, 7.643333865083955736 ) ) ;
#1176 = ORIENTED_EDGE ( 'NONE', *, *, #3818, .T. ) ;
#1177 = VERTEX_POINT ( 'NONE', #12903 ) ;
#1178 = CARTESIAN_POINT ( 'NONE',  ( 79.69769351933607027, 63.91149418591603393, -3.725738571856551662 ) ) ;
#1179 = CARTESIAN_POINT ( 'NONE',  ( 33.60131552963068913, -4.188911086009777129, 4.688672432858080441 ) ) ;
#1180 = CARTESIAN_POINT ( 'NONE',  ( 78.73521632358557554, 65.70333808056840041, 2.340042473998457773 ) ) ;
#1181 = CARTESIAN_POINT ( 'NONE',  ( 24.18364339310534916, 2.677224417268836199, 3.980840453756503194 ) ) ;
#1182 = DIRECTION ( 'NONE',  ( 1.000000000000000000, 0.000000000000000000, 0.000000000000000000 ) ) ;
#1183 = CYLINDRICAL_SURFACE ( 'NONE', #24845, 12.80480339192541628 ) ;
#1184 = AXIS2_PLACEMENT_3D ( 'NONE', #34946, #32055, #6726 ) ;
#1185 = CARTESIAN_POINT ( 'NONE',  ( 21.85643539959778181, 2.657715471900086612, -15.25567151318962367 ) ) ;
#1186 = DIRECTION ( 'NONE',  ( -1.000000000000000000, -3.905578250920211148E-15, 0.000000000000000000 ) ) ;
#1187 = LINE ( 'NONE', #35955, #946 ) ;
#1188 = CYLINDRICAL_SURFACE ( 'NONE', #2503, 0.09010775117052992333 ) ;
#1189 = CIRCLE ( 'NONE', #4471, 10.00000000000000533 ) ;
#1190 = VERTEX_POINT ( 'NONE', #4067 ) ;
#1191 = CARTESIAN_POINT ( 'NONE',  ( -1.766059499949450773, -30.05349463170571767, 6.867199677474202346 ) ) ;
#1192 = CARTESIAN_POINT ( 'NONE',  ( 4.281682929012584182, -27.35702998321412593, 7.695279973900954751 ) ) ;
#1193 = CARTESIAN_POINT ( 'NONE',  ( -75.00170219041523012, -3.073105394106712129, -9.174977135382700766 ) ) ;
#1194 = FACE_OUTER_BOUND ( 'NONE', #38012, .T. ) ;
#1195 = DIRECTION ( 'NONE',  ( 0.000000000000000000, 1.000000000000000000, 0.000000000000000000 ) ) ;
#1196 = CARTESIAN_POINT ( 'NONE',  ( 81.31277617166799132, 62.04138461958081052, 2.639511535887547833 ) ) ;
#1197 = CARTESIAN_POINT ( 'NONE',  ( -71.72837670882105954, -31.30579396504363388, -1.385640646055078307 ) ) ;
#1198 = DIRECTION ( 'NONE',  ( 0.7660444431189857850, -0.6427876096865299260, -0.000000000000000000 ) ) ;
#1199 = CARTESIAN_POINT ( 'NONE',  ( 2.931042139431549565, -32.84643678970255110, 7.700536657684216912 ) ) ;
#1200 = FACE_OUTER_BOUND ( 'NONE', #32712, .T. ) ;
#1201 = ADVANCED_FACE ( 'NONE', ( #35560 ), #30903, .T. ) ;
#1202 = CARTESIAN_POINT ( 'NONE',  ( 1.671100228160198764, -26.17005511905719217, 7.730758795053807475 ) ) ;
#1203 = CARTESIAN_POINT ( 'NONE',  ( -0.3331733235464042209, -26.84510637993277271, 7.006423389747791219 ) ) ;
#1204 = EDGE_CURVE ( 'NONE', #22060, #24466, #16197, .T. ) ;
#1205 = CARTESIAN_POINT ( 'NONE',  ( 4.918762182065622213, -28.47348944886545397, 7.784476445165072533 ) ) ;
#1206 = CARTESIAN_POINT ( 'NONE',  ( -1.577774374486538678, -28.34370111728035013, 6.894806418505347700 ) ) ;
#1207 = AXIS2_PLACEMENT_3D ( 'NONE', #23187, #22594, #13911 ) ;
#1208 = DIRECTION ( 'NONE',  ( 0.6427876096865379196, 0.7660444431189793457, -0.000000000000000000 ) ) ;
#1209 = CARTESIAN_POINT ( 'NONE',  ( 69.35860043680946774, 58.39594701590269921, 3.954017255840814649 ) ) ;
#1210 = CARTESIAN_POINT ( 'NONE',  ( 34.33337444863689569, -1.484546483778259818, 5.564951457145235203 ) ) ;
#1211 = CYLINDRICAL_SURFACE ( 'NONE', #10209, 0.1000000000000028644 ) ;
#1212 = CARTESIAN_POINT ( 'NONE',  ( 85.85116863490735284, 1.861966474136578231, -4.950709030323501736 ) ) ;
#1214 = CARTESIAN_POINT ( 'NONE',  ( -0.4597662833393237336, -26.81607390015101799, 6.865482280155367434 ) ) ;
#1213 = CARTESIAN_POINT ( 'NONE',  ( 80.83425215363003247, 63.04220640063321213, -3.443978770203981021 ) ) ;
#1215 = CARTESIAN_POINT ( 'NONE',  ( -1.302730225678609965, -27.77235727801802057, 6.875671892026061549 ) ) ;
#1216 = AXIS2_PLACEMENT_3D ( 'NONE', #27119, #20943, #2227 ) ;
#1217 = CARTESIAN_POINT ( 'NONE',  ( -59.07422214908515201, 27.36241337473658319, 4.461357708502259101 ) ) ;
#1218 = ORIENTED_EDGE ( 'NONE', *, *, #19193, .T. ) ;
#1219 = CARTESIAN_POINT ( 'NONE',  ( 6.396068641104377228, -30.45570603157191769, 7.013842709614101167 ) ) ;
#1220 = PLANE ( 'NONE',  #30647 ) ;
#1221 = EDGE_LOOP ( 'NONE', ( #16790, #18819, #34634, #35996, #28546 ) ) ;
#1222 = CARTESIAN_POINT ( 'NONE',  ( -0.9146243593313261311, -25.28420110832643886, 7.754798119455333705 ) ) ;
#1223 = EDGE_LOOP ( 'NONE', ( #35956, #16011, #20211, #34093 ) ) ;
#1224 = CARTESIAN_POINT ( 'NONE',  ( 80.93223178899225445, 61.91756539228702394, -2.804471013201356389 ) ) ;
#1225 = FACE_OUTER_BOUND ( 'NONE', #8192, .T. ) ;
#1226 = CARTESIAN_POINT ( 'NONE',  ( 80.47318323629869496, 63.22351390842204211, 3.619557188109058021 ) ) ;
#1227 = CARTESIAN_POINT ( 'NONE',  ( 25.36303923114378733, 1.426800422063377427, 4.397790789347460816 ) ) ;
#1228 = ORIENTED_EDGE ( 'NONE', *, *, #3853, .F. ) ;
#1229 = CARTESIAN_POINT ( 'NONE',  ( 5.035164781800626876, -30.23278213633238209, 6.874555630061440326 ) ) ;
#1230 = CIRCLE ( 'NONE', #24210, 10.00000000000000888 ) ;
#1232 = FACE_OUTER_BOUND ( 'NONE', #23037, .T. ) ;
#1231 = CARTESIAN_POINT ( 'NONE',  ( -58.64136512043187821, 29.17320997702626428, -5.450418868401677663 ) ) ;
#1233 = CARTESIAN_POINT ( 'NONE',  ( -1.694464052375517671, -29.38293999636734810, 7.013842709614101167 ) ) ;
#1234 = CARTESIAN_POINT ( 'NONE',  ( -63.37350057586147045, 42.57076579999920796, -3.677910432553653131 ) ) ;
#1235 = CARTESIAN_POINT ( 'NONE',  ( -40.44874870218063734, -26.64985754041175525, 6.700000000000000178 ) ) ;
#1236 = CARTESIAN_POINT ( 'NONE',  ( 23.41943767133188814, 3.656341323882381200, -3.349654434191691621 ) ) ;
#1237 = ORIENTED_EDGE ( 'NONE', *, *, #1249, .T. ) ;
#1238 = DIRECTION ( 'NONE',  ( 0.000000000000000000, 0.000000000000000000, 1.000000000000000000 ) ) ;
#1239 = CARTESIAN_POINT ( 'NONE',  ( 22.37806265499392566, 3.168015787195890720, 7.828147373443384183 ) ) ;
#1240 = CARTESIAN_POINT ( 'NONE',  ( 21.86870537176919527, 3.698784010464675198, 3.388912068464415395 ) ) ;
#1241 = CARTESIAN_POINT ( 'NONE',  ( 0.3419956299568869262, -32.68678192801872484, 6.949473656533215582 ) ) ;
#1242 = CARTESIAN_POINT ( 'NONE',  ( 81.48469013494974433, 61.56585122427133427, 1.622497907168700682 ) ) ;
#1243 = CARTESIAN_POINT ( 'NONE',  ( 84.68420644151177612, 2.996072101527111453, 1.894685230139086851 ) ) ;
#1244 = ORIENTED_EDGE ( 'NONE', *, *, #36356, .F. ) ;
#1245 = AXIS2_PLACEMENT_3D ( 'NONE', #21698, #24156, #2774 ) ;
#1246 = PLANE ( 'NONE',  #30331 ) ;
#1247 = CARTESIAN_POINT ( 'NONE',  ( 31.01275874060653592, -3.765090545890084961, 4.604780786014718963 ) ) ;
#1248 = CARTESIAN_POINT ( 'NONE',  ( 33.12677655050840997, -3.093949257744326609, -5.376632673462000689 ) ) ;
#1249 = EDGE_CURVE ( 'NONE', #12996, #5611, #7868, .T. ) ;
#1250 = CARTESIAN_POINT ( 'NONE',  ( 36.63309929816978894, -3.078772421412805382, -5.923879138970663760 ) ) ;
#1251 = CARTESIAN_POINT ( 'NONE',  ( -14.24874870218063450, -25.49307895267003587, 6.700000000000000178 ) ) ;
#1252 = CARTESIAN_POINT ( 'NONE',  ( 84.43366413210182486, 2.606424049041346169, 3.204991622768011084 ) ) ;
#1253 = CARTESIAN_POINT ( 'NONE',  ( -2.735299443412492426, -31.17001996922091678, 7.635761828346577573 ) ) ;
#1254 = ORIENTED_EDGE ( 'NONE', *, *, #35907, .T. ) ;
#1255 = DIRECTION ( 'NONE',  ( 1.000000000000000000, 0.000000000000000000, 0.000000000000000000 ) ) ;
#1256 = CARTESIAN_POINT ( 'NONE',  ( -1.644646209780476820, -30.17880794741612505, 7.748216051605118615 ) ) ;
#1257 = CARTESIAN_POINT ( 'NONE',  ( 4.990378111456791999, -28.41860493638662888, 7.785096263473211486 ) ) ;
#1258 = ORIENTED_EDGE ( 'NONE', *, *, #18494, .T. ) ;
#1259 = ORIENTED_EDGE ( 'NONE', *, *, #27979, .T. ) ;
#1260 = CARTESIAN_POINT ( 'NONE',  ( 29.48809767354670086, 1.219317615460245641, 4.222743620664576092 ) ) ;
#1261 = CARTESIAN_POINT ( 'NONE',  ( 15.55633224523761982, -3.531369950178294914, 2.634339896823157723 ) ) ;
#1262 = CARTESIAN_POINT ( 'NONE',  ( -62.89148181836064566, 37.17958841060804076, -4.327622075140624247 ) ) ;
#1263 = CARTESIAN_POINT ( 'NONE',  ( 87.90175190873620181, -2.482191174542180523, 0.8726593636648759533 ) ) ;
#1264 = ORIENTED_EDGE ( 'NONE', *, *, #31818, .F. ) ;
#1265 = CARTESIAN_POINT ( 'NONE',  ( 2.406735030961865363, -33.78287863190474383, 7.695279973900954751 ) ) ;
#1266 = CARTESIAN_POINT ( 'NONE',  ( -58.49128007771433602, 30.53048970692593400, -5.009453334674668135 ) ) ;
#1267 = EDGE_CURVE ( 'NONE', #26853, #22787, #24958, .T. ) ;
#1268 = CARTESIAN_POINT ( 'NONE',  ( 3.799857242690032777, -32.37032976418250740, 6.941203072598476354 ) ) ;
#1269 = VERTEX_POINT ( 'NONE', #3673 ) ;
#1270 = CARTESIAN_POINT ( 'NONE',  ( 22.92431439707159058, 4.119491578302444168, 3.288696840953844625 ) ) ;
#1271 = CARTESIAN_POINT ( 'NONE',  ( 79.60403240858884999, 66.28972460246984610, -1.461108304022175730 ) ) ;
#1272 = CARTESIAN_POINT ( 'NONE',  ( 5.885943586549580608, -28.70822073431874344, 7.754798119455333705 ) ) ;
#1273 = AXIS2_PLACEMENT_3D ( 'NONE', #4046, #3453, #6716 ) ;
#1274 = CARTESIAN_POINT ( 'NONE',  ( -1.627984416835427162, -30.65173788820889200, 7.754798119455333705 ) ) ;
#1275 = ORIENTED_EDGE ( 'NONE', *, *, #39239, .T. ) ;
#1277 = CARTESIAN_POINT ( 'NONE',  ( 4.419915592368481860, -27.38632609080736557, 7.782861076432731728 ) ) ;
#1276 = CARTESIAN_POINT ( 'NONE',  ( -1.593127767899503722, -28.38555688987459291, 7.635761828346575797 ) ) ;
#1278 = CARTESIAN_POINT ( 'NONE',  ( 22.07118065842499277, 4.795981446113927404, -3.651139553905330182 ) ) ;
#1279 = EDGE_CURVE ( 'NONE', #38902, #32411, #11629, .T. ) ;
#1280 = CARTESIAN_POINT ( 'NONE',  ( 76.54556538389320508, 62.22002718612346683, 3.872369636030853712 ) ) ;
#1281 = CARTESIAN_POINT ( 'NONE',  ( 22.04371986193802968, 2.335811073793032211, -5.477320531203638154 ) ) ;
#1282 = CARTESIAN_POINT ( 'NONE',  ( -70.92837670881976919, 0.2170085631237942680, 10.00000000000113154 ) ) ;
#1283 = EDGE_CURVE ( 'NONE', #1015, #486, #19030, .T. ) ;
#1284 = DIRECTION ( 'NONE',  ( -1.000000000000000000, -1.165409145176970240E-16, 0.000000000000000000 ) ) ;
#1285 = CARTESIAN_POINT ( 'NONE',  ( -35.07867591359219972, -24.55319635012989110, 6.700000000000000178 ) ) ;
#1286 = CARTESIAN_POINT ( 'NONE',  ( -62.74545191947990475, 35.90010598104516504, 5.266623911128414548 ) ) ;
#1287 = CARTESIAN_POINT ( 'NONE',  ( -5.078675913592192614, -26.64985754041175525, 6.800000000000000711 ) ) ;
#1288 = CARTESIAN_POINT ( 'NONE',  ( 81.40691186390338885, 61.43583663329575728, 1.251938014746357242 ) ) ;
#1289 = CARTESIAN_POINT ( 'NONE',  ( -0.1048951552736917536, -32.56843413746527460, 6.870737987065012042 ) ) ;
#1290 = CARTESIAN_POINT ( 'NONE',  ( 31.58133870531054654, -3.380569343585269504, 5.164673136779329710 ) ) ;
#1291 = CARTESIAN_POINT ( 'NONE',  ( 7.121324086407810228, -26.64985754041175525, 6.700000000000000178 ) ) ;
#1292 = CARTESIAN_POINT ( 'NONE',  ( 8.290806648384990041, -25.50263309590217276, 27.90461065042423527 ) ) ;
#1293 = FACE_OUTER_BOUND ( 'NONE', #4220, .T. ) ;
#1294 = CARTESIAN_POINT ( 'NONE',  ( -0.5714818571711197670, -32.09947517033602793, 6.864276522220859711 ) ) ;
#1295 = CARTESIAN_POINT ( 'NONE',  ( 3.925174318192090617, -26.86801694415465747, 7.670465701733752972 ) ) ;
#1296 = EDGE_CURVE ( 'NONE', #8875, #10017, #1826, .T. ) ;
#1297 = CARTESIAN_POINT ( 'NONE',  ( 36.21777210603757169, -2.179854984378739591, -5.859057285912292024 ) ) ;
#1298 = LINE ( 'NONE', #26205, #3633 ) ;
#1299 = FACE_OUTER_BOUND ( 'NONE', #3763, .T. ) ;
#1300 = CARTESIAN_POINT ( 'NONE',  ( 4.998117124696596747, -33.55594714837163650, 7.695279973900954751 ) ) ;
#1301 = CARTESIAN_POINT ( 'NONE',  ( -1.544665293549569052, -28.25920506871950622, 7.754798119455333705 ) ) ;
#1302 = CARTESIAN_POINT ( 'NONE',  ( -0.4574464213436950089, -32.19742739189324254, 7.692469944509193525 ) ) ;
#1303 = CYLINDRICAL_SURFACE ( 'NONE', #14814, 0.1000000000000028644 ) ;
#1304 = ORIENTED_EDGE ( 'NONE', *, *, #8540, .T. ) ;
#1305 = CARTESIAN_POINT ( 'NONE',  ( 25.49146503112114459, 2.250848193396226993, 4.142220051770394207 ) ) ;
#1306 = CARTESIAN_POINT ( 'NONE',  ( -70.39213229241123315, 0.06107131307206801335, 5.988032920670404380 ) ) ;
#1307 = CARTESIAN_POINT ( 'NONE',  ( 67.20175956769865877, 57.92120807820956685, -3.995511504169228179 ) ) ;
#1308 = EDGE_CURVE ( 'NONE', #14269, #28383, #9170, .T. ) ;
#1309 = CARTESIAN_POINT ( 'NONE',  ( 3.066970013825967900, -26.34774553824737708, 6.912143950357344302 ) ) ;
#1310 = ORIENTED_EDGE ( 'NONE', *, *, #18970, .T. ) ;
#1311 = B_SPLINE_CURVE_WITH_KNOTS ( 'NONE', 3,
 ( #29663, #20585, #39943, #39326, #39736, #11310 ),
 .UNSPECIFIED., .F., .F.,
 ( 4, 2, 4 ),
 ( 0.000000000000000000, 0.001088541862127108796, 0.002177083724254217593 ),
 .UNSPECIFIED. ) ;
#1312 = DIRECTION ( 'NONE',  ( -0.7508067542896625923, -2.621427771679738966E-15, -0.6605219282605402364 ) ) ;
#1313 = FACE_OUTER_BOUND ( 'NONE', #22762, .T. ) ;
#1314 = CARTESIAN_POINT ( 'NONE',  ( 85.65063761622859317, 0.8893949271338112972, -5.850088623745237193 ) ) ;
#1315 = CARTESIAN_POINT ( 'NONE',  ( 0.9049691096044686356, -32.87557774234537789, 6.969307238440506147 ) ) ;
#1316 = DIRECTION ( 'NONE',  ( -0.000000000000000000, -0.000000000000000000, 1.000000000000000000 ) ) ;
#1317 = VERTEX_POINT ( 'NONE', #30167 ) ;
#1318 = CARTESIAN_POINT ( 'NONE',  ( 24.39763012491684080, 3.159636959096371100, 3.289163722610739082 ) ) ;
#1319 =( NAMED_UNIT ( * ) SI_UNIT ( $, .STERADIAN. ) SOLID_ANGLE_UNIT ( ) );
#1320 = CARTESIAN_POINT ( 'NONE',  ( 17.92594389746831851, -3.172814633591019451, 2.962253944291116436 ) ) ;
#1321 = CARTESIAN_POINT ( 'NONE',  ( 79.82117971689783076, 65.09389273565577128, 3.300462285847911570 ) ) ;
#1322 = CARTESIAN_POINT ( 'NONE',  ( -63.24203369823550247, 41.86349869517832900, 3.933568017676808193 ) ) ;
#1323 = VERTEX_POINT ( 'NONE', #39007 ) ;
#1324 = CARTESIAN_POINT ( 'NONE',  ( 79.37220710802424151, 62.20501526703845485, -3.590127757398436703 ) ) ;
#1326 = CARTESIAN_POINT ( 'NONE',  ( -5.078675913592192614, -24.55319635012989110, 6.800000000000000711 ) ) ;
#1325 = CARTESIAN_POINT ( 'NONE',  ( 23.05869099769193653, 0.3511655747170696062, 5.953694451861818671 ) ) ;
#1327 = ADVANCED_FACE ( 'NONE', ( #20280 ), #4653, .T. ) ;
#1328 = EDGE_CURVE ( 'NONE', #24028, #6532, #20952, .T. ) ;
#1329 = CARTESIAN_POINT ( 'NONE',  ( 81.64294641039653300, 62.46883698081568781, -2.647945256399892422 ) ) ;
#1330 = CARTESIAN_POINT ( 'NONE',  ( 79.88615925706736220, 62.68050235454665398, 3.612066323963901482 ) ) ;
#1331 = ADVANCED_FACE ( 'NONE', ( #20901 ), #9845, .T. ) ;
#1332 = AXIS2_PLACEMENT_3D ( 'NONE', #24016, #5096, #8576 ) ;
#1333 = CARTESIAN_POINT ( 'NONE',  ( -1.628563930502259671, -30.65045316922430985, 7.753200566781576875 ) ) ;
#1334 = CARTESIAN_POINT ( 'NONE',  ( 80.37799020243589609, 66.31529150154187846, 1.204231967107850076 ) ) ;
#1335 =( BOUNDED_CURVE ( )  B_SPLINE_CURVE ( 3, ( #4532, #4336, #38084, #3943 ),
 .UNSPECIFIED., .F., .T. ) 
 B_SPLINE_CURVE_WITH_KNOTS ( ( 4, 4 ),
 ( 4.748221474220560623, 4.941946782021396700 ),
 .UNSPECIFIED. ) 
 CURVE ( )  GEOMETRIC_REPRESENTATION_ITEM ( )  RATIONAL_B_SPLINE_CURVE ( ( 1.000000000000000000, 0.9968749865767494445, 0.9968749865767494445, 1.000000000000000000 ) ) 
 REPRESENTATION_ITEM ( '' )  );
#1336 = CARTESIAN_POINT ( 'NONE',  ( -64.08758708074093136, 42.98467135419826235, 2.320054402708805696 ) ) ;
#1337 = CARTESIAN_POINT ( 'NONE',  ( 30.01304521823198712, -3.946539318896107318, -3.661452490695084272 ) ) ;
#1338 = CARTESIAN_POINT ( 'NONE',  ( -64.08758708074093136, 35.87095250353018372, -3.952250494627737254 ) ) ;
#1339 = ORIENTED_EDGE ( 'NONE', *, *, #33464, .T. ) ;
#1340 = CARTESIAN_POINT ( 'NONE',  ( -80.58488676320212107, -5.645780868419546294, 5.363795197840156348 ) ) ;
#1341 = CARTESIAN_POINT ( 'NONE',  ( 24.74496925782481682, 0.5731625295932825104, -4.778242445000019600 ) ) ;
#1342 = CARTESIAN_POINT ( 'NONE',  ( -2.689021718275399042, -31.29716697405881476, 7.754798119455333705 ) ) ;
#1343 = ORIENTED_EDGE ( 'NONE', *, *, #10404, .T. ) ;
#1344 = CARTESIAN_POINT ( 'NONE',  ( -2.448748702180640446, -26.64985754041175525, 6.800000000000000711 ) ) ;
#1345 = VECTOR ( 'NONE', #9294, 1000.000000000000000 ) ;
#1346 = VERTEX_POINT ( 'NONE', #25375 ) ;
#1347 = CARTESIAN_POINT ( 'NONE',  ( 36.13237780866466409, -1.531151423559755198, -5.643717596868586206 ) ) ;
#1348 = CARTESIAN_POINT ( 'NONE',  ( -2.617163280481567433, -29.45682925621299475, 6.894806418505347700 ) ) ;
#1349 = DIRECTION ( 'NONE',  ( -1.000000000000000000, 0.000000000000000000, 0.000000000000000000 ) ) ;
#1350 = CARTESIAN_POINT ( 'NONE',  ( -1.066124925935248546, -31.71387034028391838, 6.870724624169668893 ) ) ;
#1351 = EDGE_CURVE ( 'NONE', #38060, #32211, #36785, .T. ) ;
#1352 = DIRECTION ( 'NONE',  ( 0.000000000000000000, 0.000000000000000000, 1.000000000000000000 ) ) ;
#1353 = CARTESIAN_POINT ( 'NONE',  ( 1.295029243323604806, -26.19418099523372945, 7.013842709614101167 ) ) ;
#1354 = CARTESIAN_POINT ( 'NONE',  ( -4.266520354791871306, -48.67644278316300444, 6.000000000000000000 ) ) ;
#1355 = B_SPLINE_CURVE_WITH_KNOTS ( 'NONE', 3,
 ( #17928, #2115, #15258, #21240 ),
 .UNSPECIFIED., .F., .F.,
 ( 4, 4 ),
 ( 0.0002401580581033240186, 0.001136201907775618225 ),
 .UNSPECIFIED. ) ;
#1356 = CARTESIAN_POINT ( 'NONE',  ( 1.845516155340734654, -26.07294027404319792, 6.875780273367530171 ) ) ;
#1357 = APPLICATION_CONTEXT ( 'automotive_design' ) ;
#1358 = ORIENTED_EDGE ( 'NONE', *, *, #8530, .T. ) ;
#1359 = CARTESIAN_POINT ( 'NONE',  ( 66.42000668879826719, 57.79655248154880098, 4.000000000000015987 ) ) ;
#1360 = CARTESIAN_POINT ( 'NONE',  ( 73.23371602657820745, 61.99063567959824184, -3.556895493546552878 ) ) ;
#1361 = VECTOR ( 'NONE', #14321, 1000.000000000000000 ) ;
#1362 = CARTESIAN_POINT ( 'NONE',  ( -64.08758708074093136, 38.13199975834322686, 3.043809435734686097 ) ) ;
#1363 = CARTESIAN_POINT ( 'NONE',  ( 88.01214243333713227, -2.271333487497714465, 2.136702053253976885 ) ) ;
#1364 = ORIENTED_EDGE ( 'NONE', *, *, #15068, .T. ) ;
#1365 = CARTESIAN_POINT ( 'NONE',  ( -72.84815947045233031, 2.429809908903064919, -10.96147798754375202 ) ) ;
#1366 = SHAPE_DEFINITION_REPRESENTATION ( #33255, #27999 ) ;
#1367 = EDGE_CURVE ( 'NONE', #37942, #25139, #13140, .T. ) ;
#1368 = CARTESIAN_POINT ( 'NONE',  ( -29.07867591359219617, -24.55319635012989110, 6.700000000000000178 ) ) ;
#1369 = CARTESIAN_POINT ( 'NONE',  ( -74.92283640148291113, 18.87330372387140187, -46.17089178453873188 ) ) ;
#1370 = CARTESIAN_POINT ( 'NONE',  ( 5.098140652402787687, -29.31764686638471318, 7.505001789837626447 ) ) ;
#1371 = EDGE_CURVE ( 'NONE', #12043, #1373, #9301, .T. ) ;
#1372 = AXIS2_PLACEMENT_3D ( 'NONE', #36269, #39544, #11531 ) ;
#1373 = VERTEX_POINT ( 'NONE', #27276 ) ;
#1374 = CARTESIAN_POINT ( 'NONE',  ( 80.80054865964804378, 61.51733283104052674, -2.392122129321803126 ) ) ;
#1375 = CARTESIAN_POINT ( 'NONE',  ( 37.14216958134459645, -2.489364195891544007, 5.966867749344678451 ) ) ;
#1376 = CARTESIAN_POINT ( 'NONE',  ( 78.96934220494367196, 65.43027598480411200, 2.854164747637875976 ) ) ;
#1377 = DIRECTION ( 'NONE',  ( -0.4690749385695646145, -0.8831583674551010121, -3.445651357372585989E-15 ) ) ;
#1378 = EDGE_CURVE ( 'NONE', #22687, #28211, #22091, .T. ) ;
#1379 = CARTESIAN_POINT ( 'NONE',  ( 24.20516649451111491, 2.665701447796034795, 3.984199654269047652 ) ) ;
#1380 = CARTESIAN_POINT ( 'NONE',  ( 21.05503876034566346, 6.110295703302774051, -3.370870897236230679 ) ) ;
#1381 = CARTESIAN_POINT ( 'NONE',  ( 3.922988059513587089, -26.99698279172644177, 6.894806418505345924 ) ) ;
#1382 = CARTESIAN_POINT ( 'NONE',  ( 33.80124125800227830, -4.917752503226308747, -3.288427953259154268 ) ) ;
#1383 = CARTESIAN_POINT ( 'NONE',  ( 5.200294581628556401, -29.54390383290751387, 7.737115613922530777 ) ) ;
#1384 = AXIS2_PLACEMENT_3D ( 'NONE', #17559, #13890, #30147 ) ;
#1385 = CARTESIAN_POINT ( 'NONE',  ( 14.68923871262327374, -4.581893804377800805, 2.499999999999876543 ) ) ;
#1386 = B_SPLINE_CURVE_WITH_KNOTS ( 'NONE', 3,
 ( #30871, #40309, #7660, #17112, #27556, #32794, #14029, #4772, #186, #40504, #34378, #28793, #25697, #9018, #34178, #31071, #40719, #37622, #35189, #26309, #10836, #19723, #26111, #23413, #38240 ),
 .UNSPECIFIED., .F., .F.,
 ( 4, 3, 3, 3, 3, 3, 3, 3, 4 ),
 ( 6.468151674594278821E-05, 9.076621574722433050E-05, 0.0001210204262068000672, 0.0001512763324577483628, 0.0001815301820994212134, 0.0002117781465860742022, 0.0002420274594459714671, 0.0002722905548971123733, 0.0002816827545175610106 ),
 .UNSPECIFIED. ) ;
#1387 = CARTESIAN_POINT ( 'NONE',  ( -74.54874278403309518, -2.537033486011438299, -9.369704204412682813 ) ) ;
#1388 = CARTESIAN_POINT ( 'NONE',  ( 5.141009602703632275, -28.92794678622675875, 7.678495282201402539 ) ) ;
#1389 = CARTESIAN_POINT ( 'NONE',  ( -22.97867591359219119, -26.64985754041175525, 6.700000000000000178 ) ) ;
#1390 = CARTESIAN_POINT ( 'NONE',  ( 79.37790743583137498, 65.75409067367344562, 2.639511535887585136 ) ) ;
#1391 = CARTESIAN_POINT ( 'NONE',  ( -1.483415766250580470, -30.76298519013761279, 7.721096864323905073 ) ) ;
#1392 = CARTESIAN_POINT ( 'NONE',  ( 3.858201203583684791, -26.94241211265676839, 7.703977250142846955 ) ) ;
#1393 = DIRECTION ( 'NONE',  ( -0.4582725098355734938, 0.8888117386314180468, -0.000000000000000000 ) ) ;
#1394 = CARTESIAN_POINT ( 'NONE',  ( -1.645585159361036220, -30.17362680341680203, 7.635761828346577573 ) ) ;
#1395 = CARTESIAN_POINT ( 'NONE',  ( 4.422352071802834850, -27.36970206379270820, 6.870737987065012042 ) ) ;
#1396 = AXIS2_PLACEMENT_3D ( 'NONE', #31980, #35078, #19006 ) ;
#1397 = CARTESIAN_POINT ( 'NONE',  ( 5.098207581826219581, -29.69173459304409946, 7.754798119455333705 ) ) ;
#1398 = CARTESIAN_POINT ( 'NONE',  ( 4.172240291830656034, -31.90445124331759530, 6.911401339314958925 ) ) ;
#1399 = CARTESIAN_POINT ( 'NONE',  ( 2.493334271959621873, -32.98593869321148730, 7.139344958878412584 ) ) ;
#1400 = CARTESIAN_POINT ( 'NONE',  ( 68.43818535210665743, 59.05932329210152432, 3.950303728398547598 ) ) ;
#1401 = CARTESIAN_POINT ( 'NONE',  ( 35.33522315395951097, -3.172769310824047118, 5.721314177413483471 ) ) ;
#1402 = ORIENTED_EDGE ( 'NONE', *, *, #10684, .T. ) ;
#1403 = CARTESIAN_POINT ( 'NONE',  ( 1.847632973160104664, 12.44248440543094958, 4.000000000000000000 ) ) ;
#1404 = CARTESIAN_POINT ( 'NONE',  ( 85.19300053701067554, 2.612159253720373275, 3.340723803646971302 ) ) ;
#1406 = DIRECTION ( 'NONE',  ( -0.000000000000000000, -0.000000000000000000, 1.000000000000000000 ) ) ;
#1405 = CARTESIAN_POINT ( 'NONE',  ( 78.97731087898851854, 65.91669204587326192, -2.137206601789619409 ) ) ;
#1407 = CARTESIAN_POINT ( 'NONE',  ( -1.265893590836503213, -27.71217119381226368, 6.867199677474202346 ) ) ;
#1408 = CARTESIAN_POINT ( 'NONE',  ( -6.878675913592188884, -26.64985754041175525, 6.800000000000000711 ) ) ;
#1409 = EDGE_LOOP ( 'NONE', ( #16820, #14083, #26242, #14507 ) ) ;
#1410 = VECTOR ( 'NONE', #12265, 1000.000000000000000 ) ;
#1411 = CARTESIAN_POINT ( 'NONE',  ( 4.826899123084856136, -31.15826764627123424, 7.139344958878409919 ) ) ;
#1412 = FACE_OUTER_BOUND ( 'NONE', #24496, .T. ) ;
#1413 = ORIENTED_EDGE ( 'NONE', *, *, #26461, .F. ) ;
#1414 = CARTESIAN_POINT ( 'NONE',  ( -71.78177034180626492, -21.31587262608876543, 5.951446729975963912 ) ) ;
#1415 = CARTESIAN_POINT ( 'NONE',  ( 80.97304215327341126, 61.92799980795002313, -2.787474064117368311 ) ) ;
#1416 = CARTESIAN_POINT ( 'NONE',  ( 25.01091293555841233, 3.329590545877085805, 1.936828124349011526 ) ) ;
#1417 = CARTESIAN_POINT ( 'NONE',  ( 78.88238753611518916, 65.83802744495456238, 2.215902410107951415 ) ) ;
#1418 = CARTESIAN_POINT ( 'NONE',  ( 24.52405562390649152, 0.9766989416590386996, 4.778545449797553246 ) ) ;
#1419 = ORIENTED_EDGE ( 'NONE', *, *, #7107, .T. ) ;
#1420 = EDGE_CURVE ( 'NONE', #637, #12025, #9690, .T. ) ;
#1421 = EDGE_CURVE ( 'NONE', #24859, #27482, #2904, .T. ) ;
#1422 = AXIS2_PLACEMENT_3D ( 'NONE', #5373, #27190, #39748 ) ;
#1424 = ADVANCED_FACE ( 'NONE', ( #18777 ), #31557, .F. ) ;
#1423 = CARTESIAN_POINT ( 'NONE',  ( 5.038442556635803982, -30.21599964681902506, 6.887041543973312585 ) ) ;
#1426 = CARTESIAN_POINT ( 'NONE',  ( -8.400069747914319152, -0.9236158798217076749, 2.500000000000000000 ) ) ;
#1425 = FACE_OUTER_BOUND ( 'NONE', #26472, .T. ) ;
#1427 = CARTESIAN_POINT ( 'NONE',  ( -20.87867591359218977, -24.55319635012989110, 6.700000000000000178 ) ) ;
#1428 = CARTESIAN_POINT ( 'NONE',  ( -63.55798368792363107, 43.57337240874115736, -2.980826430635752367 ) ) ;
#1429 = CARTESIAN_POINT ( 'NONE',  ( 22.67711167293747465, 4.399063442879564079, -3.239999287829872010 ) ) ;
#1430 = ORIENTED_EDGE ( 'NONE', *, *, #39262, .F. ) ;
#1431 = CARTESIAN_POINT ( 'NONE',  ( -71.19092636660957396, 0.1906808711754918728, 5.995465708869196497 ) ) ;
#1432 = CARTESIAN_POINT ( 'NONE',  ( 21.85643539959776049, -3.145688729744653411, 12.47482453294728266 ) ) ;
#1433 = CARTESIAN_POINT ( 'NONE',  ( 21.38787910472312959, 9.379444465854763990, -3.308503362029312722 ) ) ;
#1434 = CARTESIAN_POINT ( 'NONE',  ( 16.10543310223363989, 10.11511964520479623, 2.500000000000331291 ) ) ;
#1435 = CYLINDRICAL_SURFACE ( 'NONE', #15585, 0.1000000000000028644 ) ;
#1436 = CARTESIAN_POINT ( 'NONE',  ( 81.48104477344870133, 62.99720032632000510, 3.089171411838275372 ) ) ;
#1437 = CARTESIAN_POINT ( 'NONE',  ( 88.82472656415403378, -2.095778867207653828, 0.2190179053162402134 ) ) ;
#1438 = CARTESIAN_POINT ( 'NONE',  ( -0.5120772278873689798, -26.98826626735417378, 7.680992449362115337 ) ) ;
#1439 = ORIENTED_EDGE ( 'NONE', *, *, #10916, .F. ) ;
#1440 = CARTESIAN_POINT ( 'NONE',  ( -77.48844425012140391, -4.890808455674215516, 9.140760539542357677 ) ) ;
#1441 = CARTESIAN_POINT ( 'NONE',  ( 1.578585683582427235, -32.96774767198657941, 7.754798119455333705 ) ) ;
#1442 = CARTESIAN_POINT ( 'NONE',  ( 1.145429890469515932, -32.92433313672930240, 7.695279973900954751 ) ) ;
#1443 = CARTESIAN_POINT ( 'NONE',  ( 18.21410597459779979, -2.881839143183631879, -3.049149765790359012 ) ) ;
#1444 = CARTESIAN_POINT ( 'NONE',  ( 20.42278620884589202, 3.662520991485072042, -3.393867733478101112 ) ) ;
#1445 = CYLINDRICAL_SURFACE ( 'NONE', #14804, 0.1000000000000028644 ) ;
#1446 = CARTESIAN_POINT ( 'NONE',  ( -0.1040043641139408170, -32.45162424111279620, 7.754798119455333705 ) ) ;
#1447 = DIRECTION ( 'NONE',  ( -0.2567910337120311026, 0.7055275666422143876, -0.6605219282605403475 ) ) ;
#1448 = DIRECTION ( 'NONE',  ( 0.000000000000000000, 0.000000000000000000, 1.000000000000000000 ) ) ;
#1449 = VECTOR ( 'NONE', #20329, 1000.000000000000114 ) ;
#1450 = CARTESIAN_POINT ( 'NONE',  ( 31.91123179551076561, -2.970386030880023398, -5.186917516383627635 ) ) ;
#1451 = ORIENTED_EDGE ( 'NONE', *, *, #23533, .F. ) ;
#1452 = ORIENTED_EDGE ( 'NONE', *, *, #25717, .T. ) ;
#1453 = CARTESIAN_POINT ( 'NONE',  ( 36.20098261264391226, -3.650343263429455476, 5.718100817311416506 ) ) ;
#1454 = CARTESIAN_POINT ( 'NONE',  ( -1.649286765102148777, -30.58465425659426629, 6.951256099901588215 ) ) ;
#1455 = CARTESIAN_POINT ( 'NONE',  ( 66.27376694609004915, 57.73522568913436004, -4.000000000000000000 ) ) ;
#1456 = CARTESIAN_POINT ( 'NONE',  ( -4.248748702180636272, -26.64985754041175525, 6.700000000000000178 ) ) ;
#1457 = EDGE_LOOP ( 'NONE', ( #39718, #28497, #15279, #32228 ) ) ;
#1458 = ORIENTED_EDGE ( 'NONE', *, *, #11982, .T. ) ;
#1459 = DIRECTION ( 'NONE',  ( 0.4999999999999979461, 0.8660254037844397068, -0.000000000000000000 ) ) ;
#1460 =( NAMED_UNIT ( * ) SI_UNIT ( $, .STERADIAN. ) SOLID_ANGLE_UNIT ( ) );
#1461 = CARTESIAN_POINT ( 'NONE',  ( -16.44874870218064089, -26.64985754041175525, 6.700000000000000178 ) ) ;
#1463 = CYLINDRICAL_SURFACE ( 'NONE', #28929, 6.000000000000002665 ) ;
#1462 = CARTESIAN_POINT ( 'NONE',  ( 4.820161459608385712, -27.98341619935644076, 6.921725064902950919 ) ) ;
#1464 = ORIENTED_EDGE ( 'NONE', *, *, #37587, .F. ) ;
#1465 = CARTESIAN_POINT ( 'NONE',  ( 22.55238216757502556, 4.103974954327002322, 3.630433831594339633 ) ) ;
#1466 = CARTESIAN_POINT ( 'NONE',  ( 82.11700085695680684, 62.19713100941778805, -1.465650077276901886 ) ) ;
#1468 = EDGE_CURVE ( 'NONE', #11412, #35457, #22361, .T. ) ;
#1467 = CARTESIAN_POINT ( 'NONE',  ( -1.312937918266134707, -31.35033874361411321, 7.710604733652628440 ) ) ;
#1469 = ORIENTED_EDGE ( 'NONE', *, *, #38773, .T. ) ;
#1471 = FACE_OUTER_BOUND ( 'NONE', #6124, .T. ) ;
#1470 = DIRECTION ( 'NONE',  ( 0.000000000000000000, 0.000000000000000000, 1.000000000000000000 ) ) ;
#1472 = FACE_OUTER_BOUND ( 'NONE', #14916, .T. ) ;
#1473 = CARTESIAN_POINT ( 'NONE',  ( 75.50377651103727317, 61.49872921062497255, 3.901127667181019110 ) ) ;
#1474 = CARTESIAN_POINT ( 'NONE',  ( 22.67441447122924103, 2.915876502080354093, -4.452506167857361419 ) ) ;
#1475 = DIRECTION ( 'NONE',  ( -0.000000000000000000, -0.000000000000000000, -1.000000000000000000 ) ) ;
#1476 = DIRECTION ( 'NONE',  ( 1.000000000000000000, 1.486905836551549118E-14, 0.000000000000000000 ) ) ;
#1477 = CARTESIAN_POINT ( 'NONE',  ( -14.44874870218064089, -25.49307895267003587, 6.800000000000000711 ) ) ;
#1478 = CARTESIAN_POINT ( 'NONE',  ( 1.751251297819361730, -26.64985754041175525, 6.700000000000000178 ) ) ;
#1479 = CARTESIAN_POINT ( 'NONE',  ( -1.057258846844102873, -31.72486802769777725, 7.754798119455333705 ) ) ;
#1480 = CARTESIAN_POINT ( 'NONE',  ( 80.57628295459070955, 65.85481838934502719, 2.430878896394115696 ) ) ;
#1481 = CARTESIAN_POINT ( 'NONE',  ( 85.82060591106392167, 1.959946745720340777, 4.199140470389015611 ) ) ;
#1482 = CARTESIAN_POINT ( 'NONE',  ( 33.33276309746427302, -3.557760156652166383, 5.357383698657358195 ) ) ;
#1483 = PLANE ( 'NONE',  #5669 ) ;
#1484 = CARTESIAN_POINT ( 'NONE',  ( -71.32207927536605041, -45.65648572842182062, 9.993882909048494412 ) ) ;
#1485 = AXIS2_PLACEMENT_3D ( 'NONE', #33810, #5590, #30721 ) ;
#1486 = CARTESIAN_POINT ( 'NONE',  ( -74.48011309984730133, -2.455786751632346832, -10.65291168091849805 ) ) ;
#1487 = CARTESIAN_POINT ( 'NONE',  ( -70.95330471031414277, 33.71485196875532608, 8.800414904976364028 ) ) ;
#1488 = CARTESIAN_POINT ( 'NONE',  ( 0.06942149629988161874, -26.47315344242070267, 6.870724624169668893 ) ) ;
#1489 = CARTESIAN_POINT ( 'NONE',  ( 36.79817360360340928, -3.072032592432972553, -5.949642976670753036 ) ) ;
#1490 = VECTOR ( 'NONE', #40411, 1000.000000000000000 ) ;
#1491 = CARTESIAN_POINT ( 'NONE',  ( 1.099000663213878015, -32.91633116162691408, 7.775108481317161591 ) ) ;
#1492 = CARTESIAN_POINT ( 'NONE',  ( 1.700390093233090871, -29.56993018339339940, 6.850000000000000533 ) ) ;
#1493 = CARTESIAN_POINT ( 'NONE',  ( -63.70768058868310391, 44.39675795731060504, -1.424602271588051527 ) ) ;
#1494 = EDGE_CURVE ( 'NONE', #25777, #31697, #32744, .T. ) ;
#1495 = CARTESIAN_POINT ( 'NONE',  ( -70.92837670882107659, 28.72470171467712063, 0.000000000000000000 ) ) ;
#1496 = CARTESIAN_POINT ( 'NONE',  ( -1.799609906766908685, -29.56993018339339940, 6.850000000000000533 ) ) ;
#1497 = ORIENTED_EDGE ( 'NONE', *, *, #13901, .F. ) ;
#1498 = CARTESIAN_POINT ( 'NONE',  ( 35.34387176057341406, -3.571392527219161561, 5.666785202510572717 ) ) ;
#1499 = CARTESIAN_POINT ( 'NONE',  ( 5.015318072754217482, -33.54151383920058294, 7.635761828346577573 ) ) ;
#1500 = CARTESIAN_POINT ( 'NONE',  ( 67.09515986712425217, 58.21407947277521089, -3.993497817183391696 ) ) ;
#1501 = CARTESIAN_POINT ( 'NONE',  ( -1.346804739101824966, -27.84812774008250003, 7.670465701733752972 ) ) ;
#1502 = ADVANCED_FACE ( 'NONE', ( #24970 ), #34457, .T. ) ;
#1503 = EDGE_LOOP ( 'NONE', ( #28736, #3473, #31108, #47 ) ) ;
#1504 = CARTESIAN_POINT ( 'NONE',  ( 0.9053063435450576790, -25.37262878166647084, 7.695279973900954751 ) ) ;
#1505 = CARTESIAN_POINT ( 'NONE',  ( 3.883672655497297121, -32.17632179888655486, 7.769368695748489095 ) ) ;
#1506 = CARTESIAN_POINT ( 'NONE',  ( 85.38064914651351955, 1.325933486174632359, -5.556288812255563592 ) ) ;
#1507 = CARTESIAN_POINT ( 'NONE',  ( 5.050166971101031521, -28.55553628183517034, 6.961115707816237119 ) ) ;
#1508 = DIRECTION ( 'NONE',  ( 0.01395351027862084224, -0.9999026450364577601, 0.000000000000000000 ) ) ;
#1509 = VECTOR ( 'NONE', #23962, 1000.000000000000000 ) ;
#1510 = CARTESIAN_POINT ( 'NONE',  ( 1.267242271181500568, -26.09682929696383269, 6.903112506833892326 ) ) ;
#1511 = VERTEX_POINT ( 'NONE', #22897 ) ;
#1512 = CARTESIAN_POINT ( 'NONE',  ( 23.74299019415878220, 3.560518783519561303, 3.187235075460781442 ) ) ;
#1513 = SURFACE_STYLE_FILL_AREA ( #3418 ) ;
#1514 = CARTESIAN_POINT ( 'NONE',  ( 81.12411360294466078, 61.28734817074503383, 1.205449537698832563 ) ) ;
#1516 = EDGE_CURVE ( 'NONE', #22380, #20746, #23495, .T. ) ;
#1515 = CARTESIAN_POINT ( 'NONE',  ( -63.16614402916191295, 41.45853387640750753, 4.000000000000003553 ) ) ;
#1517 = ORIENTED_EDGE ( 'NONE', *, *, #33017, .T. ) ;
#1518 = CARTESIAN_POINT ( 'NONE',  ( 79.68931684371919744, 62.31783030446535321, -3.554489553981595051 ) ) ;
#1520 = CARTESIAN_POINT ( 'NONE',  ( -0.6429675508017466123, -32.04310423402981201, 7.386948897581452123 ) ) ;
#1519 = CARTESIAN_POINT ( 'NONE',  ( 26.02524177375569181, 0.8359984680724493744, 4.424135539687619634 ) ) ;
#1521 = CARTESIAN_POINT ( 'NONE',  ( 81.64001200211806974, 62.74592715520643793, -2.852119850606562590 ) ) ;
#1522 = CARTESIAN_POINT ( 'NONE',  ( 78.56694041390316841, 64.50177951359142980, 3.424416364708430027 ) ) ;
#1523 = CARTESIAN_POINT ( 'NONE',  ( -0.9161852239640245754, -27.39886279396606739, 7.748216051605112398 ) ) ;
#1524 = CARTESIAN_POINT ( 'NONE',  ( 81.32357852907315987, 65.91643957835155732, 1.421283058690022916 ) ) ;
#1525 = CARTESIAN_POINT ( 'NONE',  ( -70.92837670882107659, -56.35932253828836025, 0.000000000000000000 ) ) ;
#1526 = CARTESIAN_POINT ( 'NONE',  ( 28.77170544830297416, -1.679059579700503901, 5.945470488877720783 ) ) ;
#1527 = CARTESIAN_POINT ( 'NONE',  ( -64.72110749213814529, 34.74377494905899511, -6.240054254828758751 ) ) ;
#1528 = ORIENTED_EDGE ( 'NONE', *, *, #12883, .F. ) ;
#1529 = AXIS2_PLACEMENT_3D ( 'NONE', #27491, #14703, #26872 ) ;
#1530 = CARTESIAN_POINT ( 'NONE',  ( -78.62674788310239649, -5.321002937650163744, 8.138356128977308757 ) ) ;
#1531 = CARTESIAN_POINT ( 'NONE',  ( 24.12311362605193210, 0.4935845079932565382, -5.095120067356918803 ) ) ;
#1532 = EDGE_CURVE ( 'NONE', #34807, #36832, #20388, .T. ) ;
#1533 = B_SPLINE_CURVE_WITH_KNOTS ( 'NONE', 3,
 ( #20835, #8882, #2747, #15270, #5200, #37095, #28034, #27218, #37297, #6017, #27821, #36493, #9094, #8472, #24538, #5610, #18149, #21464, #5813, #40579, #14646, #17731, #18354, #23917, #11553, #21668, #18553, #12179, #8263, #34246, #21055 ),
 .UNSPECIFIED., .F., .F.,
 ( 4, 3, 3, 3, 3, 3, 3, 3, 3, 3, 4 ),
 ( 9.171767249593720258E-19, 2.999644130998047059E-05, 6.002588995695312495E-05, 8.960886084588529804E-05, 0.0001190604700446542971, 0.0001489538463052789846, 0.0001796139255494059864, 0.0002109707048517130417, 0.0002426195318110442199, 0.0002740640997890140445, 0.0002849778069099921174 ),
 .UNSPECIFIED. ) ;
#1534 = DIRECTION ( 'NONE',  ( -0.000000000000000000, -0.000000000000000000, -1.000000000000000000 ) ) ;
#1535 = ORIENTED_EDGE ( 'NONE', *, *, #18438, .F. ) ;
#1536 = CARTESIAN_POINT ( 'NONE',  ( 33.67912868440872387, -3.778924337320058502, -5.203600794767529791 ) ) ;
#1537 = SURFACE_STYLE_USAGE ( .BOTH. , #32637 ) ;
#1538 = CARTESIAN_POINT ( 'NONE',  ( 3.323202191371804393, -32.67097531272231947, 6.875780273367528395 ) ) ;
#1539 = CARTESIAN_POINT ( 'NONE',  ( -1.100427372579028340, -31.66883981513531054, 6.961115707816243336 ) ) ;
#1540 = CARTESIAN_POINT ( 'NONE',  ( 0.000000000000000000, 0.000000000000000000, 2.500000000000000000 ) ) ;
#1541 = CARTESIAN_POINT ( 'NONE',  ( 2.691619168861421052, -32.82224166115583586, 6.887945620086118659 ) ) ;
#1542 = DIRECTION ( 'NONE',  ( 1.000000000000000000, -0.000000000000000000, 0.000000000000000000 ) ) ;
#1543 = B_SPLINE_CURVE_WITH_KNOTS ( 'NONE', 3,
 ( #23430, #35995, #27318, #8159, #7776, #4889, #39878, #23812, #30209, #11655, #1614, #1823, #32906, #2026, #14345, #11247, #36387, #20731, #33316, #28552, #34762, #40690, #18457, #30839, #37596, #12495, #9605, #15583, #40279, #21769, #11860 ),
 .UNSPECIFIED., .F., .F.,
 ( 4, 3, 3, 3, 3, 3, 3, 3, 3, 3, 4 ),
 ( 1.852685484479510593E-18, 2.999644130997725525E-05, 6.002588995694735157E-05, 8.960886084588132715E-05, 0.0001190604700446500145, 0.0001489538463052724794, 0.0001796139255493986139, 0.0002109707048517102228, 0.0002426195318110376876, 0.0002740640997890085692, 0.0002849778069099863169 ),
 .UNSPECIFIED. ) ;
#1544 = CYLINDRICAL_SURFACE ( 'NONE', #1384, 0.09010775117053103356 ) ;
#1545 = ORIENTED_EDGE ( 'NONE', *, *, #25757, .F. ) ;
#1546 = ADVANCED_FACE ( 'NONE', ( #35270 ), #19994, .F. ) ;
#1547 = VERTEX_POINT ( 'NONE', #1477 ) ;
#1549 = ADVANCED_FACE ( 'NONE', ( #16893 ), #29473, .F. ) ;
#1548 = CARTESIAN_POINT ( 'NONE',  ( 66.42693215277247987, 57.77698748017490971, 4.000000000000009770 ) ) ;
#1550 = CARTESIAN_POINT ( 'NONE',  ( 72.21306447944246543, 59.67152943164661849, -3.942504219364093121 ) ) ;
#1551 = EDGE_CURVE ( 'NONE', #5954, #20746, #16300, .T. ) ;
#1552 = EDGE_LOOP ( 'NONE', ( #32484, #9373, #40170, #13436 ) ) ;
#1553 = CARTESIAN_POINT ( 'NONE',  ( 88.05006142693602555, -2.316660831613085225, -1.868938639203592489 ) ) ;
#1554 = FACE_OUTER_BOUND ( 'NONE', #12637, .T. ) ;
#1555 = LINE ( 'NONE', #1760, #19571 ) ;
#1556 = CARTESIAN_POINT ( 'NONE',  ( 0.000000000000000000, 0.000000000000000000, 0.000000000000000000 ) ) ;
#1557 = CARTESIAN_POINT ( 'NONE',  ( 2.296140040222784950, -32.91733974362343673, 7.763628509615286610 ) ) ;
#1558 = CARTESIAN_POINT ( 'NONE',  ( -42.83131703149249603, -27.06993018339339585, 6.800000000000000711 ) ) ;
#1559 = CARTESIAN_POINT ( 'NONE',  ( 25.11437021580303863, 164.7550792202006562, -1.000000000000000000 ) ) ;
#1560 = DIRECTION ( 'NONE',  ( 1.000000000000000000, 0.000000000000000000, 0.000000000000000000 ) ) ;
#1561 = ORIENTED_EDGE ( 'NONE', *, *, #9680, .F. ) ;
#1562 = EDGE_CURVE ( 'NONE', #16241, #1778, #14544, .T. ) ;
#1563 = ORIENTED_EDGE ( 'NONE', *, *, #10637, .F. ) ;
#1564 = CARTESIAN_POINT ( 'NONE',  ( 79.54992950373222982, 64.18601594420306355, -3.671038198312436496 ) ) ;
#1565 =( BOUNDED_CURVE ( )  B_SPLINE_CURVE ( 3, ( #2291, #14607, #30485, #27179 ),
 .UNSPECIFIED., .F., .T. ) 
 B_SPLINE_CURVE_WITH_KNOTS ( ( 4, 4 ),
 ( 4.708531083176467291, 4.895802057644188743 ),
 .UNSPECIFIED. ) 
 CURVE ( )  GEOMETRIC_REPRESENTATION_ITEM ( )  RATIONAL_B_SPLINE_CURVE ( ( 1.000000000000000000, 0.9970795998553221295, 0.9970795998553221295, 1.000000000000000000 ) ) 
 REPRESENTATION_ITEM ( '' )  );
#1566 = CARTESIAN_POINT ( 'NONE',  ( 13.80252864702349314, 11.14042148585687109, -2.500000000000005773 ) ) ;
#1567 = CARTESIAN_POINT ( 'NONE',  ( 78.51047153333163919, 65.93088068117918965, 1.448968528257593258 ) ) ;
#1568 = DIRECTION ( 'NONE',  ( -0.000000000000000000, 1.000000000000000000, -0.000000000000000000 ) ) ;
#1569 = CARTESIAN_POINT ( 'NONE',  ( -40.34874870218063592, -26.64985754041175525, 6.700000000000000178 ) ) ;
#1570 = CARTESIAN_POINT ( 'NONE',  ( 14.97038224746134816, 12.32935407697701358, -2.523898521188913335 ) ) ;
#1571 = CARTESIAN_POINT ( 'NONE',  ( 17.34825500165157308, 14.28608438251766444, 2.500000000000000444 ) ) ;
#1572 = CARTESIAN_POINT ( 'NONE',  ( 21.85643539959779247, -13.31640034840845388, 0.8419676367911695936 ) ) ;
#1573 = CARTESIAN_POINT ( 'NONE',  ( 1.700390093233090871, -29.56993018339339940, 7.800000000000000711 ) ) ;
#1574 = EDGE_LOOP ( 'NONE', ( #33274, #14393, #25939, #14553 ) ) ;
#1575 = CARTESIAN_POINT ( 'NONE',  ( 76.46955312333206223, 64.49609874770474960, -2.565500891477647816 ) ) ;
#1576 = EDGE_CURVE ( 'NONE', #32349, #32411, #25781, .T. ) ;
#1577 = CARTESIAN_POINT ( 'NONE',  ( 14.76025685109631169, -5.148805109997777407, 2.500008232146889942 ) ) ;
#1578 = VECTOR ( 'NONE', #27868, 1000.000000000000000 ) ;
#1579 = CARTESIAN_POINT ( 'NONE',  ( -76.52714247067879683, -4.348968750379587078, -9.772157169844637892 ) ) ;
#1580 = DIRECTION ( 'NONE',  ( -0.3420201433256706003, 0.9396926207859077618, 0.000000000000000000 ) ) ;
#1581 = CARTESIAN_POINT ( 'NONE',  ( 33.68523101384537455, -3.842693762900835530, -5.135094833158061256 ) ) ;
#1582 = CARTESIAN_POINT ( 'NONE',  ( 80.54433603269386310, 64.00140174820366212, 3.588566286536281957 ) ) ;
#1583 = LINE ( 'NONE', #1197, #20933 ) ;
#1584 = DIRECTION ( 'NONE',  ( 0.8660254037844380415, 0.5000000000000009992, -0.000000000000000000 ) ) ;
#1585 = CARTESIAN_POINT ( 'NONE',  ( -1.642727701737825896, -30.18925514571027335, 7.661510568013096822 ) ) ;
#1586 = CARTESIAN_POINT ( 'NONE',  ( 0.6319492117650733487, -26.23698571484616693, 6.870724624169667116 ) ) ;
#1587 = ADVANCED_FACE ( 'NONE', ( #32776 ), #35863, .T. ) ;
#1588 = AXIS2_PLACEMENT_3D ( 'NONE', #33095, #29997, #36380 ) ;
#1589 = CARTESIAN_POINT ( 'NONE',  ( 4.497269860293852339, -27.46577629914297702, 6.921725064902955360 ) ) ;
#1590 = EDGE_CURVE ( 'NONE', #33368, #22465, #31032, .T. ) ;
#1591 = CARTESIAN_POINT ( 'NONE',  ( 87.02342806255605012, 0.6088798157811630141, 4.904800718280144523 ) ) ;
#1592 = CARTESIAN_POINT ( 'NONE',  ( 4.176219800253964998, -31.90023320913972782, 7.006423389747793884 ) ) ;
#1593 = AXIS2_PLACEMENT_3D ( 'NONE', #1881, #39938, #8632 ) ;
#1594 = DIRECTION ( 'NONE',  ( -0.000000000000000000, -0.000000000000000000, -1.000000000000000000 ) ) ;
#1595 = CARTESIAN_POINT ( 'NONE',  ( 67.63028434841179148, 58.56128740577801750, 3.979762160777183588 ) ) ;
#1596 = CARTESIAN_POINT ( 'NONE',  ( 36.14178000185388839, -3.145485669043203814, 5.847196880178433531 ) ) ;
#1597 = EDGE_CURVE ( 'NONE', #40141, #14437, #22702, .T. ) ;
#1598 = DIRECTION ( 'NONE',  ( -0.000000000000000000, -0.000000000000000000, -1.000000000000000000 ) ) ;
#1599 = CARTESIAN_POINT ( 'NONE',  ( 87.65094362820954643, -0.09597545124639318692, -4.742286025697146634 ) ) ;
#1601 = CARTESIAN_POINT ( 'NONE',  ( -0.4841935375551393306, -26.83541114705590758, 6.865554069792297653 ) ) ;
#1600 = CARTESIAN_POINT ( 'NONE',  ( 80.95271419388603817, 62.75148163162413795, -3.324099845469154602 ) ) ;
#1602 = CARTESIAN_POINT ( 'NONE',  ( 4.365277478145313417, -27.30091955980304874, 7.651421919295146701 ) ) ;
#1603 = ORIENTED_EDGE ( 'NONE', *, *, #23697, .T. ) ;
#1604 = CARTESIAN_POINT ( 'NONE',  ( 1.076698322469717750, -26.22039822960329403, 7.257242401810562349 ) ) ;
#1605 = DIRECTION ( 'NONE',  ( 0.000000000000000000, 0.000000000000000000, 1.000000000000000000 ) ) ;
#1606 = ORIENTED_EDGE ( 'NONE', *, *, #8051, .T. ) ;
#1607 = CARTESIAN_POINT ( 'NONE',  ( -71.92837670882107659, -20.78299143688747819, 5.928123921495630277 ) ) ;
#1608 = AXIS2_PLACEMENT_3D ( 'NONE', #15904, #35622, #3386 ) ;
#1609 = EDGE_LOOP ( 'NONE', ( #12170, #36601, #32369, #22372 ) ) ;
#1610 = CARTESIAN_POINT ( 'NONE',  ( 79.84444348018388382, 64.37461814510197655, -3.624000857162082312 ) ) ;
#1611 = DIRECTION ( 'NONE',  ( 0.000000000000000000, 1.000000000000000000, 0.000000000000000000 ) ) ;
#1612 = CARTESIAN_POINT ( 'NONE',  ( 81.08254763934547782, 61.27217476014467934, 1.284346554836957255 ) ) ;
#1613 = CARTESIAN_POINT ( 'NONE',  ( 22.45543544006284620, 0.4771679794038178879, 6.706977661937824742 ) ) ;
#1615 = EDGE_LOOP ( 'NONE', ( #22756, #962 ) ) ;
#1614 = CARTESIAN_POINT ( 'NONE',  ( -0.7684451854189515707, -27.23222622129974724, 6.920489980334480151 ) ) ;
#1616 = AXIS2_PLACEMENT_3D ( 'NONE', #28205, #37666, #37 ) ;
#1617 = CARTESIAN_POINT ( 'NONE',  ( -0.1022282953655194032, -32.45273633994818141, 7.757178535559533294 ) ) ;
#1619 = CARTESIAN_POINT ( 'NONE',  ( -70.92837670882107659, 28.72470171467712063, -4.406751979251624540 ) ) ;
#1618 = CARTESIAN_POINT ( 'NONE',  ( 0.1825688514504736626, 0.5999999999999995337, -3.931742364880508767 ) ) ;
#1620 = LINE ( 'NONE', #14155, #11937 ) ;
#1621 = CARTESIAN_POINT ( 'NONE',  ( 4.659461314909612462, -31.24441443385555672, 7.661510568013094158 ) ) ;
#1622 = CARTESIAN_POINT ( 'NONE',  ( 21.90044900377229098, 5.537031193749818669, -3.318543414941498515 ) ) ;
#1623 = ORIENTED_EDGE ( 'NONE', *, *, #25818, .F. ) ;
#1624 = CARTESIAN_POINT ( 'NONE',  ( 5.128111633932078917, -30.21023550748081377, 7.783750581861600182 ) ) ;
#1625 = ADVANCED_FACE ( 'NONE', ( #36450 ), #39738, .F. ) ;
#1626 = CARTESIAN_POINT ( 'NONE',  ( 22.39040353993711108, 2.683735211801196563, -8.168217153243197970 ) ) ;
#1627 = CARTESIAN_POINT ( 'NONE',  ( 16.55058170395099637, 7.675961124049503148, 3.484773800359490359 ) ) ;
#1628 = CARTESIAN_POINT ( 'NONE',  ( 0.3430422367937097095, -32.68723900743627553, 6.939395833800439561 ) ) ;
#1629 = CARTESIAN_POINT ( 'NONE',  ( 79.86705713781546478, 65.75210810415633489, 2.684801069578925947 ) ) ;
#1630 = CARTESIAN_POINT ( 'NONE',  ( 87.30391260081773908, -0.2898811470106905652, 5.673122884556256906 ) ) ;
#1631 = DIRECTION ( 'NONE',  ( 0.000000000000000000, -0.000000000000000000, -1.000000000000000000 ) ) ;
#1632 = ORIENTED_EDGE ( 'NONE', *, *, #32386, .F. ) ;
#1633 = CARTESIAN_POINT ( 'NONE',  ( -66.99872204295122913, 28.48507918597134037, 9.800414904976365804 ) ) ;
#1634 = VERTEX_POINT ( 'NONE', #39327 ) ;
#1635 = VECTOR ( 'NONE', #32985, 1000.000000000000000 ) ;
#1636 = CIRCLE ( 'NONE', #21354, 10.00000000000000533 ) ;
#1637 = CARTESIAN_POINT ( 'NONE',  ( 4.634605404468733703, -27.83824422985297531, 7.257242401810564125 ) ) ;
#1638 = CARTESIAN_POINT ( 'NONE',  ( 31.37357152309853348, -3.143197726502084954, -5.103002627509826361 ) ) ;
#1639 = CARTESIAN_POINT ( 'NONE',  ( 35.33510904524467833, -3.167696954624281691, -5.721296367988784048 ) ) ;
#1640 = CARTESIAN_POINT ( 'NONE',  ( -17.27251170661583402, 3.729367930467589076, -6.000000000000000000 ) ) ;
#1641 = B_SPLINE_CURVE_WITH_KNOTS ( 'NONE', 3,
 ( #33052, #20678, #1766, #10796, #33260, #39207, #39617, #5660, #30373, #17786, #24807, #14914, #2599, #11805, #12015, #13247, #10150, #31796, #35303, #15527, #21920, #18817, #3216, #12639, #16933, #29702, #20425, #23721, #1320, #19836, #29108, #22938, #4202, #27419 ),
 .UNSPECIFIED., .F., .F.,
 ( 4, 2, 2, 1, 1, 1, 1, 1, 1, 2, 2, 2, 2, 1, 1, 1, 1, 1, 1, 2, 2, 2, 4 ),
 ( 0.000000000000000000, 0.2499999999999977796, 0.3749999999999966693, 0.4374999999999957812, 0.4687499999999956701, 0.4843749999999956701, 0.4921874999999956146, 0.4960937499999956146, 0.4980468749999955591, 0.4990234374999951705, 0.4999999999999947820, 0.6249999999999529265, 0.6874999999999320544, 0.7187499999999212852, 0.7343749999999154010, 0.7421874999999126254, 0.7460937499999110711, 0.7480468749999104050, 0.7490234374999100719, 0.7495117187499102940, 0.7499999999999105160, 0.8749999999999553690, 1.000000000000000000 ),
 .UNSPECIFIED. ) ;
#1642 = CARTESIAN_POINT ( 'NONE',  ( 21.81791346015125654, 0.2734699911238404058, -8.212990486451831273 ) ) ;
#1643 = CYLINDRICAL_SURFACE ( 'NONE', #6437, 6.406751979251626317 ) ;
#1644 = ORIENTED_EDGE ( 'NONE', *, *, #31991, .T. ) ;
#1645 = CARTESIAN_POINT ( 'NONE',  ( 36.42057415831622080, -3.112379919131356143, 5.890709450956581605 ) ) ;
#1646 = ADVANCED_FACE ( 'NONE', ( #4754 ), #33787, .T. ) ;
#1647 = CIRCLE ( 'NONE', #8849, 2.500000000000000000 ) ;
#1648 = CARTESIAN_POINT ( 'NONE',  ( -10.97867591359219475, -26.64985754041175525, 6.800000000000000711 ) ) ;
#1649 = EDGE_CURVE ( 'NONE', #31697, #33979, #39393, .T. ) ;
#1650 = CARTESIAN_POINT ( 'NONE',  ( 4.992773418886902626, -28.42625648742630773, 7.785344483711591934 ) ) ;
#1651 = ORIENTED_EDGE ( 'NONE', *, *, #17090, .F. ) ;
#1652 = VERTEX_POINT ( 'NONE', #8029 ) ;
#1653 = CARTESIAN_POINT ( 'NONE',  ( 37.10978108531639919, -2.403808732534971515, 5.951661781935858819 ) ) ;
#1654 = CARTESIAN_POINT ( 'NONE',  ( -1.642705848810893210, -30.60612974056809676, 6.895394898881666457 ) ) ;
#1655 = CARTESIAN_POINT ( 'NONE',  ( 66.27376694609004915, 57.73522568913436004, -4.000000000000000000 ) ) ;
#1656 = CARTESIAN_POINT ( 'NONE',  ( 86.49500509992682851, -0.6166496396440827032, 5.723172357827475132 ) ) ;
#1657 = ORIENTED_EDGE ( 'NONE', *, *, #38294, .F. ) ;
#1658 = ORIENTED_EDGE ( 'NONE', *, *, #14390, .F. ) ;
#1659 = CARTESIAN_POINT ( 'NONE',  ( 3.070800210251708684, -33.66578602384694108, 6.894806418505347700 ) ) ;
#1660 = SHAPE_REPRESENTATION_RELATIONSHIP ( 'NONE' , 'NONE' ,  #29798, #21016 ) ;
#1661 = B_SPLINE_CURVE_WITH_KNOTS ( 'NONE', 3,
 ( #18220, #12034, #5678, #9164, #15136, #8953, #12251, #24823, #6090, #18623, #38179, #29133, #28313, #38375, #22561, #31414, #16163, #9782, #37768, #25637, #6707, #34518, #10177, #9362, #19255, #21946, #7101, #19664, #3241, #9982, #22766 ),
 .UNSPECIFIED., .F., .F.,
 ( 4, 3, 3, 3, 3, 3, 3, 3, 3, 3, 4 ),
 ( 9.697399036122160616E-19, 2.999644130997348087E-05, 6.002588995694365173E-05, 8.960886084587883348E-05, 0.0001190604700446476428, 0.0001489538463052722083, 0.0001796139255493953341, 0.0002109707048517089488, 0.0002426195318110391512, 0.0002740640997890091655, 0.0002849778069099856122 ),
 .UNSPECIFIED. ) ;
#1662 = VERTEX_POINT ( 'NONE', #21427 ) ;
#1663 = DIRECTION ( 'NONE',  ( 0.000000000000000000, -0.000000000000000000, -1.000000000000000000 ) ) ;
#1665 = CARTESIAN_POINT ( 'NONE',  ( 4.296671084470158775, -27.37462607708720341, 7.756377446753165650 ) ) ;
#1664 = SURFACE_STYLE_FILL_AREA ( #4740 ) ;
#1666 = VERTEX_POINT ( 'NONE', #17903 ) ;
#1667 = CARTESIAN_POINT ( 'NONE',  ( 22.94147134705455926, 4.030654817714214744, 3.371037374912960960 ) ) ;
#1668 = CARTESIAN_POINT ( 'NONE',  ( 81.32635356316018260, 65.55379304840796806, -2.259066313178065943 ) ) ;
#1669 = AXIS2_PLACEMENT_3D ( 'NONE', #7800, #8398, #33552 ) ;
#1670 = VECTOR ( 'NONE', #17832, 1000.000000000000000 ) ;
#1671 = CARTESIAN_POINT ( 'NONE',  ( 1.700390093233090871, -29.56993018339339940, -15.49999999999999822 ) ) ;
#1672 = VERTEX_POINT ( 'NONE', #27382 ) ;
#1673 = AXIS2_PLACEMENT_3D ( 'NONE', #10532, #29286, #19619 ) ;
#1675 = CARTESIAN_POINT ( 'NONE',  ( 18.72828149013939125, -2.774847064971670552, -3.129399290372459674 ) ) ;
#1674 = CARTESIAN_POINT ( 'NONE',  ( 0.01821419288840892339, -26.61520874120817837, 7.779495906702012853 ) ) ;
#1676 = CARTESIAN_POINT ( 'NONE',  ( -70.92837670882074974, 0.2169278855384722815, 6.000000000000007994 ) ) ;
#1677 = CARTESIAN_POINT ( 'NONE',  ( 75.52602547247359155, 59.92744485144773137, 3.494507759123859358 ) ) ;
#1678 = VERTEX_POINT ( 'NONE', #30276 ) ;
#1679 = CARTESIAN_POINT ( 'NONE',  ( 23.39550106081508218, 2.664895405987246502, -4.239314792157373724 ) ) ;
#1680 = CARTESIAN_POINT ( 'NONE',  ( -62.85296432946437051, 36.91960874151882166, 4.452026683638354854 ) ) ;
#1681 = AXIS2_PLACEMENT_3D ( 'NONE', #30370, #39405, #20676 ) ;
#1682 = DIRECTION ( 'NONE',  ( -0.000000000000000000, -0.000000000000000000, 1.000000000000000000 ) ) ;
#1683 = CARTESIAN_POINT ( 'NONE',  ( -71.89960098016555889, -42.46322148352267334, 1.682209783512720325 ) ) ;
#1684 = CARTESIAN_POINT ( 'NONE',  ( -63.08379346057677139, 18.80112958435941906, 9.800414904976365804 ) ) ;
#1685 = CARTESIAN_POINT ( 'NONE',  ( 1.700390093233090871, -29.56993018339339940, 7.800000000000000711 ) ) ;
#1686 = CARTESIAN_POINT ( 'NONE',  ( 81.88652354500527508, 62.08144837224595847, 1.918505602738378224 ) ) ;
#1687 = CARTESIAN_POINT ( 'NONE',  ( 86.26657670271889344, 1.459011185482768314, -4.895973709007312991 ) ) ;
#1688 = CARTESIAN_POINT ( 'NONE',  ( 33.73883514186113075, -4.630787605642836091, -3.992050560354765576 ) ) ;
#1689 = CARTESIAN_POINT ( 'NONE',  ( -40.87867591359218977, -26.64985754041175525, 6.700000000000000178 ) ) ;
#1690 = CARTESIAN_POINT ( 'NONE',  ( -74.72715548395238727, -2.765387099023297157, -10.57877961556935098 ) ) ;
#1691 = CARTESIAN_POINT ( 'NONE',  ( 0.5882562476373008886, -26.35696177504351212, 6.889465824494256374 ) ) ;
#1692 = LINE ( 'NONE', #14225, #34172 ) ;
#1693 = CARTESIAN_POINT ( 'NONE',  ( 37.05749439986598759, -2.899774270594387637, -5.990116258624699874 ) ) ;
#1694 = DIRECTION ( 'NONE',  ( 0.000000000000000000, 1.000000000000000000, 0.000000000000000000 ) ) ;
#1695 = DIRECTION ( 'NONE',  ( -0.9267318687906771491, 0.3757233601570964532, 0.000000000000000000 ) ) ;
#1696 = CARTESIAN_POINT ( 'NONE',  ( 2.240298271943185870, -32.92678960775148056, 6.892063359921933419 ) ) ;
#1697 = EDGE_CURVE ( 'NONE', #3707, #35445, #36857, .T. ) ;
#1698 = AXIS2_PLACEMENT_3D ( 'NONE', #31877, #10433, #38229 ) ;
#1699 = CARTESIAN_POINT ( 'NONE',  ( -34.87867591359218977, -26.64985754041175525, 6.700000000000000178 ) ) ;
#1700 = CIRCLE ( 'NONE', #31296, 2.500000000000000444 ) ;
#1701 = ADVANCED_FACE ( 'NONE', ( #1892 ), #8641, .F. ) ;
#1702 = ORIENTED_EDGE ( 'NONE', *, *, #12600, .T. ) ;
#1703 = CARTESIAN_POINT ( 'NONE',  ( 36.69966961405233263, -3.382783021916500044, 5.888606945404527337 ) ) ;
#1704 = CARTESIAN_POINT ( 'NONE',  ( -70.70332177653823180, 0.1913546399533780362, 3.995777704139396924 ) ) ;
#1705 = CARTESIAN_POINT ( 'NONE',  ( 67.13068300324758297, 58.11650739856835202, -3.998197261021420701 ) ) ;
#1706 = VECTOR ( 'NONE', #19916, 1000.000000000000000 ) ;
#1707 = CARTESIAN_POINT ( 'NONE',  ( 3.058617350509197585, -26.34421757184894020, 7.009310105710484962 ) ) ;
#1708 = VERTEX_POINT ( 'NONE', #39529 ) ;
#1709 = DIRECTION ( 'NONE',  ( 1.000000000000000000, 0.000000000000000000, 0.000000000000000000 ) ) ;
#1710 = DIRECTION ( 'NONE',  ( 1.000000000000000000, -6.938893903907229167E-15, 0.000000000000000000 ) ) ;
#1711 = CARTESIAN_POINT ( 'NONE',  ( 85.66380979468560497, 0.8667738229574647457, -5.860807272458633754 ) ) ;
#1712 = CARTESIAN_POINT ( 'NONE',  ( -78.91378792136296738, 11.43306328107894032, 6.033766101647666247 ) ) ;
#1713 = CARTESIAN_POINT ( 'NONE',  ( 0.3374848729783252455, -32.79366859719224436, 7.002103980607166989 ) ) ;
#1714 = FACE_OUTER_BOUND ( 'NONE', #25111, .T. ) ;
#1715 = ORIENTED_EDGE ( 'NONE', *, *, #26675, .F. ) ;
#1716 = CARTESIAN_POINT ( 'NONE',  ( 24.06494024425525069, 3.347574872190568929, 3.211326713574206515 ) ) ;
#1717 = CARTESIAN_POINT ( 'NONE',  ( 0.9730757925788008356, -32.99329091482906762, 7.754798119455333705 ) ) ;
#1718 = CARTESIAN_POINT ( 'NONE',  ( 80.80454364895454944, 63.02910633771583093, 3.452358620554646151 ) ) ;
#1719 = CARTESIAN_POINT ( 'NONE',  ( -63.68563422865328505, 44.27494078859859883, 1.828866361102486238 ) ) ;
#1720 = ORIENTED_EDGE ( 'NONE', *, *, #30483, .F. ) ;
#1721 = CARTESIAN_POINT ( 'NONE',  ( 77.96902425052306285, 62.15836910947902538, -3.808649511194685200 ) ) ;
#1722 = B_SPLINE_CURVE_WITH_KNOTS ( 'NONE', 3,
 ( #37789, #12892, #38000, #9801 ),
 .UNSPECIFIED., .F., .F.,
 ( 4, 4 ),
 ( 0.000000000000000000, 1.000000000000000000 ),
 .UNSPECIFIED. ) ;
#1724 = CARTESIAN_POINT ( 'NONE',  ( 14.76771331554806999, -5.163171487644635960, -2.500000296585186632 ) ) ;
#1723 = CARTESIAN_POINT ( 'NONE',  ( 26.06744471409270147, 0.7518114339798734891, 4.421646308027469274 ) ) ;
#1725 = CARTESIAN_POINT ( 'NONE',  ( 78.68416471612006546, 66.05417514313620586, -1.083735637652206485 ) ) ;
#1726 = EDGE_CURVE ( 'NONE', #37911, #1142, #33590, .T. ) ;
#1727 = CARTESIAN_POINT ( 'NONE',  ( 79.47877296666170821, 61.98342160143343449, 3.470679136763286099 ) ) ;
#1728 = CIRCLE ( 'NONE', #31979, 0.1000000000000028644 ) ;
#1729 = CARTESIAN_POINT ( 'NONE',  ( 35.64856448684500378, -3.751217397768356054, -5.580918352854083331 ) ) ;
#1730 = VECTOR ( 'NONE', #27504, 1000.000000000000000 ) ;
#1731 = CARTESIAN_POINT ( 'NONE',  ( 80.34788146105277917, 66.29920961842019267, 1.394285451509447382 ) ) ;
#1732 = CARTESIAN_POINT ( 'NONE',  ( -81.07947155388369254, 30.81399289130168384, 9.800414904976365804 ) ) ;
#1733 = CARTESIAN_POINT ( 'NONE',  ( 29.34753533916922308, -2.431376398363487734, 5.582488461359439214 ) ) ;
#1734 = CARTESIAN_POINT ( 'NONE',  ( -64.08758708074091714, 36.87876644325631759, -4.900609702795900802 ) ) ;
#1735 = VERTEX_POINT ( 'NONE', #24502 ) ;
#1736 = CARTESIAN_POINT ( 'NONE',  ( -2.672839399606415256, -26.73366507310607076, 6.894806418505347700 ) ) ;
#1737 = CARTESIAN_POINT ( 'NONE',  ( 21.78667867209630060, 0.2188310260794802675, -8.380823656482592199 ) ) ;
#1738 = VECTOR ( 'NONE', #25826, 1000.000000000000000 ) ;
#1739 = EDGE_CURVE ( 'NONE', #13396, #17894, #21216, .T. ) ;
#1740 = CARTESIAN_POINT ( 'NONE',  ( -1.799609906766908685, -29.56993018339339940, 7.202408869016148074 ) ) ;
#1741 = CYLINDRICAL_SURFACE ( 'NONE', #26897, 0.1000000000000028644 ) ;
#1742 = ORIENTED_EDGE ( 'NONE', *, *, #27000, .F. ) ;
#1743 = CARTESIAN_POINT ( 'NONE',  ( 36.68395750019694646, -1.917487243977046729, -5.804568023447322034 ) ) ;
#1744 = LINE ( 'NONE', #1348, #22039 ) ;
#1745 = DIRECTION ( 'NONE',  ( 0.000000000000000000, -1.000000000000000000, 0.000000000000000000 ) ) ;
#1746 = DIRECTION ( 'NONE',  ( 1.000000000000000000, 0.000000000000000000, 0.000000000000000000 ) ) ;
#1747 = DIRECTION ( 'NONE',  ( 0.000000000000000000, 0.000000000000000000, 1.000000000000000000 ) ) ;
#1748 = CARTESIAN_POINT ( 'NONE',  ( 2.716203735777188211, -32.81465175439641513, 6.871394612369935651 ) ) ;
#1749 = CARTESIAN_POINT ( 'NONE',  ( -70.92837670882107659, -36.87473357531881391, 5.950000000000010836 ) ) ;
#1750 = CARTESIAN_POINT ( 'NONE',  ( 1.805519397879190135, -26.07149441967674974, 6.863784140767622333 ) ) ;
#1751 = EDGE_CURVE ( 'NONE', #39647, #9655, #36653, .T. ) ;
#1752 = ORIENTED_EDGE ( 'NONE', *, *, #9288, .F. ) ;
#1753 = ORIENTED_EDGE ( 'NONE', *, *, #35951, .F. ) ;
#1754 = CARTESIAN_POINT ( 'NONE',  ( 66.27376694608996388, 57.73522568913447373, 4.000000000000000000 ) ) ;
#1755 = CARTESIAN_POINT ( 'NONE',  ( 71.00148000485552302, 59.33579794997937995, -3.971832046809253391 ) ) ;
#1756 = ORIENTED_EDGE ( 'NONE', *, *, #13156, .F. ) ;
#1757 = CARTESIAN_POINT ( 'NONE',  ( 85.19771215196759329, 1.813128620488922760, 5.066052097874169213 ) ) ;
#1758 = CARTESIAN_POINT ( 'NONE',  ( -0.5390062018526512455, -32.25974509032589310, 7.635761828346574021 ) ) ;
#1759 = CARTESIAN_POINT ( 'NONE',  ( -16.24874870218063450, -26.64985754041175525, 6.700000000000000178 ) ) ;
#1760 = CARTESIAN_POINT ( 'NONE',  ( -38.87867591359218977, -24.55319635012989110, 6.700000000000000178 ) ) ;
#1761 = APPLICATION_PROTOCOL_DEFINITION ( 'draft international standard', 'automotive_design', 1998, #18698 ) ;
#1762 = VECTOR ( 'NONE', #8028, 1000.000000000000000 ) ;
#1763 = CARTESIAN_POINT ( 'NONE',  ( -14.87867591359218977, -24.55319635012989110, 6.800000000000000711 ) ) ;
#1764 = DIRECTION ( 'NONE',  ( 0.9396926207859126468, -0.3420201433256568335, -0.000000000000000000 ) ) ;
#1765 = CARTESIAN_POINT ( 'NONE',  ( -42.44874870218064444, -26.64985754041175525, 6.800000000000000711 ) ) ;
#1766 = CARTESIAN_POINT ( 'NONE',  ( 27.40362055195197755, -3.367332562137738794, 4.313861870170892843 ) ) ;
#1767 = ORIENTED_EDGE ( 'NONE', *, *, #38842, .T. ) ;
#1768 = CARTESIAN_POINT ( 'NONE',  ( 79.42292528565204179, 64.10449580132841163, -3.686141857899477348 ) ) ;
#1769 = CARTESIAN_POINT ( 'NONE',  ( 37.14318591385630697, -2.491847215272260829, 5.967311536227382085 ) ) ;
#1770 = ADVANCED_FACE ( 'NONE', ( #15029, #20796 ), #33390, .T. ) ;
#1771 = CARTESIAN_POINT ( 'NONE',  ( 80.75052706852349615, 61.66721672131043874, 2.660933152496148590 ) ) ;
#1772 = CARTESIAN_POINT ( 'NONE',  ( 0.2199985751287987512, -32.63861014186149845, 7.505001789837627335 ) ) ;
#1773 = CARTESIAN_POINT ( 'NONE',  ( 23.14887797670855107, 3.363171500915444589, 3.819340284631616900 ) ) ;
#1774 = CARTESIAN_POINT ( 'NONE',  ( 0.9235138160669791318, -32.98262327366389712, 7.010186378901970272 ) ) ;
#1775 = CARTESIAN_POINT ( 'NONE',  ( 16.11725891508299924, 15.27317977276803873, 2.500000000000000000 ) ) ;
#1776 = ADVANCED_FACE ( 'NONE', ( #26788 ), #18106, .T. ) ;
#1777 = CARTESIAN_POINT ( 'NONE',  ( 21.85643539959774628, 6.760345589247273246, -10.71366635798555578 ) ) ;
#1778 = VERTEX_POINT ( 'NONE', #11117 ) ;
#1779 = CARTESIAN_POINT ( 'NONE',  ( -80.90823458386326195, 10.55951580149532809, 0.6344085041158121774 ) ) ;
#1780 = EDGE_CURVE ( 'NONE', #6329, #6673, #5162, .T. ) ;
#1781 = EDGE_CURVE ( 'NONE', #32844, #18906, #1565, .T. ) ;
#1782 = CARTESIAN_POINT ( 'NONE',  ( 14.75796219645098795, -5.141356742665804447, 2.500016127560962254 ) ) ;
#1783 = CIRCLE ( 'NONE', #5060, 0.1000000000000028644 ) ;
#1784 = CARTESIAN_POINT ( 'NONE',  ( -77.44075151393023759, 9.727190932936968792, -9.175713659463616167 ) ) ;
#1785 = CARTESIAN_POINT ( 'NONE',  ( 4.643350526641022213, -31.46439155470594073, 7.013842709614101167 ) ) ;
#1786 = CARTESIAN_POINT ( 'NONE',  ( 37.01100706631705606, -2.247765066581573823, -5.912597513712233521 ) ) ;
#1787 = CARTESIAN_POINT ( 'NONE',  ( 81.26385631823474398, 62.29349618781995446, 2.861733672647093218 ) ) ;
#1788 = DIRECTION ( 'NONE',  ( 0.8660254037844393737, 0.000000000000000000, 0.4999999999999985567 ) ) ;
#1789 = CARTESIAN_POINT ( 'NONE',  ( -21.07867591359219617, -24.55319635012989110, 6.700000000000000178 ) ) ;
#1790 = LINE ( 'NONE', #17203, #33947 ) ;
#1791 = CARTESIAN_POINT ( 'NONE',  ( 0.5390211770124229140, -26.26822319535999384, 6.887161170156906209 ) ) ;
#1792 = VECTOR ( 'NONE', #31538, 1000.000000000000000 ) ;
#1793 = VECTOR ( 'NONE', #32468, 1000.000000000000114 ) ;
#1794 = AXIS2_PLACEMENT_3D ( 'NONE', #16703, #23114, #7454 ) ;
#1795 = CARTESIAN_POINT ( 'NONE',  ( 4.499507836142066175, -27.46875105750827117, 6.931070083220562061 ) ) ;
#1796 = CARTESIAN_POINT ( 'NONE',  ( 86.98314280420640898, 0.6541301300131903140, 4.930073579784800764 ) ) ;
#1797 = FACE_OUTER_BOUND ( 'NONE', #1223, .T. ) ;
#1798 = ADVANCED_FACE ( 'NONE', ( #14817 ), #24295, .F. ) ;
#1799 = CYLINDRICAL_SURFACE ( 'NONE', #31361, 0.09010775117052916006 ) ;
#1800 = CARTESIAN_POINT ( 'NONE',  ( 67.36808046129075933, 58.37408278799862416, 3.989212576213369221 ) ) ;
#1801 = CARTESIAN_POINT ( 'NONE',  ( 36.64085946849131403, -3.117955867178630935, 5.925090301229771761 ) ) ;
#1802 = VERTEX_POINT ( 'NONE', #25532 ) ;
#1803 = CARTESIAN_POINT ( 'NONE',  ( 2.246982590450817163, -33.01192690407003028, 7.785593909369613819 ) ) ;
#1804 = CARTESIAN_POINT ( 'NONE',  ( 86.49834695356116754, 1.198675839257056230, 5.248227958817050620 ) ) ;
#1806 = CYLINDRICAL_SURFACE ( 'NONE', #13869, 0.09010775117052903516 ) ;
#1805 = CARTESIAN_POINT ( 'NONE',  ( 80.71579011337402676, 63.33293116964227920, -3.563857694938807885 ) ) ;
#1807 =( BOUNDED_CURVE ( )  B_SPLINE_CURVE ( 3, ( #16042, #25522, #21824, #38067 ),
 .UNSPECIFIED., .F., .T. ) 
 B_SPLINE_CURVE_WITH_KNOTS ( ( 4, 4 ),
 ( 4.708531083176466403, 4.895802057644187855 ),
 .UNSPECIFIED. ) 
 CURVE ( )  GEOMETRIC_REPRESENTATION_ITEM ( )  RATIONAL_B_SPLINE_CURVE ( ( 1.000000000000000000, 0.9970795998553221295, 0.9970795998553221295, 1.000000000000000000 ) ) 
 REPRESENTATION_ITEM ( '' )  );
#1808 = CARTESIAN_POINT ( 'NONE',  ( -1.639146693691649892, -28.93157757802832819, 6.894806418505346812 ) ) ;
#1809 = CARTESIAN_POINT ( 'NONE',  ( -58.36416262933997245, 28.31210393328042585, 5.221062780410256288 ) ) ;
#1810 = VERTEX_POINT ( 'NONE', #22041 ) ;
#1811 = CARTESIAN_POINT ( 'NONE',  ( -0.5730865926811068434, -32.23100210249002373, 6.894806418505347700 ) ) ;
#1812 = ADVANCED_FACE ( 'NONE', ( #3333 ), #9456, .T. ) ;
#1813 = VERTEX_POINT ( 'NONE', #34000 ) ;
#1814 = CARTESIAN_POINT ( 'NONE',  ( -71.46462112523092003, -21.62705418684702252, 5.988032920670398163 ) ) ;
#1815 = B_SPLINE_CURVE_WITH_KNOTS ( 'NONE', 3,
 ( #35736, #25649, #16764, #28743, #6915, #16972, #552, #7510, #13088, #13896 ),
 .UNSPECIFIED., .F., .F.,
 ( 4, 3, 3, 4 ),
 ( 0.0005050348086185292486, 0.0005143352185143279303, 0.0005445898203825193500, 0.0005634294782181697644 ),
 .UNSPECIFIED. ) ;
#1816 = ORIENTED_EDGE ( 'NONE', *, *, #22261, .T. ) ;
#1817 = CARTESIAN_POINT ( 'NONE',  ( 79.68769792879572833, 64.63763403318208134, -3.508091314521180504 ) ) ;
#1818 = AXIS2_PLACEMENT_3D ( 'NONE', #37788, #37999, #15574 ) ;
#1819 = CARTESIAN_POINT ( 'NONE',  ( -1.525553370913913076, -28.21224846644693685, 7.010186378901971160 ) ) ;
#1820 = VECTOR ( 'NONE', #81, 1000.000000000000000 ) ;
#1821 = CARTESIAN_POINT ( 'NONE',  ( 79.68769792879609781, 64.63763403318228029, 3.508091314521096127 ) ) ;
#1822 = CARTESIAN_POINT ( 'NONE',  ( 26.76923719187233175, 1.540101848406568052, 4.364735894841153652 ) ) ;
#1824 = ORIENTED_EDGE ( 'NONE', *, *, #4744, .F. ) ;
#1823 = CARTESIAN_POINT ( 'NONE',  ( -0.7714601053644620787, -27.23540912346919285, 6.911401339314957148 ) ) ;
#1825 = AXIS2_PLACEMENT_3D ( 'NONE', #26664, #13699, #35935 ) ;
#1826 = B_SPLINE_CURVE_WITH_KNOTS ( 'NONE', 3,
 ( #8325, #1380, #10610, #29560, #35754, #13910, #32865, #17188, #33064, #5256, #20480, #4848, #1570, #14704, #20689, #17796 ),
 .UNSPECIFIED., .F., .F.,
 ( 4, 2, 2, 2, 2, 2, 2, 4 ),
 ( 0.000000000000000000, 0.002644435627895791452, 0.005288871255791582904, 0.006611089069739476028, 0.007933306883687369152, 0.009255524697635263143, 0.009916633604609207536, 0.01057774251158315366 ),
 .UNSPECIFIED. ) ;
#1827 = CARTESIAN_POINT ( 'NONE',  ( 75.27660179239936156, 61.98686977074611804, -3.846775394605563392 ) ) ;
#1828 = CARTESIAN_POINT ( 'NONE',  ( -70.42442292110172275, -21.65671257467926836, 5.980030958859729573 ) ) ;
#1830 = DIRECTION ( 'NONE',  ( -0.000000000000000000, -0.000000000000000000, -1.000000000000000000 ) ) ;
#1829 = CARTESIAN_POINT ( 'NONE',  ( -70.92837670882107659, -23.80776546975053165, -6.000000000000002665 ) ) ;
#1831 = FACE_OUTER_BOUND ( 'NONE', #14855, .T. ) ;
#1832 = EDGE_CURVE ( 'NONE', #20740, #908, #20462, .T. ) ;
#1833 = CARTESIAN_POINT ( 'NONE',  ( -2.489212967774009577, -31.84613700427082250, 6.954324564059724878 ) ) ;
#1834 = CARTESIAN_POINT ( 'NONE',  ( 22.76078985634742935, 3.901595487204953638, -3.625275301636816216 ) ) ;
#1835 = VERTEX_POINT ( 'NONE', #22257 ) ;
#1836 = CARTESIAN_POINT ( 'NONE',  ( -4.878675913592187108, -26.64985754041175525, 6.700000000000000178 ) ) ;
#1837 = EDGE_CURVE ( 'NONE', #21757, #26563, #23390, .T. ) ;
#1838 = CARTESIAN_POINT ( 'NONE',  ( 21.85643539959774273, 9.212406492340052822, 1.715677401501900956 ) ) ;
#1839 = FACE_OUTER_BOUND ( 'NONE', #19988, .T. ) ;
#1840 = CARTESIAN_POINT ( 'NONE',  ( 1.092632081715625203, -33.01346371419235481, 7.767720160662275219 ) ) ;
#1841 = CARTESIAN_POINT ( 'NONE',  ( 81.30751890104828306, 61.38951540425497200, 1.382728580145337505 ) ) ;
#1842 = CARTESIAN_POINT ( 'NONE',  ( 84.91553621511910421, 2.364970790127210787, 4.120477167815592701 ) ) ;
#1843 = CARTESIAN_POINT ( 'NONE',  ( 2.782197798051136317, -32.89830469346890141, 7.754798119455333705 ) ) ;
#1844 = ORIENTED_EDGE ( 'NONE', *, *, #4047, .F. ) ;
#1845 = DIRECTION ( 'NONE',  ( -1.000000000000000000, 0.000000000000000000, 0.000000000000000000 ) ) ;
#1846 = ORIENTED_EDGE ( 'NONE', *, *, #6440, .T. ) ;
#1847 = VECTOR ( 'NONE', #38622, 1000.000000000000000 ) ;
#1848 = LINE ( 'NONE', #5324, #11132 ) ;
#1849 = CARTESIAN_POINT ( 'NONE',  ( 26.27693392017907925, -3.249033630802554473, -4.181544638722900054 ) ) ;
#1850 = CARTESIAN_POINT ( 'NONE',  ( 34.92931741750302876, -1.710645300694223492, -5.657962770372154893 ) ) ;
#1851 = CARTESIAN_POINT ( 'NONE',  ( 8.290806648384990041, 0.000000000000000000, 6.000000000000000000 ) ) ;
#1852 = CARTESIAN_POINT ( 'NONE',  ( 22.33694865187872480, 0.2827817013730578033, -7.021907440927535937 ) ) ;
#1853 = DIRECTION ( 'NONE',  ( 1.000000000000000000, -0.000000000000000000, 0.000000000000000000 ) ) ;
#1854 = VERTEX_POINT ( 'NONE', #19145 ) ;
#1855 = CARTESIAN_POINT ( 'NONE',  ( 31.71703756440468069, -0.5641108459604192715, 5.156608810014274624 ) ) ;
#1856 = AXIS2_PLACEMENT_3D ( 'NONE', #19788, #35652, #4360 ) ;
#1857 = CARTESIAN_POINT ( 'NONE',  ( 5.022807544912395450, -28.47749337420469828, 7.766640943994347346 ) ) ;
#1858 = ORIENTED_EDGE ( 'NONE', *, *, #20133, .T. ) ;
#1859 = ORIENTED_EDGE ( 'NONE', *, *, #26010, .F. ) ;
#1860 = CARTESIAN_POINT ( 'NONE',  ( 37.00876839025129073, -3.246501946636328295, 5.946957662215321072 ) ) ;
#1861 = CARTESIAN_POINT ( 'NONE',  ( -1.632554375314136275, -30.63837106486143114, 6.870724624169666228 ) ) ;
#1862 = CARTESIAN_POINT ( 'NONE',  ( 16.71262745093176250, -3.379652782812611722, -2.787236875488859678 ) ) ;
#1863 = DIRECTION ( 'NONE',  ( 0.000000000000000000, 0.000000000000000000, 1.000000000000000000 ) ) ;
#1864 = VERTEX_POINT ( 'NONE', #24712 ) ;
#1865 = DIRECTION ( 'NONE',  ( 0.000000000000000000, 0.000000000000000000, -1.000000000000000000 ) ) ;
#1866 = ORIENTED_EDGE ( 'NONE', *, *, #31728, .F. ) ;
#1867 = EDGE_LOOP ( 'NONE', ( #38659, #24476, #2163, #38591 ) ) ;
#1868 = CARTESIAN_POINT ( 'NONE',  ( 0.000000000000000000, -0.5999999999999994227, -3.730072921939604047 ) ) ;
#1869 = CIRCLE ( 'NONE', #23572, 10.00000000000000888 ) ;
#1870 = EDGE_LOOP ( 'NONE', ( #14802, #25233, #20620, #14309 ) ) ;
#1871 = CARTESIAN_POINT ( 'NONE',  ( -56.22749146662674491, 30.67773648377160001, -3.904540345294674530 ) ) ;
#1872 = ORIENTED_EDGE ( 'NONE', *, *, #31070, .T. ) ;
#1873 = CARTESIAN_POINT ( 'NONE',  ( 4.809580840142714031, -27.96276457679604377, 6.887547729233689076 ) ) ;
#1874 = VERTEX_POINT ( 'NONE', #34209 ) ;
#1875 = EDGE_CURVE ( 'NONE', #37531, #18951, #31711, .T. ) ;
#1876 = CARTESIAN_POINT ( 'NONE',  ( 24.35455115775381785, 2.928845783586057738, 3.741716916781699709 ) ) ;
#1877 = CARTESIAN_POINT ( 'NONE',  ( 80.49077247797903567, 66.09228938494860017, -1.971256063808603631 ) ) ;
#1878 = ADVANCED_FACE ( 'NONE', ( #2915 ), #23044, .T. ) ;
#1879 = DIRECTION ( 'NONE',  ( 0.000000000000000000, 0.000000000000000000, 1.000000000000000000 ) ) ;
#1880 = EDGE_LOOP ( 'NONE', ( #32919, #33955, #32628, #37606, #11902 ) ) ;
#1882 = CARTESIAN_POINT ( 'NONE',  ( 1.075169146119493879, -26.22790998750958025, 7.680992449362119778 ) ) ;
#1881 = CARTESIAN_POINT ( 'NONE',  ( -38.97867591359219119, -24.55319635012989110, 6.700000000000000178 ) ) ;
#1883 = CARTESIAN_POINT ( 'NONE',  ( -1.796218690686571584, -29.41562043804214710, 6.880828092187096345 ) ) ;
#1884 = CARTESIAN_POINT ( 'NONE',  ( 75.05654786057638717, 62.45444674818786268, 3.685888554891597835 ) ) ;
#1885 = CARTESIAN_POINT ( 'NONE',  ( 22.71051984177768190, 2.583563127446080188, -4.683974715729272376 ) ) ;
#1886 = ORIENTED_EDGE ( 'NONE', *, *, #30787, .T. ) ;
#1887 = CARTESIAN_POINT ( 'NONE',  ( -64.08758708074093136, 37.74469198210200460, 4.273126118784214889 ) ) ;
#1888 = EDGE_CURVE ( 'NONE', #38890, #24333, #37427, .T. ) ;
#1889 = AXIS2_PLACEMENT_3D ( 'NONE', #26254, #13475, #22962 ) ;
#1890 = FACE_OUTER_BOUND ( 'NONE', #23994, .T. ) ;
#1891 = ADVANCED_FACE ( 'NONE', ( #11099 ), #39514, .F. ) ;
#1892 = FACE_OUTER_BOUND ( 'NONE', #37559, .T. ) ;
#1893 = CARTESIAN_POINT ( 'NONE',  ( -62.75245724414897808, 36.25555358314721843, 4.889260473756201542 ) ) ;
#1894 = DIRECTION ( 'NONE',  ( -0.000000000000000000, -0.000000000000000000, 1.000000000000000000 ) ) ;
#1896 = CARTESIAN_POINT ( 'NONE',  ( 81.44289297360093371, 64.86039221060747195, 2.864610283900509202 ) ) ;
#1895 = APPLICATION_CONTEXT ( 'automotive_design' ) ;
#1897 = CARTESIAN_POINT ( 'NONE',  ( 88.10293741339057760, -0.6036763236807990429, 2.641732887311516453 ) ) ;
#1898 = CARTESIAN_POINT ( 'NONE',  ( 31.05604276399450114, -2.500009215535430762, 5.784057531382419626 ) ) ;
#1899 = CARTESIAN_POINT ( 'NONE',  ( 4.198225232297463805, -33.92331276665304785, 7.635761828346577573 ) ) ;
#1900 = CARTESIAN_POINT ( 'NONE',  ( 4.647595270087047759, -31.26523263687563770, 7.763628509615284834 ) ) ;
#1901 = CARTESIAN_POINT ( 'NONE',  ( -81.21715035842910879, -5.646436377738331736, -3.817250611473149036 ) ) ;
#1902 = CARTESIAN_POINT ( 'NONE',  ( 23.84748567078391446, -3.102047020920744913, 3.830198175285921547 ) ) ;
#1903 = CARTESIAN_POINT ( 'NONE',  ( 0.04221685988047467475, -26.48763128618372065, 6.863784140767622333 ) ) ;
#1904 = CARTESIAN_POINT ( 'NONE',  ( 31.75256816120542425, -0.4599525743511591602, -5.162154218955760321 ) ) ;
#1905 = CYLINDRICAL_SURFACE ( 'NONE', #1033, 5.000000000000000000 ) ;
#1906 = DIRECTION ( 'NONE',  ( -0.2567910337120262732, -0.7055275666422161640, -0.6605219282605403475 ) ) ;
#1907 = CARTESIAN_POINT ( 'NONE',  ( 4.433004015503416717, -25.10972701691773779, 7.013842709614101167 ) ) ;
#1908 = CYLINDRICAL_SURFACE ( 'NONE', #36747, 0.1000000000000028644 ) ;
#1909 = CARTESIAN_POINT ( 'NONE',  ( -0.4624923041496786791, -32.19327532559099581, 7.661510568013091493 ) ) ;
#1910 = ORIENTED_EDGE ( 'NONE', *, *, #29793, .T. ) ;
#1911 = CARTESIAN_POINT ( 'NONE',  ( 35.36141464313556071, -3.735660561169047877, 5.554341061716538519 ) ) ;
#1912 = CARTESIAN_POINT ( 'NONE',  ( -64.08758708074091714, 38.34299140179737719, -3.014629887201876635 ) ) ;
#1913 = CARTESIAN_POINT ( 'NONE',  ( 67.62039053056824400, 58.58799842263783120, -3.976226663256291260 ) ) ;
#1914 = DIRECTION ( 'NONE',  ( 1.000000000000000000, 0.000000000000000000, 0.000000000000000000 ) ) ;
#1915 = EDGE_LOOP ( 'NONE', ( #25208, #504, #34556, #14770 ) ) ;
#1916 = EDGE_CURVE ( 'NONE', #32358, #40685, #13785, .T. ) ;
#1917 = CARTESIAN_POINT ( 'NONE',  ( -0.5737835481674327109, -32.09740712681197294, 7.759451378593101190 ) ) ;
#1918 = CARTESIAN_POINT ( 'NONE',  ( 1.822194502883781375, -26.17211269480022295, 7.754798119455333705 ) ) ;
#1919 = CARTESIAN_POINT ( 'NONE',  ( 76.98045162513071205, 64.85275298426677182, 2.378822723470982670 ) ) ;
#1920 = CARTESIAN_POINT ( 'NONE',  ( 1.054320629807504295, -32.90798264679612117, 6.887041543973314361 ) ) ;
#1921 = CARTESIAN_POINT ( 'NONE',  ( 0.3819031147581120056, -32.81210268184693746, 6.868546646838340486 ) ) ;
#1922 = CARTESIAN_POINT ( 'NONE',  ( -24.24874870218063450, -26.64985754041175525, 6.700000000000000178 ) ) ;
#1923 = ORIENTED_EDGE ( 'NONE', *, *, #27065, .T. ) ;
#1924 = CARTESIAN_POINT ( 'NONE',  ( 24.73621386372994380, 3.010848716420428062, 3.391332750938185203 ) ) ;
#1925 = CARTESIAN_POINT ( 'NONE',  ( 81.16955088369260807, 61.30397035488353197, -1.005837412005794906 ) ) ;
#1926 = CARTESIAN_POINT ( 'NONE',  ( 80.09489858828513320, 64.52483703883090982, 3.563857694938804777 ) ) ;
#1927 = VECTOR ( 'NONE', #36002, 1000.000000000000000 ) ;
#1928 = LINE ( 'NONE', #26624, #39013 ) ;
#1929 = ORIENTED_EDGE ( 'NONE', *, *, #35756, .F. ) ;
#1930 = CARTESIAN_POINT ( 'NONE',  ( 79.26553226962353449, 61.67928659302132388, -3.361664161258277161 ) ) ;
#1931 = B_SPLINE_CURVE_WITH_KNOTS ( 'NONE', 3,
 ( #31893, #12728, #28170, #3501, #6769, #9642, #12524, #31280, #25502, #35196 ),
 .UNSPECIFIED., .F., .F.,
 ( 4, 3, 3, 4 ),
 ( 0.0002170292169044773015, 0.0002420761345915959295, 0.0002723302478206993896, 0.0002816811360866744701 ),
 .UNSPECIFIED. ) ;
#1932 =( BOUNDED_SURFACE ( )  B_SPLINE_SURFACE ( 3, 2, ( 
 ( #17523, #7680, #33212 ),
 ( #19839, #20230, #17130 ),
 ( #30118, #1127, #26428 ),
 ( #29905, #38956, #14049 ) ),
 .UNSPECIFIED., .F., .F., .T. ) 
 B_SPLINE_SURFACE_WITH_KNOTS ( ( 4, 4 ),
 ( 3, 3 ),
 ( 0.1160256260365885861, 0.1317056536943987943 ),
 ( 0.000000000000000000, 0.8973000442991090342 ),
 .UNSPECIFIED. ) 
 GEOMETRIC_REPRESENTATION_ITEM ( )  RATIONAL_B_SPLINE_SURFACE ( (
 ( 1.000000000000000000, 0.9342716120537195579, 0.9864993949392519834),
 ( 1.000000000000000000, 0.9342716120537195579, 0.9864993949392519834),
 ( 1.000000000000000000, 0.9342716120537194469, 0.9864993949392519834),
 ( 1.000000000000000000, 0.9342716120537194469, 0.9864993949392519834) ) ) 
 REPRESENTATION_ITEM ( '' )  SURFACE ( )  );
#1934 = CARTESIAN_POINT ( 'NONE',  ( 2.277491769660097365, -26.21926552469281191, 7.635761828346577573 ) ) ;
#1933 = CARTESIAN_POINT ( 'NONE',  ( 24.11607445809433514, 0.4540071914542280762, 5.103030637244794221 ) ) ;
#1935 = CARTESIAN_POINT ( 'NONE',  ( 81.13122672739170582, 64.30755116178544029, -3.292658836668130640 ) ) ;
#1936 = CARTESIAN_POINT ( 'NONE',  ( 77.83481221125374816, 64.51125116100621426, 3.218236826935550798 ) ) ;
#1937 = ADVANCED_FACE ( 'NONE', ( #20372 ), #1463, .F. ) ;
#1938 = EDGE_CURVE ( 'NONE', #11548, #21166, #3302, .T. ) ;
#1939 = CARTESIAN_POINT ( 'NONE',  ( 35.41233797231917890, -3.779600677375021256, -5.524434929723343046 ) ) ;
#1940 = EDGE_CURVE ( 'NONE', #309, #774, #8122, .T. ) ;
#1941 = CARTESIAN_POINT ( 'NONE',  ( 81.46190421581952990, 61.46294189193149293, 1.114595100209201162 ) ) ;
#1943 = CARTESIAN_POINT ( 'NONE',  ( 37.83867290611771494, -6.084034091406928191, -6.000000000000000000 ) ) ;
#1942 = CARTESIAN_POINT ( 'NONE',  ( 4.361462012329716309, -31.84340686930758935, 6.894806418505347700 ) ) ;
#1944 = CARTESIAN_POINT ( 'NONE',  ( 27.52542935251784328, 0.09321990139520379415, -5.913109915068038624 ) ) ;
#1945 = DIRECTION ( 'NONE',  ( 0.000000000000000000, 0.000000000000000000, -1.000000000000000000 ) ) ;
#1946 = CARTESIAN_POINT ( 'NONE',  ( 4.582084150952498547, -31.37432464074042215, 7.754798119455333705 ) ) ;
#1947 = ORIENTED_EDGE ( 'NONE', *, *, #5919, .T. ) ;
#1948 = CARTESIAN_POINT ( 'NONE',  ( -81.80090188080515645, -5.603160304130406111, -0.6545554231109771415 ) ) ;
#1949 = CARTESIAN_POINT ( 'NONE',  ( 23.58764223058103227, 0.4154427152156035530, -5.528209969427812176 ) ) ;
#1950 = VECTOR ( 'NONE', #31112, 1000.000000000000000 ) ;
#1951 = CARTESIAN_POINT ( 'NONE',  ( -42.34874870218063592, -25.49307895267003587, 6.700000000000000178 ) ) ;
#1952 = LINE ( 'NONE', #5630, #5998 ) ;
#1953 = CARTESIAN_POINT ( 'NONE',  ( 5.159329814365638534, -29.03529183849990147, 6.867280401193707640 ) ) ;
#1954 = CARTESIAN_POINT ( 'NONE',  ( -71.84266479621042834, -48.31020963306245619, 9.958452096079875915 ) ) ;
#1955 = CARTESIAN_POINT ( 'NONE',  ( 30.88234279937811166, 0.6976323447808369105, -4.494874676303273198 ) ) ;
#1956 = CARTESIAN_POINT ( 'NONE',  ( 3.388683086819756163, -26.61871572696936994, 7.635761828346577573 ) ) ;
#1957 = CARTESIAN_POINT ( 'NONE',  ( -11.81496944966682960, -21.25669541281728669, 4.000000000000000000 ) ) ;
#1958 = CYLINDRICAL_SURFACE ( 'NONE', #12107, 3.000000000000002665 ) ;
#1959 = CARTESIAN_POINT ( 'NONE',  ( 5.000279045638660769, -30.73643474909027518, 7.670465701733750308 ) ) ;
#1960 = CARTESIAN_POINT ( 'NONE',  ( 2.664359094183485599, -32.83041543721814293, 6.969307238440505259 ) ) ;
#1961 = CARTESIAN_POINT ( 'NONE',  ( 1.686887486498408029, -26.16995699532097319, 7.635761828346577573 ) ) ;
#1962 = DIRECTION ( 'NONE',  ( 1.000000000000000000, 0.000000000000000000, 0.000000000000000000 ) ) ;
#1963 = AXIS2_PLACEMENT_3D ( 'NONE', #24863, #34356, #162 ) ;
#1964 = CARTESIAN_POINT ( 'NONE',  ( 2.183954541545420458, -33.03637977657594149, 6.867199677474202346 ) ) ;
#1965 = ORIENTED_EDGE ( 'NONE', *, *, #36863, .T. ) ;
#1966 = CARTESIAN_POINT ( 'NONE',  ( -69.72971309252355354, -48.03957001906470481, 5.880709122941769174 ) ) ;
#1967 = CARTESIAN_POINT ( 'NONE',  ( 66.41703863280932296, 57.80493748213761762, 4.000000000000019540 ) ) ;
#1968 = CARTESIAN_POINT ( 'NONE',  ( 73.73614897715009420, 59.29615633563123822, -3.619654763491260585 ) ) ;
#1969 = CARTESIAN_POINT ( 'NONE',  ( 4.289323970621365056, -27.35503128888597146, 7.257242401810561461 ) ) ;
#1970 = ORIENTED_EDGE ( 'NONE', *, *, #27641, .F. ) ;
#1971 = CARTESIAN_POINT ( 'NONE',  ( -62.92837670882106238, -23.80776546975053520, -6.000000000000000000 ) ) ;
#1972 = CARTESIAN_POINT ( 'NONE',  ( -0.5254690805390769270, -26.86890242742082080, 6.894806418505347700 ) ) ;
#1973 = CARTESIAN_POINT ( 'NONE',  ( 3.058784556509318797, -26.45307843876808462, 6.949473656533219135 ) ) ;
#1974 = EDGE_LOOP ( 'NONE', ( #15030, #13071, #3505, #26512, #37227 ) ) ;
#1975 = CARTESIAN_POINT ( 'NONE',  ( -0.9695225508750403565, -31.83301800158153227, 7.749999999999998224 ) ) ;
#1976 = PLANE ( 'NONE',  #31756 ) ;
#1977 = ORIENTED_EDGE ( 'NONE', *, *, #3672, .F. ) ;
#1978 = CARTESIAN_POINT ( 'NONE',  ( 24.08390956300509700, 3.360009220450308032, 3.160289221677234028 ) ) ;
#1979 = CIRCLE ( 'NONE', #22376, 10.00000000000000888 ) ;
#1980 = VERTEX_POINT ( 'NONE', #9444 ) ;
#1981 = CARTESIAN_POINT ( 'NONE',  ( 79.60839748543872929, 63.85977214187242623, -3.734652355492745102 ) ) ;
#1982 = CARTESIAN_POINT ( 'NONE',  ( 16.28258139852007957, 10.03625398311444705, -2.500000000000424993 ) ) ;
#1983 = CARTESIAN_POINT ( 'NONE',  ( 80.42678074443124103, 62.56544727678166140, 3.449595662144092412 ) ) ;
#1984 = CARTESIAN_POINT ( 'NONE',  ( 0.5660192589948234154, -26.36474644288341551, 7.782167645815905033 ) ) ;
#1985 = DIRECTION ( 'NONE',  ( 0.000000000000000000, 0.000000000000000000, 1.000000000000000000 ) ) ;
#1986 = AXIS2_PLACEMENT_3D ( 'NONE', #22368, #9786, #6511 ) ;
#1987 = ADVANCED_FACE ( 'NONE', ( #2899 ), #14440, .T. ) ;
#1988 = CARTESIAN_POINT ( 'NONE',  ( -105.6213936588467135, -59.15536422891795354, 9.800414904976365804 ) ) ;
#1989 = DIRECTION ( 'NONE',  ( -1.000000000000000000, 0.000000000000000000, 0.000000000000000000 ) ) ;
#1990 = CARTESIAN_POINT ( 'NONE',  ( 21.85643539959778181, 10.07385928288181987, 4.538892979079195200 ) ) ;
#1991 = EDGE_LOOP ( 'NONE', ( #13209, #16071, #3495, #40369 ) ) ;
#1992 = CARTESIAN_POINT ( 'NONE',  ( -79.67878442765989178, 10.46676075307951592, 4.855440592539105538 ) ) ;
#1993 = ORIENTED_EDGE ( 'NONE', *, *, #28989, .F. ) ;
#1994 = CARTESIAN_POINT ( 'NONE',  ( 14.73988855999587422, -5.058265782967484192, 2.500274136440799211 ) ) ;
#1995 = CARTESIAN_POINT ( 'NONE',  ( -80.59971289683194584, 10.50603676119796503, -5.334131017465025160 ) ) ;
#1996 = CARTESIAN_POINT ( 'NONE',  ( 1.554942410987211865, -32.96681772520712883, 6.868387053540520704 ) ) ;
#1997 = CARTESIAN_POINT ( 'NONE',  ( 2.346459556658704315, -26.23187771999068119, 6.887041543973313473 ) ) ;
#1998 = CARTESIAN_POINT ( 'NONE',  ( 79.68007496026341130, 65.35156779369863500, 3.108243619504650113 ) ) ;
#1999 = CARTESIAN_POINT ( 'NONE',  ( -69.08758708074093136, 35.93730870640389696, -8.800414904976364028 ) ) ;
#2000 = CARTESIAN_POINT ( 'NONE',  ( -63.08758708074094557, 43.61223004741321319, -1.000000000000000000 ) ) ;
#2001 = CARTESIAN_POINT ( 'NONE',  ( -4.890026461918812295, -8.951974136083761024, 2.500000000000000000 ) ) ;
#2002 = CARTESIAN_POINT ( 'NONE',  ( -70.92837670881976919, 0.2170085631237942680, 10.00000000000113154 ) ) ;
#2003 = CARTESIAN_POINT ( 'NONE',  ( -64.24852075262772644, 34.84521132811198640, 5.064982173168631086 ) ) ;
#2004 = CARTESIAN_POINT ( 'NONE',  ( 87.91376162421416041, -0.3911850984532471154, 3.331745215148313122 ) ) ;
#2005 = CARTESIAN_POINT ( 'NONE',  ( 4.172416336262816827, -31.90426121769112555, 6.997764925645185485 ) ) ;
#2006 = VERTEX_POINT ( 'NONE', #36843 ) ;
#2007 = CARTESIAN_POINT ( 'NONE',  ( 67.37599051809213790, 58.35250968650521486, 3.990882853436548139 ) ) ;
#2008 = CARTESIAN_POINT ( 'NONE',  ( 36.19519395851039434, -2.229529781144294898, 5.855533419936117312 ) ) ;
#2009 = EDGE_CURVE ( 'NONE', #13035, #3867, #19725, .T. ) ;
#2010 = CARTESIAN_POINT ( 'NONE',  ( 2.222359783566090208, -33.02043838110294871, 7.780491323090172884 ) ) ;
#2011 = CARTESIAN_POINT ( 'NONE',  ( 86.86561140461988373, 0.2703162379016064154, -5.930766725306959586 ) ) ;
#2012 = AXIS2_PLACEMENT_3D ( 'NONE', #37068, #27397, #30291 ) ;
#2014 = CARTESIAN_POINT ( 'NONE',  ( 33.70392053634464702, -1.255035446422470891, -5.466709950731788226 ) ) ;
#2013 = CARTESIAN_POINT ( 'NONE',  ( 31.00707005056823817, -0.8718966892480422004, 5.891928739871540088 ) ) ;
#2015 = CARTESIAN_POINT ( 'NONE',  ( -1.621787578243040651, -28.84658016871684794, 6.865312560952603782 ) ) ;
#2016 = CARTESIAN_POINT ( 'NONE',  ( 2.363993368752974167, -26.14856561996513662, 7.785593909369613819 ) ) ;
#2017 = CARTESIAN_POINT ( 'NONE',  ( -0.6924112550790449960, -32.12424229857576563, 6.971170733404098208 ) ) ;
#2018 = ORIENTED_EDGE ( 'NONE', *, *, #8403, .T. ) ;
#2019 = EDGE_CURVE ( 'NONE', #17221, #8271, #9087, .T. ) ;
#2020 = VERTEX_POINT ( 'NONE', #22027 ) ;
#2021 = ORIENTED_EDGE ( 'NONE', *, *, #4492, .F. ) ;
#2022 = CARTESIAN_POINT ( 'NONE',  ( 80.81138441778081472, 62.13752223189714385, -3.030715982579941681 ) ) ;
#2023 = CARTESIAN_POINT ( 'NONE',  ( 4.200390093233091093, -29.56993018339339940, 6.800000000000000711 ) ) ;
#2024 = CARTESIAN_POINT ( 'NONE',  ( 79.49051211673885575, 64.87125159350641468, 3.403428918328328834 ) ) ;
#2025 = CARTESIAN_POINT ( 'NONE',  ( 22.22833818514967419, 0.9551375975900053827, 6.581072739463595944 ) ) ;
#2027 = ORIENTED_EDGE ( 'NONE', *, *, #21238, .T. ) ;
#2026 = CARTESIAN_POINT ( 'NONE',  ( -0.7792710424444403428, -27.24370714888392442, 6.895222827070024429 ) ) ;
#2028 = VECTOR ( 'NONE', #21034, 1000.000000000000000 ) ;
#2029 = CARTESIAN_POINT ( 'NONE',  ( 74.43259725886051115, 60.83706718145764114, -3.924711207976804950 ) ) ;
#2030 = CARTESIAN_POINT ( 'NONE',  ( -81.07947155388369254, 30.81399289130168384, 12.49999999999999645 ) ) ;
#2031 = EDGE_CURVE ( 'NONE', #7067, #4684, #22895, .T. ) ;
#2033 = CARTESIAN_POINT ( 'NONE',  ( 11.29080664838498826, -10.90558813203967148, 6.000000000000000000 ) ) ;
#2032 = CARTESIAN_POINT ( 'NONE',  ( 91.69672933337632514, -4.640393979863029372, -6.000000000000000888 ) ) ;
#2034 = CARTESIAN_POINT ( 'NONE',  ( -1.203028700869076095, -27.80068031303635223, 7.782034975670476307 ) ) ;
#2035 = DIRECTION ( 'NONE',  ( -0.7660444431189725734, -0.6427876096865456912, -0.000000000000000000 ) ) ;
#2036 = CARTESIAN_POINT ( 'NONE',  ( 1.700390093233090871, -29.56993018339339940, 7.800000000000000711 ) ) ;
#2037 = CARTESIAN_POINT ( 'NONE',  ( 21.91451482393930306, 5.430938580357159040, -3.368358593842193383 ) ) ;
#2038 = ORIENTED_EDGE ( 'NONE', *, *, #215, .T. ) ;
#2039 = CARTESIAN_POINT ( 'NONE',  ( -52.01549048184568846, -30.94667987854474234, 4.800000000000000711 ) ) ;
#2040 = CARTESIAN_POINT ( 'NONE',  ( 22.82080504511013430, -6.970192185297126031, -1.116939615399285657 ) ) ;
#2041 = CIRCLE ( 'NONE', #39505, 0.1000000000000028644 ) ;
#2042 = CARTESIAN_POINT ( 'NONE',  ( -0.9575446616272440536, -31.84707375580262578, 7.698786668945011513 ) ) ;
#2043 = CARTESIAN_POINT ( 'NONE',  ( 4.979040433996382298, -28.34499767243864810, 7.660770905198782899 ) ) ;
#2044 = CARTESIAN_POINT ( 'NONE',  ( 81.58232553938692888, 62.71761900942991730, 2.892908819267544729 ) ) ;
#2045 = CARTESIAN_POINT ( 'NONE',  ( 85.85763368383675243, 1.114829962406831410, -5.799110970849834068 ) ) ;
#2046 = CARTESIAN_POINT ( 'NONE',  ( 2.921324086407800280, -26.64985754041175525, 6.700000000000000178 ) ) ;
#2047 = EDGE_LOOP ( 'NONE', ( #3058, #8960, #20319, #1430, #12735 ) ) ;
#2048 = PLANE ( 'NONE',  #33916 ) ;
#2049 = EDGE_CURVE ( 'NONE', #15393, #2537, #290, .T. ) ;
#2050 = B_SPLINE_CURVE_WITH_KNOTS ( 'NONE', 3,
 ( #483, #38322, #7244, #13626, #13019, #22709, #22904, #38127, #31977, #29279, #9929, #26197, #22511, #10525, #19405, #10119, #32378, #21378, #5937, #32977, #15188, #18476, #32783, #37417, #36260, #33957, #31061, #4762, #9213, #27548, #17099 ),
 .UNSPECIFIED., .F., .F.,
 ( 4, 3, 3, 3, 3, 3, 3, 3, 3, 3, 4 ),
 ( 9.697399036122160616E-19, 2.999644130997572721E-05, 6.002588995694706019E-05, 8.960886084587848111E-05, 0.0001190604700446479952, 0.0001489538463052703923, 0.0001796139255493973670, 0.0002109707048517048017, 0.0002426195318110344079, 0.0002740640997890034193, 0.0002849778069099790528 ),
 .UNSPECIFIED. ) ;
#2051 = CARTESIAN_POINT ( 'NONE',  ( 3.551251297819357777, -25.49307895267003587, 6.800000000000000711 ) ) ;
#2052 = CARTESIAN_POINT ( 'NONE',  ( 14.81973502151181243, -5.946294937045099260, -2.518644691825020931 ) ) ;
#2053 = CARTESIAN_POINT ( 'NONE',  ( 35.45276959245764203, -1.916775701034503898, -5.739660142012472654 ) ) ;
#2054 = LINE ( 'NONE', #27347, #37824 ) ;
#2055 = CARTESIAN_POINT ( 'NONE',  ( 23.10155575571232234, 0.3729460866388023543, -5.910048752073230105 ) ) ;
#2056 = CARTESIAN_POINT ( 'NONE',  ( -0.4463135599462602632, -26.93331026361374470, 7.785868773668302545 ) ) ;
#2057 = VERTEX_POINT ( 'NONE', #34806 ) ;
#2058 = CARTESIAN_POINT ( 'NONE',  ( 21.25143394907042449, 3.315796038557054182, 3.523198254261666218 ) ) ;
#2059 = VECTOR ( 'NONE', #22867, 1000.000000000000000 ) ;
#2060 = CARTESIAN_POINT ( 'NONE',  ( 31.84521792906302906, -2.966245498930080160, -5.176614455973063578 ) ) ;
#2061 = ORIENTED_EDGE ( 'NONE', *, *, #9157, .T. ) ;
#2062 = VERTEX_POINT ( 'NONE', #10800 ) ;
#2063 = CARTESIAN_POINT ( 'NONE',  ( 37.01052352883407082, -2.248283349646221563, 5.912786814818789871 ) ) ;
#2064 = CIRCLE ( 'NONE', #23726, 0.1000000000000028644 ) ;
#2065 = CYLINDRICAL_SURFACE ( 'NONE', #35968, 8.080217238368769372 ) ;
#2066 = ADVANCED_FACE ( 'NONE', ( #19129 ), #29751, .F. ) ;
#2067 = EDGE_CURVE ( 'NONE', #21810, #21380, #35663, .T. ) ;
#2068 = CYLINDRICAL_SURFACE ( 'NONE', #40521, 0.1000000000000028644 ) ;
#2069 = CYLINDRICAL_SURFACE ( 'NONE', #777, 2.500000000000002220 ) ;
#2070 = ORIENTED_EDGE ( 'NONE', *, *, #18627, .T. ) ;
#2071 = EDGE_CURVE ( 'NONE', #18532, #22978, #40503, .T. ) ;
#2072 = DIRECTION ( 'NONE',  ( 1.000000000000000000, 0.000000000000000000, 0.000000000000000000 ) ) ;
#2073 = VERTEX_POINT ( 'NONE', #32454 ) ;
#2074 = VECTOR ( 'NONE', #40514, 999.9999999999998863 ) ;
#2075 = VERTEX_POINT ( 'NONE', #4254 ) ;
#2076 = CARTESIAN_POINT ( 'NONE',  ( 0.1069670619869697303, -26.56643171602332032, 7.754798119455333705 ) ) ;
#2077 = CARTESIAN_POINT ( 'NONE',  ( 79.19089293128583051, 65.62284279856319813, -2.735335646780913788 ) ) ;
#2078 = CARTESIAN_POINT ( 'NONE',  ( -58.91453996558632156, 28.99622802882459638, -6.206785453512805972 ) ) ;
#2079 = ORIENTED_EDGE ( 'NONE', *, *, #27186, .T. ) ;
#2080 = CARTESIAN_POINT ( 'NONE',  ( 4.746899557684813864, -27.84691535960167030, 6.894806418505347700 ) ) ;
#2081 = ORIENTED_EDGE ( 'NONE', *, *, #25583, .F. ) ;
#2082 = CARTESIAN_POINT ( 'NONE',  ( 22.49878221582566340, 4.485478565812190510, 3.364408562939156244 ) ) ;
#2083 = CARTESIAN_POINT ( 'NONE',  ( 81.66247121191628366, 61.65231731326586839, -1.378120381825870266 ) ) ;
#2084 = CARTESIAN_POINT ( 'NONE',  ( -1.718189074305093600, -25.68532020122240311, 7.754798119455333705 ) ) ;
#2085 = ORIENTED_EDGE ( 'NONE', *, *, #29510, .T. ) ;
#2087 = CARTESIAN_POINT ( 'NONE',  ( 18.17282410049547536, -2.848335441370983379, -3.042706730930791803 ) ) ;
#2086 = CARTESIAN_POINT ( 'NONE',  ( 0.02667858525708081963, -26.61042181407449192, 7.782167645815904145 ) ) ;
#2088 = CARTESIAN_POINT ( 'NONE',  ( -80.92837670882107659, 2.429809908903242555, 12.50000000000000000 ) ) ;
#2089 = CARTESIAN_POINT ( 'NONE',  ( 76.25423822322979106, 59.84407948384421161, 3.204585025132129950 ) ) ;
#2090 = CARTESIAN_POINT ( 'NONE',  ( 24.46993583969108244, 2.591970903540452120, -3.976734763430334496 ) ) ;
#2091 = CARTESIAN_POINT ( 'NONE',  ( -36.97867591359219119, -26.64985754041175525, 6.800000000000000711 ) ) ;
#2092 = DIRECTION ( 'NONE',  ( -1.000000000000000000, 0.000000000000000000, 0.000000000000000000 ) ) ;
#2093 = CARTESIAN_POINT ( 'NONE',  ( -66.22295697853020613, 35.49170696305580464, 7.967283012326582536 ) ) ;
#2094 = CARTESIAN_POINT ( 'NONE',  ( 81.00802433895704269, 65.38516391083565793, 2.726953404243151802 ) ) ;
#2095 = CARTESIAN_POINT ( 'NONE',  ( 86.64693249831780975, 1.031777503091004800, -5.158387491453222395 ) ) ;
#2096 = CARTESIAN_POINT ( 'NONE',  ( 31.72291873093343284, -3.714249907566092634, 4.801291842747894556 ) ) ;
#2097 = DIRECTION ( 'NONE',  ( 1.000000000000000000, 0.000000000000000000, 0.000000000000000000 ) ) ;
#2098 = CARTESIAN_POINT ( 'NONE',  ( 3.913290293412393872, -32.15122301917286762, 7.695279973900954751 ) ) ;
#2099 = CARTESIAN_POINT ( 'NONE',  ( 14.91371995633972247, -5.924865805607109515, 2.519702374887847096 ) ) ;
#2100 = DIRECTION ( 'NONE',  ( -0.9848077530122091305, 0.1736481776669241417, -0.000000000000000000 ) ) ;
#2101 = CIRCLE ( 'NONE', #19838, 0.1000000000000028644 ) ;
#2102 = CARTESIAN_POINT ( 'NONE',  ( 35.50436178781468755, -1.785355687363928689, -5.747712351859902924 ) ) ;
#2103 = CARTESIAN_POINT ( 'NONE',  ( 4.738207753463742122, -31.30822356001046458, 7.635761828346574021 ) ) ;
#2104 = CARTESIAN_POINT ( 'NONE',  ( 5.191948456685583579, -29.66439323399636407, 7.776484688137390577 ) ) ;
#2105 = LINE ( 'NONE', #4974, #34272 ) ;
#2106 = ADVANCED_FACE ( 'NONE', ( #17375 ), #15506, .F. ) ;
#2107 = DIRECTION ( 'NONE',  ( 0.000000000000000000, 0.000000000000000000, -1.000000000000000000 ) ) ;
#2108 = CARTESIAN_POINT ( 'NONE',  ( -70.17520183749425655, -45.81613455447481442, 5.953107086803218095 ) ) ;
#2109 = EDGE_CURVE ( 'NONE', #33369, #14626, #30795, .T. ) ;
#2110 = VERTEX_POINT ( 'NONE', #17790 ) ;
#2111 = CARTESIAN_POINT ( 'NONE',  ( 37.06794226148818439, -2.451797619550506901, 5.964046084392197855 ) ) ;
#2112 = CARTESIAN_POINT ( 'NONE',  ( -70.21272673770054951, -0.07566977545864603250, 3.957576123060443596 ) ) ;
#2113 = CARTESIAN_POINT ( 'NONE',  ( 66.98823442903206171, 58.05250069757015297, -3.998791315154375692 ) ) ;
#2114 = EDGE_CURVE ( 'NONE', #39964, #16562, #33886, .T. ) ;
#2115 = CARTESIAN_POINT ( 'NONE',  ( -58.99872204295123623, 28.26327478256400383, -6.631997745857265869 ) ) ;
#2116 = VERTEX_POINT ( 'NONE', #5666 ) ;
#2117 = CARTESIAN_POINT ( 'NONE',  ( -10.44874870218064089, -25.49307895267003587, 6.800000000000000711 ) ) ;
#2118 = CARTESIAN_POINT ( 'NONE',  ( 3.794562874143936781, -32.24844578246045046, 7.759451378593092308 ) ) ;
#2119 = CARTESIAN_POINT ( 'NONE',  ( -71.90228189594579078, -21.04538751579064737, 5.920650877785229582 ) ) ;
#2120 = CARTESIAN_POINT ( 'NONE',  ( -75.29003035974771763, 9.883927643020312459, 9.004751556950759905 ) ) ;
#2121 = CARTESIAN_POINT ( 'NONE',  ( -37.07867591359219261, -26.64985754041175525, 6.700000000000000178 ) ) ;
#2122 = EDGE_CURVE ( 'NONE', #2020, #23233, #18410, .T. ) ;
#2123 = CARTESIAN_POINT ( 'NONE',  ( 1.276579259530898458, -26.09568431166286828, 6.921725064902952695 ) ) ;
#2124 = ORIENTED_EDGE ( 'NONE', *, *, #23648, .F. ) ;
#2125 = CARTESIAN_POINT ( 'NONE',  ( 23.74487617493794644, 3.563056966343403076, 3.179706526333272887 ) ) ;
#2126 = CARTESIAN_POINT ( 'NONE',  ( 82.44648106056945380, 62.87232481290443076, -1.233992409460997308 ) ) ;
#2127 = CARTESIAN_POINT ( 'NONE',  ( 81.02087009143654939, 62.46468763289096415, 3.155412080370043615 ) ) ;
#2128 = DIRECTION ( 'NONE',  ( 0.000000000000000000, 0.000000000000000000, -1.000000000000000000 ) ) ;
#2129 = VERTEX_POINT ( 'NONE', #27678 ) ;
#2130 = CARTESIAN_POINT ( 'NONE',  ( 79.17274970258590372, 61.87635977960857758, -3.505091495581010630 ) ) ;
#2132 = CARTESIAN_POINT ( 'NONE',  ( 14.72813615105396323, -4.875043543781444555, -2.502213707555314581 ) ) ;
#2131 = CARTESIAN_POINT ( 'NONE',  ( 27.43005921570062355, 0.9938728547065163177, 4.487513223811070873 ) ) ;
#2133 = CARTESIAN_POINT ( 'NONE',  ( 81.15996319168233697, 61.30045982539696325, -1.094381639753446045 ) ) ;
#2134 = CARTESIAN_POINT ( 'NONE',  ( 79.37220710802424151, 62.20501526703846906, 3.590127757398436259 ) ) ;
#2135 = AXIS2_PLACEMENT_3D ( 'NONE', #31784, #38746, #31994 ) ;
#2136 = ORIENTED_EDGE ( 'NONE', *, *, #11028, .F. ) ;
#2137 = CARTESIAN_POINT ( 'NONE',  ( -0.8845957367844016206, -27.36134505743407530, 7.782167645815903256 ) ) ;
#2138 = CARTESIAN_POINT ( 'NONE',  ( 82.33093480182121482, 62.53300266214105108, 1.299258709308648729 ) ) ;
#2141 = VERTEX_POINT ( 'NONE', #12018 ) ;
#2140 = CARTESIAN_POINT ( 'NONE',  ( 5.150390093233091271, -29.56993018339339940, 6.800000000000000711 ) ) ;
#2139 = CARTESIAN_POINT ( 'NONE',  ( -75.45330471031414277, 33.71485196875532608, -8.800414904976364028 ) ) ;
#2142 = CARTESIAN_POINT ( 'NONE',  ( 27.17726507492083599, 0.7866376163037266389, 5.581651230154481169 ) ) ;
#2143 = DIRECTION ( 'NONE',  ( 0.000000000000000000, 0.000000000000000000, 1.000000000000000000 ) ) ;
#2144 = DIRECTION ( 'NONE',  ( -0.000000000000000000, -0.000000000000000000, 1.000000000000000000 ) ) ;
#2145 = ORIENTED_EDGE ( 'NONE', *, *, #16317, .F. ) ;
#2146 = CARTESIAN_POINT ( 'NONE',  ( -1.722970638209900596, -28.84261588273779964, 7.754798119455333705 ) ) ;
#2147 = CARTESIAN_POINT ( 'NONE',  ( 21.78050909960382953, 0.2073865793812009195, -8.415697349445284914 ) ) ;
#2148 = EDGE_CURVE ( 'NONE', #18519, #2141, #6073, .T. ) ;
#2149 = CARTESIAN_POINT ( 'NONE',  ( -1.699609906766908818, -29.56993018339339940, 7.800000000000000711 ) ) ;
#2150 = CARTESIAN_POINT ( 'NONE',  ( -0.8980191362577285563, -27.22509128144364610, 7.750000000000000888 ) ) ;
#2151 = CARTESIAN_POINT ( 'NONE',  ( 5.175086729718587186, -29.14981455392978660, 6.931070083220560285 ) ) ;
#2152 = CARTESIAN_POINT ( 'NONE',  ( -72.38841993492154359, -47.51249456017484363, 9.893128921701961787 ) ) ;
#2153 = CARTESIAN_POINT ( 'NONE',  ( 37.21138578923722662, -2.744110368974991498, -6.000908943309275045 ) ) ;
#2154 = CARTESIAN_POINT ( 'NONE',  ( 3.369155479471896530, -26.60763004909045293, 7.693875151218755981 ) ) ;
#2155 = DIRECTION ( 'NONE',  ( 0.000000000000000000, 0.000000000000000000, 1.000000000000000000 ) ) ;
#2156 = LINE ( 'NONE', #30142, #981 ) ;
#2157 = FACE_OUTER_BOUND ( 'NONE', #188, .T. ) ;
#2158 = CYLINDRICAL_SURFACE ( 'NONE', #40412, 7.999999999999986677 ) ;
#2159 = CARTESIAN_POINT ( 'NONE',  ( 4.893494088014897159, -28.40195944670255912, 7.763628509615286610 ) ) ;
#2160 = CARTESIAN_POINT ( 'NONE',  ( 2.829405163535268386, -26.36285597610873310, 7.693875151218754205 ) ) ;
#2161 = CARTESIAN_POINT ( 'NONE',  ( 21.79832107181720957, 1.471655218185874858, -6.775317797187613067 ) ) ;
#2162 = CARTESIAN_POINT ( 'NONE',  ( 2.173839223709712609, -33.03777254838963273, 6.870724624169667116 ) ) ;
#2163 = ORIENTED_EDGE ( 'NONE', *, *, #8162, .T. ) ;
#2164 = CARTESIAN_POINT ( 'NONE',  ( 66.27376694608996388, 57.73522568913447373, 4.000000000000000000 ) ) ;
#2165 = CARTESIAN_POINT ( 'NONE',  ( 69.13527637438681950, 58.97494527044376866, -3.984982412582154687 ) ) ;
#2166 = EDGE_CURVE ( 'NONE', #15412, #463, #32244, .T. ) ;
#2167 = EDGE_CURVE ( 'NONE', #3715, #26905, #3424, .T. ) ;
#2168 = EDGE_LOOP ( 'NONE', ( #22253, #14634, #30880, #6210 ) ) ;
#2169 = DIRECTION ( 'NONE',  ( 0.000000000000000000, 0.000000000000000000, 1.000000000000000000 ) ) ;
#2170 = EDGE_CURVE ( 'NONE', #10700, #14079, #25417, .T. ) ;
#2171 = CARTESIAN_POINT ( 'NONE',  ( 0.1649012726517564975, -26.53640515764040231, 7.013842709614101167 ) ) ;
#2172 = CARTESIAN_POINT ( 'NONE',  ( 17.97454669799173033, 51.66243977840390045, 1.000000000000000000 ) ) ;
#2173 = CARTESIAN_POINT ( 'NONE',  ( 4.703888560603170177, -27.97650715214728123, 7.754798119455333705 ) ) ;
#2174 =( BOUNDED_SURFACE ( )  B_SPLINE_SURFACE ( 3, 2, ( 
 ( #12198, #3187, #22309 ),
 ( #15905, #28464, #271 ),
 ( #25383, #15493, #25177 ),
 ( #37315, #12811, #21688 ),
 ( #24559, #19201, #9309 ),
 ( #28253, #34266, #18373 ),
 ( #6037, #79, #34876 ),
 ( #37923, #31767, #15083 ),
 ( #27644, #28053, #37708 ),
 ( #40200, #11981, #37113 ),
 ( #18572, #8899, #2974 ),
 ( #31158, #21887, #37514 ),
 ( #21482, #40602, #34465 ),
 ( #12610, #9517, #22098 ),
 ( #34060, #30960, #2765 ),
 ( #20199, #35075, #3581 ) ),
 .UNSPECIFIED., .F., .F., .F. ) 
 B_SPLINE_SURFACE_WITH_KNOTS ( ( 4, 2, 2, 2, 2, 2, 2, 4 ),
 ( 3, 3 ),
 ( 7.589415207398531038E-18, 0.0009755768803159603443, 0.001463365320473936776, 0.001951153760631913099, 0.002438942200789889422, 0.002926730640947865746, 0.003414519081105842069, 0.003902307521263818826 ),
 ( 0.000000000000000000, 1.000000000000000000 ),
 .UNSPECIFIED. ) 
 GEOMETRIC_REPRESENTATION_ITEM ( )  RATIONAL_B_SPLINE_SURFACE ( (
 ( 1.000000000000000000, 0.6029302108204158683, 1.000000000000000000),
 ( 1.000000000000000000, 0.5783298881757151788, 1.000000000000000000),
 ( 1.000000000000000000, 0.5522465926628815636, 1.000000000000000000),
 ( 1.000000000000000000, 0.5169885426013864915, 1.000000000000000000),
 ( 1.000000000000000000, 0.5061025709684146001, 1.000000000000000000),
 ( 1.000000000000000000, 0.4881721342722146750, 1.000000000000000000),
 ( 1.000000000000000000, 0.4810711757772043184, 1.000000000000000000),
 ( 1.000000000000000000, 0.4726640060677125832, 1.000000000000000000),
 ( 1.000000000000000000, 0.4715283203431503423, 1.000000000000000000),
 ( 1.000000000000000000, 0.4761415489114605992, 1.000000000000000000),
 ( 1.000000000000000000, 0.4818043763597624762, 1.000000000000000000),
 ( 1.000000000000000000, 0.4989518560459819119, 1.000000000000000000),
 ( 1.000000000000000000, 0.5102645520264953438, 1.000000000000000000),
 ( 1.000000000000000000, 0.5358562791028443906, 1.000000000000000000),
 ( 1.000000000000000000, 0.5501980292661390326, 1.000000000000000000),
 ( 1.000000000000000000, 0.5652620711642688534, 1.000000000000000000) ) ) 
 REPRESENTATION_ITEM ( '' )  SURFACE ( )  );
#2175 = FACE_OUTER_BOUND ( 'NONE', #30006, .T. ) ;
#2176 = CARTESIAN_POINT ( 'NONE',  ( -1.799591427079094030, -29.58235858030848675, 7.756555456908253987 ) ) ;
#2177 = VERTEX_POINT ( 'NONE', #112 ) ;
#2178 = CARTESIAN_POINT ( 'NONE',  ( -69.08758708074093136, 24.84364830758653397, -3.800414904976364028 ) ) ;
#2179 = VERTEX_POINT ( 'NONE', #28708 ) ;
#2180 = CARTESIAN_POINT ( 'NONE',  ( 79.46360196572365453, 64.13050462409741215, -3.681573067026198576 ) ) ;
#2181 = CARTESIAN_POINT ( 'NONE',  ( 18.26922853518255252, 11.64739320590812888, -2.500000000000005773 ) ) ;
#2182 = CARTESIAN_POINT ( 'NONE',  ( 81.80618415539481703, 63.87961589575506594, -2.903340743335492302 ) ) ;
#2183 = CARTESIAN_POINT ( 'NONE',  ( 80.80786883982545987, 61.35646782832052537, 2.148686496494744080 ) ) ;
#2184 = B_SPLINE_CURVE_WITH_KNOTS ( 'NONE', 3,
 ( #9126, #30772, #2574, #39599, #36720, #15096, #8503, #21086, #37125, #8913 ),
 .UNSPECIFIED., .F., .F.,
 ( 4, 3, 3, 4 ),
 ( 0.000000000000000000, 3.025570593003320367E-05, 6.051145698344263427E-05, 6.468151674593523946E-05 ),
 .UNSPECIFIED. ) ;
#2185 = FACE_OUTER_BOUND ( 'NONE', #9760, .T. ) ;
#2186 = CARTESIAN_POINT ( 'NONE',  ( 4.042068651234693277, -27.10486591319729754, 6.969307238440507923 ) ) ;
#2187 = CARTESIAN_POINT ( 'NONE',  ( -77.95330471031414277, 33.71485196875532608, 21.52833696633422988 ) ) ;
#2188 = CARTESIAN_POINT ( 'NONE',  ( 21.85643539959774273, 11.87467848218428834, -0.9583437110454642305 ) ) ;
#2189 = ORIENTED_EDGE ( 'NONE', *, *, #29979, .F. ) ;
#2190 = DIRECTION ( 'NONE',  ( -1.000000000000000000, 0.000000000000000000, 0.000000000000000000 ) ) ;
#2191 = AXIS2_PLACEMENT_3D ( 'NONE', #9283, #25359, #37897 ) ;
#2192 = CARTESIAN_POINT ( 'NONE',  ( 14.76646934850686321, -4.520893997360137639, 2.511033383266843888 ) ) ;
#2193 = CARTESIAN_POINT ( 'NONE',  ( -74.87089915843765198, 7.795108144428510855, -9.236877437684523073 ) ) ;
#2194 = CARTESIAN_POINT ( 'NONE',  ( 1.564919489175762735, -32.96724492301107290, 6.865312560952603782 ) ) ;
#2195 = CARTESIAN_POINT ( 'NONE',  ( 2.363242046172057353, -26.23515549482586096, 6.874555630061442102 ) ) ;
#2196 = CARTESIAN_POINT ( 'NONE',  ( 4.899937972425366439, -30.72010120057137073, 7.635761828346577573 ) ) ;
#2197 = CARTESIAN_POINT ( 'NONE',  ( 14.72032977250883334, 13.14393988312540529, 2.499678740116445752 ) ) ;
#2198 = CARTESIAN_POINT ( 'NONE',  ( -24.87867591359218977, -26.64985754041175525, 6.800000000000000711 ) ) ;
#2199 = CARTESIAN_POINT ( 'NONE',  ( 0.03162470699431464694, -32.53223031769636009, 7.695279973900954751 ) ) ;
#2200 = CARTESIAN_POINT ( 'NONE',  ( -0.2278126045957919732, -32.49907834724773892, 7.387053503561885393 ) ) ;
#2201 = CIRCLE ( 'NONE', #35737, 6.681288188914807691 ) ;
#2202 = DIRECTION ( 'NONE',  ( 1.000000000000000000, 0.000000000000000000, 0.000000000000000000 ) ) ;
#2203 = DIRECTION ( 'NONE',  ( 0.000000000000000000, 1.000000000000000000, 0.000000000000000000 ) ) ;
#2204 = CARTESIAN_POINT ( 'NONE',  ( 4.169225371885145748, -31.90763414548703736, 6.920489980334481928 ) ) ;
#2205 = EDGE_LOOP ( 'NONE', ( #36341, #27877, #24437, #30151 ) ) ;
#2206 = CARTESIAN_POINT ( 'NONE',  ( 68.05544300132015678, 58.31078564718745127, 3.995571880668738363 ) ) ;
#2207 = CARTESIAN_POINT ( 'NONE',  ( 34.13188676842981550, -3.213403896779438718, 5.533504431668644585 ) ) ;
#2208 = EDGE_CURVE ( 'NONE', #39394, #6683, #34217, .T. ) ;
#2209 = DIRECTION ( 'NONE',  ( 0.000000000000000000, 0.000000000000000000, 1.000000000000000000 ) ) ;
#2210 = CARTESIAN_POINT ( 'NONE',  ( 88.65680102019307185, -1.418189719613276223, -2.767552868364703045 ) ) ;
#2211 = ADVANCED_FACE ( 'NONE', ( #12236 ), #15533, .T. ) ;
#2213 = CARTESIAN_POINT ( 'NONE',  ( 4.858345136377215212, -30.82986309310958717, 6.864651958020304257 ) ) ;
#2212 = CARTESIAN_POINT ( 'NONE',  ( 31.80158048871438581, -1.669318041804891850, 6.009059823207920203 ) ) ;
#2214 = DIRECTION ( 'NONE',  ( 1.000000000000000000, 0.000000000000000000, 0.000000000000000000 ) ) ;
#2215 = CARTESIAN_POINT ( 'NONE',  ( -63.08379346057677139, 18.80112958435941906, -9.800414904976365804 ) ) ;
#2216 = CARTESIAN_POINT ( 'NONE',  ( -0.5981535632466232766, -32.20939563122895777, 6.870737987065014707 ) ) ;
#2217 = EDGE_LOOP ( 'NONE', ( #7470, #10552, #37349, #36551, #15075 ) ) ;
#2218 = CARTESIAN_POINT ( 'NONE',  ( -69.92837670882107659, -20.78299143688747819, 5.928123921495640936 ) ) ;
#2219 = ORIENTED_EDGE ( 'NONE', *, *, #23789, .F. ) ;
#2220 = EDGE_LOOP ( 'NONE', ( #19687, #27231, #11268, #39519 ) ) ;
#2221 = CARTESIAN_POINT ( 'NONE',  ( 80.48752863069321961, 62.90068369996134834, -3.525318766974259166 ) ) ;
#2222 = FACE_OUTER_BOUND ( 'NONE', #18144, .T. ) ;
#2223 = CARTESIAN_POINT ( 'NONE',  ( 79.17340063025110908, 65.28954359503943294, 3.030715982579951451 ) ) ;
#2224 = CARTESIAN_POINT ( 'NONE',  ( 26.67559340739115115, 0.9924815708228320599, 4.380057119474870753 ) ) ;
#2226 = ORIENTED_EDGE ( 'NONE', *, *, #20409, .T. ) ;
#2225 = CARTESIAN_POINT ( 'NONE',  ( 4.757778760719634903, -27.89174059054909094, 7.782861076432730840 ) ) ;
#2227 = DIRECTION ( 'NONE',  ( 1.000000000000000000, 0.000000000000000000, 0.000000000000000000 ) ) ;
#2228 = VECTOR ( 'NONE', #35385, 1000.000000000000000 ) ;
#2229 = CARTESIAN_POINT ( 'NONE',  ( 73.86803306573551708, 62.08347648694399368, -3.642458757454824614 ) ) ;
#2230 = VECTOR ( 'NONE', #34040, 1000.000000000000000 ) ;
#2231 = CARTESIAN_POINT ( 'NONE',  ( 3.215891561669039778, -32.61348987959953405, 6.969307238440507923 ) ) ;
#2233 = DIRECTION ( 'NONE',  ( -0.000000000000000000, -0.000000000000000000, 1.000000000000000000 ) ) ;
#2232 = CARTESIAN_POINT ( 'NONE',  ( -0.5122432252254431884, -25.35718825981775382, 6.894806418505347700 ) ) ;
#2234 = CARTESIAN_POINT ( 'NONE',  ( -0.7036529332303063100, -33.97746366811107777, 7.754798119455333705 ) ) ;
#2235 = CARTESIAN_POINT ( 'NONE',  ( -69.08758708074093136, 36.88538962427716683, 8.800414904976364028 ) ) ;
#2236 = CARTESIAN_POINT ( 'NONE',  ( -1.588256500155083240, -30.72927027690474588, 7.783750581861600182 ) ) ;
#2237 = EDGE_CURVE ( 'NONE', #3709, #38484, #12067, .T. ) ;
#2238 = CARTESIAN_POINT ( 'NONE',  ( 22.22276440514101381, 5.121701983031256233, -3.164228572747696422 ) ) ;
#2239 = ORIENTED_EDGE ( 'NONE', *, *, #3669, .T. ) ;
#2240 = CARTESIAN_POINT ( 'NONE',  ( 2.427704393887406109, -26.14656945195773119, 7.754798119455333705 ) ) ;
#2241 = CARTESIAN_POINT ( 'NONE',  ( 26.56634348862415251, 2.991955253353971500, -0.5426703667890996341 ) ) ;
#2242 = CARTESIAN_POINT ( 'NONE',  ( 28.52663967383706023, 50.14399159706750453, 1.000000000000000000 ) ) ;
#2243 = CARTESIAN_POINT ( 'NONE',  ( 4.980612442748399538, -28.34920280925516067, 7.651421919295148477 ) ) ;
#2244 = CARTESIAN_POINT ( 'NONE',  ( 81.40528610411782040, 61.52959015154564071, 1.692865493182717840 ) ) ;
#2245 = CARTESIAN_POINT ( 'NONE',  ( 84.85978623402763787, 2.253055191119315737, -4.296636491436513161 ) ) ;
#2246 = CARTESIAN_POINT ( 'NONE',  ( -42.24874870218063450, -25.49307895267003587, 6.800000000000000711 ) ) ;
#2247 = EDGE_LOOP ( 'NONE', ( #37637, #20979, #7092, #5383, #24729, #13471, #35158, #1970, #9566, #30476, #35986, #38208, #17257, #8671, #568, #8414, #19701, #30000, #31642, #34439, #8412, #35612, #36565, #19976, #32199, #12550, #28388, #10697, #37997, #5132, #17816, #36421, #21136, #15271, #2911, #28020, #38944, #3852, #29067, #5595, #31313, #9348, #8981, #14811, #37671, #32166, #16658, #29257, #924, #20770, #38872, #1452, #22742, #11385, #4690, #10496, #28593, #17131, #6628, #24887, #28531, #27213, #5335, #2550, #31484, #14702, #634, #33370, #38957, #20583, #11954, #15069, #22955, #12057, #39174, #26267, #2677, #11741, #28224, #11570, #8617, #27262, #2085, #2493, #20124, #6337, #12944, #29023, #30223, #40017, #20313, #23227, #21014, #31960, #30017, #9656, #11589, #6267, #13165, #35393, #25301, #32133, #3515, #4497, #8922, #22876, #34969, #23283, #26326, #5836 ) ) ;
#2248 = CARTESIAN_POINT ( 'NONE',  ( 3.021324086407803478, -26.64985754041175525, 6.700000000000000178 ) ) ;
#2249 = EDGE_CURVE ( 'NONE', #14798, #25728, #39563, .T. ) ;
#2250 = CARTESIAN_POINT ( 'NONE',  ( 5.062217907964971175, -29.06188122502908300, 6.870716933885666400 ) ) ;
#2251 = CARTESIAN_POINT ( 'NONE',  ( 21.51474421073843502, -2.978796432270695682, -3.508324343008054846 ) ) ;
#2252 = CARTESIAN_POINT ( 'NONE',  ( -63.99293516169446150, 35.89893413629673091, -7.506047544094580637 ) ) ;
#2253 = PLANE ( 'NONE',  #7556 ) ;
#2254 = CARTESIAN_POINT ( 'NONE',  ( -0.4228120283973959559, -26.91435142379919299, 7.782034975670478083 ) ) ;
#2255 = EDGE_LOOP ( 'NONE', ( #30060, #4003, #25056, #9557, #12158, #12053, #15972, #4464 ) ) ;
#2256 = CARTESIAN_POINT ( 'NONE',  ( 2.828915453401516622, -32.86827817813306751, 7.784725160561909441 ) ) ;
#2257 = CARTESIAN_POINT ( 'NONE',  ( 86.06238440510853138, 1.688369665709827272, 4.446988894268222303 ) ) ;
#2258 = EDGE_CURVE ( 'NONE', #12826, #20627, #22745, .T. ) ;
#2259 = ORIENTED_EDGE ( 'NONE', *, *, #13212, .F. ) ;
#2260 = ORIENTED_EDGE ( 'NONE', *, *, #9898, .F. ) ;
#2262 = CARTESIAN_POINT ( 'NONE',  ( 33.68538319921849933, -3.842697165577637186, 5.135126983811714396 ) ) ;
#2261 = CARTESIAN_POINT ( 'NONE',  ( 81.29039616289740877, 62.30485139745669443, -2.850064543546689588 ) ) ;
#2263 = CARTESIAN_POINT ( 'NONE',  ( -1.328168952220487586, -31.31782122304711180, 7.767720160662272555 ) ) ;
#2264 = CARTESIAN_POINT ( 'NONE',  ( 16.87423662129170765, -3.093369055974038329, 2.840030748344179568 ) ) ;
#2265 = CARTESIAN_POINT ( 'NONE',  ( 16.92519036607385985, -3.330348903852535791, -2.818005368153482237 ) ) ;
#2266 = CARTESIAN_POINT ( 'NONE',  ( -1.697427395360086244, -29.44812577374269580, 7.754798119455333705 ) ) ;
#2267 = ORIENTED_EDGE ( 'NONE', *, *, #10039, .F. ) ;
#2268 = CARTESIAN_POINT ( 'NONE',  ( -69.08758708074093136, 24.84364830758653397, 8.800414904976364028 ) ) ;
#2269 = ORIENTED_EDGE ( 'NONE', *, *, #8966, .T. ) ;
#2270 = VERTEX_POINT ( 'NONE', #1326 ) ;
#2271 = CARTESIAN_POINT ( 'NONE',  ( -5.316495087772349137, -32.84709638682603838, -2.500000000000000444 ) ) ;
#2272 = AXIS2_PLACEMENT_3D ( 'NONE', #11107, #29658, #1470 ) ;
#2273 = CARTESIAN_POINT ( 'NONE',  ( 80.99158576241018181, 62.18982880056436358, -2.968223699503256263 ) ) ;
#2274 = CARTESIAN_POINT ( 'NONE',  ( 27.60344192425479193, 81.15229837709949834, 1.000000000000000000 ) ) ;
#2275 = ORIENTED_EDGE ( 'NONE', *, *, #4572, .T. ) ;
#2277 = CARTESIAN_POINT ( 'NONE',  ( 4.330482794039245853, -27.41523602638843826, 7.784838882742139532 ) ) ;
#2276 = CARTESIAN_POINT ( 'NONE',  ( 4.812521983982041895, -27.96848237138598137, 7.013842709614101167 ) ) ;
#2278 = ORIENTED_EDGE ( 'NONE', *, *, #8027, .F. ) ;
#2279 = CARTESIAN_POINT ( 'NONE',  ( 82.23158145857209433, 63.37565065107707341, -2.326649614738084182 ) ) ;
#2280 = EDGE_CURVE ( 'NONE', #33469, #30519, #10206, .T. ) ;
#2281 = DIRECTION ( 'NONE',  ( 0.000000000000000000, 0.000000000000000000, 1.000000000000000000 ) ) ;
#2282 = VERTEX_POINT ( 'NONE', #23335 ) ;
#2284 = CARTESIAN_POINT ( 'NONE',  ( 26.06061125667445921, -2.757087722844052902, -4.273786683505784723 ) ) ;
#2283 = DIRECTION ( 'NONE',  ( 0.000000000000000000, 0.000000000000000000, 1.000000000000000000 ) ) ;
#2285 = CARTESIAN_POINT ( 'NONE',  ( 1.700390093233090871, -29.56993018339339940, 7.750000000000000888 ) ) ;
#2286 = CARTESIAN_POINT ( 'NONE',  ( 75.65523814419378823, 61.17064132828575396, 3.882889210543257974 ) ) ;
#2287 = CARTESIAN_POINT ( 'NONE',  ( 22.65677964865432870, 3.082858489129792545, -4.336902647173903169 ) ) ;
#2288 = VECTOR ( 'NONE', #1694, 1000.000000000000000 ) ;
#2289 = CARTESIAN_POINT ( 'NONE',  ( -0.2130774203410400469, -26.63113507583277695, 7.139344958878410807 ) ) ;
#2290 = CIRCLE ( 'NONE', #12098, 3.499999999999999556 ) ;
#2291 = CARTESIAN_POINT ( 'NONE',  ( 1.079328522417935421, -26.12547340107537863, 7.635761828346579350 ) ) ;
#2292 = ORIENTED_EDGE ( 'NONE', *, *, #7895, .T. ) ;
#2293 = FACE_OUTER_BOUND ( 'NONE', #31505, .T. ) ;
#2294 = CARTESIAN_POINT ( 'NONE',  ( 82.01382571621898876, 63.62535219989236168, 2.645340681430091045 ) ) ;
#2295 = CARTESIAN_POINT ( 'NONE',  ( 85.17388679999480416, 2.686372346413934409, 1.032998165733738816 ) ) ;
#2296 = DIRECTION ( 'NONE',  ( 1.000000000000000000, 0.000000000000000000, 0.000000000000000000 ) ) ;
#2297 = EDGE_CURVE ( 'NONE', #38669, #22132, #38337, .T. ) ;
#2298 = CARTESIAN_POINT ( 'NONE',  ( -18.24874870218063450, -25.49307895267003587, 6.700000000000000178 ) ) ;
#2299 = ADVANCED_FACE ( 'NONE', ( #20234 ), #19648, .F. ) ;
#2300 = AXIS2_PLACEMENT_3D ( 'NONE', #39101, #26169, #4151 ) ;
#2301 = CARTESIAN_POINT ( 'NONE',  ( 2.721058752466466224, -32.91780047479638682, 6.921725064902950919 ) ) ;
#2302 = ORIENTED_EDGE ( 'NONE', *, *, #7859, .F. ) ;
#2303 = CARTESIAN_POINT ( 'NONE',  ( 21.53627039407701460, -3.050411829391824536, 3.479264532985287595 ) ) ;
#2304 = CARTESIAN_POINT ( 'NONE',  ( -0.01667042123058508352, -26.52005313930425601, 6.887161170156905321 ) ) ;
#2305 = CARTESIAN_POINT ( 'NONE',  ( 36.14161076797949335, -3.144492548583445846, -5.847170467139393146 ) ) ;
#2306 = DIRECTION ( 'NONE',  ( -1.000000000000000000, -0.000000000000000000, -0.000000000000000000 ) ) ;
#2307 = CARTESIAN_POINT ( 'NONE',  ( -17.07867591359219617, -26.64985754041175525, 6.700000000000000178 ) ) ;
#2308 = CYLINDRICAL_SURFACE ( 'NONE', #36846, 0.09010775117053060335 ) ;
#2309 = CARTESIAN_POINT ( 'NONE',  ( 4.307676847859603697, -31.90100969392960906, 7.766640943994648438 ) ) ;
#2310 = CARTESIAN_POINT ( 'NONE',  ( 1.723121472978328406, -33.06985636609709900, 7.742274884880762542 ) ) ;
#2311 = ADVANCED_FACE ( 'NONE', ( #39571 ), #33434, .F. ) ;
#2312 = ORIENTED_EDGE ( 'NONE', *, *, #26458, .T. ) ;
#2313 = CARTESIAN_POINT ( 'NONE',  ( 20.85071236293282482, 4.522924277292770689, 2.940040760293478161 ) ) ;
#2314 = CARTESIAN_POINT ( 'NONE',  ( -71.70854571598145810, -0.1474806467180565794, 5.961650403247826802 ) ) ;
#2315 = CARTESIAN_POINT ( 'NONE',  ( 66.83382626670835691, 58.02146702699413794, -3.998465113256441938 ) ) ;
#2316 = CARTESIAN_POINT ( 'NONE',  ( 4.298799322723926508, -31.91476908534313850, 7.750000000000000888 ) ) ;
#2317 = CARTESIAN_POINT ( 'NONE',  ( -1.337427566997555717, -27.83163680677632001, 7.635761828346574021 ) ) ;
#2318 = AXIS2_PLACEMENT_3D ( 'NONE', #30036, #14373, #26943 ) ;
#2319 = ORIENTED_EDGE ( 'NONE', *, *, #33578, .T. ) ;
#2320 = AXIS2_PLACEMENT_3D ( 'NONE', #2000, #26494, #7745 ) ;
#2321 = DIRECTION ( 'NONE',  ( 0.3420201433256790380, -0.9396926207859046531, -0.000000000000000000 ) ) ;
#2322 = CARTESIAN_POINT ( 'NONE',  ( -75.61141378505557498, -5.258309523962441112, -8.843508591838688204 ) ) ;
#2323 = CARTESIAN_POINT ( 'NONE',  ( -71.54295603092448630, -21.58232592843834396, 5.969163363928941202 ) ) ;
#2324 = LINE ( 'NONE', #31286, #29415 ) ;
#2325 = AXIS2_PLACEMENT_3D ( 'NONE', #18583, #2989, #2368 ) ;
#2326 = ORIENTED_EDGE ( 'NONE', *, *, #6440, .F. ) ;
#2327 = CARTESIAN_POINT ( 'NONE',  ( 0.4918310210129015481, -32.74788313599579936, 6.894806418505344148 ) ) ;
#2328 = CARTESIAN_POINT ( 'NONE',  ( 2.976970822604137368, -26.41868572423151207, 7.754798119455333705 ) ) ;
#2329 = ORIENTED_EDGE ( 'NONE', *, *, #16967, .F. ) ;
#2330 = CARTESIAN_POINT ( 'NONE',  ( 23.72810756034646218, 3.537902271613312610, 3.249573880183133312 ) ) ;
#2331 = CARTESIAN_POINT ( 'NONE',  ( 81.96779975749585390, 61.96402392828839822, -1.065376284871803581 ) ) ;
#2332 = CARTESIAN_POINT ( 'NONE',  ( 79.09180288389933366, 65.81009211479097587, 2.442092683901131434 ) ) ;
#2333 = EDGE_CURVE ( 'NONE', #3701, #1652, #26316, .T. ) ;
#2334 = PLANE ( 'NONE',  #38990 ) ;
#2335 = ORIENTED_EDGE ( 'NONE', *, *, #10534, .T. ) ;
#2336 = CARTESIAN_POINT ( 'NONE',  ( 78.44508438210819179, 62.63916802445879028, -3.816136337383043919 ) ) ;
#2338 = CARTESIAN_POINT ( 'NONE',  ( 14.62968864654182433, -4.708885747848794878, -2.500000000000228706 ) ) ;
#2337 = CARTESIAN_POINT ( 'NONE',  ( 22.61186175525197939, 0.2941385288943472176, 6.499543881263520895 ) ) ;
#2339 = CARTESIAN_POINT ( 'NONE',  ( 80.95699988732381769, 64.21667718577664630, -3.402511877377342842 ) ) ;
#2340 = CARTESIAN_POINT ( 'NONE',  ( -1.086373026989221113, -31.68746443619045650, 7.013842709614101167 ) ) ;
#2341 = CARTESIAN_POINT ( 'NONE',  ( 80.20105671851041507, 61.18620973470589064, 2.431999527814463935 ) ) ;
#2342 = VERTEX_POINT ( 'NONE', #5204 ) ;
#2343 = ORIENTED_EDGE ( 'NONE', *, *, #13097, .T. ) ;
#2344 = CARTESIAN_POINT ( 'NONE',  ( 35.77311163637067182, -3.731966479379717594, -5.611466549886873878 ) ) ;
#2345 = EDGE_CURVE ( 'NONE', #33227, #4406, #24338, .T. ) ;
#2346 = ORIENTED_EDGE ( 'NONE', *, *, #32057, .F. ) ;
#2347 = CARTESIAN_POINT ( 'NONE',  ( 81.73112818161185089, 61.68666564161353705, 1.174937739208268050 ) ) ;
#2349 = FACE_BOUND ( 'NONE', #29906, .T. ) ;
#2348 = DIRECTION ( 'NONE',  ( -0.4999999999999918954, -0.8660254037844432595, -0.000000000000000000 ) ) ;
#2350 = CARTESIAN_POINT ( 'NONE',  ( 30.13988473044573624, 0.1694294105150049301, -5.382122866902316893 ) ) ;
#2351 = B_SPLINE_CURVE_WITH_KNOTS ( 'NONE', 3,
 ( #6009, #15058, #37082, #24740, #21045, #27411, #28024, #8873, #39974, #2739, #5599, #5804, #5393, #30307 ),
 .UNSPECIFIED., .F., .F.,
 ( 4, 2, 2, 2, 2, 2, 4 ),
 ( 0.000000000000000000, 0.002649657113267142768, 0.005299314226534285535, 0.007948971339801423966, 0.009273799896434993181, 0.009936214174751781258, 0.01059862845306856587 ),
 .UNSPECIFIED. ) ;
#2352 = CARTESIAN_POINT ( 'NONE',  ( -1.771784689607549979, -30.01038707958819174, 7.013842709614101167 ) ) ;
#2353 = DIRECTION ( 'NONE',  ( 0.000000000000000000, 0.000000000000000000, 1.000000000000000000 ) ) ;
#2354 = CARTESIAN_POINT ( 'NONE',  ( -81.72496613755205885, -5.611374088600661558, 1.578727716436091333 ) ) ;
#2355 = CARTESIAN_POINT ( 'NONE',  ( 25.38754743222835231, 0.7148885839003105147, -4.601077336691401953 ) ) ;
#2356 = EDGE_CURVE ( 'NONE', #15938, #25969, #9713, .T. ) ;
#2357 = CARTESIAN_POINT ( 'NONE',  ( 1.578585683582427235, -32.96774767198657941, 7.754798119455333705 ) ) ;
#2358 = AXIS2_PLACEMENT_3D ( 'NONE', #25493, #16604, #392 ) ;
#2359 = FACE_OUTER_BOUND ( 'NONE', #18590, .T. ) ;
#2360 = VECTOR ( 'NONE', #7370, 1000.000000000000000 ) ;
#2361 = CARTESIAN_POINT ( 'NONE',  ( 0.5360542692519894015, -32.87058578193457237, 7.678495282201401650 ) ) ;
#2362 = CARTESIAN_POINT ( 'NONE',  ( -71.41219010185693605, -48.54025046412724009, 9.988702396128939398 ) ) ;
#2363 = CARTESIAN_POINT ( 'NONE',  ( 23.38378197942683201, 3.557987824482284456, -3.100743960359395146 ) ) ;
#2364 = LINE ( 'NONE', #33652, #10169 ) ;
#2365 = DIRECTION ( 'NONE',  ( -0.000000000000000000, 1.000000000000000000, 0.000000000000000000 ) ) ;
#2366 = DIRECTION ( 'NONE',  ( 1.000000000000000000, 0.000000000000000000, 0.000000000000000000 ) ) ;
#2367 = CARTESIAN_POINT ( 'NONE',  ( 0.5039019691771889908, -32.85561263111923580, 7.767720160662273443 ) ) ;
#2368 = DIRECTION ( 'NONE',  ( 0.000000000000000000, 0.000000000000000000, 1.000000000000000000 ) ) ;
#2369 = CARTESIAN_POINT ( 'NONE',  ( -73.32694038987526142, 5.199692155526626891, 10.90380950792603443 ) ) ;
#2370 = CIRCLE ( 'NONE', #36523, 6.000000000000005329 ) ;
#2371 = CARTESIAN_POINT ( 'NONE',  ( 4.902329457098593579, -28.42639230875254341, 7.779495906702013741 ) ) ;
#2372 = CARTESIAN_POINT ( 'NONE',  ( 14.72861853083255035, -4.938210908769336882, -2.501287736049143895 ) ) ;
#2373 = CARTESIAN_POINT ( 'NONE',  ( 22.25801210972482380, 1.411373041331142941, -6.101462656651117200 ) ) ;
#2374 = CARTESIAN_POINT ( 'NONE',  ( -0.5254690805390769270, -26.86890242742082080, 6.894806418505347700 ) ) ;
#2375 = ORIENTED_EDGE ( 'NONE', *, *, #4167, .F. ) ;
#2376 = CARTESIAN_POINT ( 'NONE',  ( 0.09894228122565373873, -26.45779829264445482, 7.013842709614101167 ) ) ;
#2377 = CARTESIAN_POINT ( 'NONE',  ( 69.97231107847817100, 58.54512925548123548, -3.931953536312680964 ) ) ;
#2378 = VERTEX_POINT ( 'NONE', #25159 ) ;
#2379 = CARTESIAN_POINT ( 'NONE',  ( 86.14505873727070195, -0.01797735283943463491, 5.995667628870159582 ) ) ;
#2380 = CARTESIAN_POINT ( 'NONE',  ( 0.1190537080039397733, -26.56003401220450755, 6.865312560952603782 ) ) ;
#2381 = CARTESIAN_POINT ( 'NONE',  ( 21.58862418887968460, 7.202556094215188054, 2.923978954502209682 ) ) ;
#2383 = CARTESIAN_POINT ( 'NONE',  ( 1.212546478539324957, -26.20509443716330722, 6.864651958020304257 ) ) ;
#2382 = CARTESIAN_POINT ( 'NONE',  ( -0.8913790868336790574, -27.21773604496269527, 6.870724624169666228 ) ) ;
#2384 = ITEM_DEFINED_TRANSFORMATION ( 'NONE', 'NONE', #1184,  #30744 ) ;
#2385 = CARTESIAN_POINT ( 'NONE',  ( -60.81661347076554591, 25.20155461598436375, -9.800414904976365804 ) ) ;
#2386 = ORIENTED_EDGE ( 'NONE', *, *, #14915, .F. ) ;
#2387 = CARTESIAN_POINT ( 'NONE',  ( 21.70916979853645756, 6.353179628818696578, 3.184481357965229797 ) ) ;
#2388 = PLANE ( 'NONE',  #22227 ) ;
#2389 = CIRCLE ( 'NONE', #35879, 2.500000000000002220 ) ;
#2390 = VECTOR ( 'NONE', #23325, 1000.000000000000114 ) ;
#2391 = VERTEX_POINT ( 'NONE', #27826 ) ;
#2392 = CARTESIAN_POINT ( 'NONE',  ( 80.15282788578683437, 62.77883523856217352, -3.578491385641961120 ) ) ;
#2393 = CARTESIAN_POINT ( 'NONE',  ( 16.14085281723246013, 12.58767971060109758, -2.499999999999998668 ) ) ;
#2394 = CARTESIAN_POINT ( 'NONE',  ( 81.62235710223383478, 64.17388774702364174, -3.017922835037758489 ) ) ;
#2395 = CARTESIAN_POINT ( 'NONE',  ( 78.57218090866955151, 65.76747258267620566, 2.123311106147464322 ) ) ;
#2396 = EDGE_CURVE ( 'NONE', #39470, #16748, #16094, .T. ) ;
#2397 = VECTOR ( 'NONE', #32821, 1000.000000000000000 ) ;
#2398 = FACE_OUTER_BOUND ( 'NONE', #17268, .T. ) ;
#2399 = ADVANCED_FACE ( 'NONE', ( #22292 ), #37301, .T. ) ;
#2400 = B_SPLINE_CURVE_WITH_KNOTS ( 'NONE', 3,
 ( #35693, #20221, #17122, #4783, #29896, #14241, #11145, #23714, #17514, #30110, #1919, #14845, #30729, #39769, #15464, #2534, #36679, #11745, #8461, #9281, #24114, #33617, #33817, #30933, #2947, #30514, #6213, #24530 ),
 .UNSPECIFIED., .F., .F.,
 ( 4, 2, 2, 2, 2, 2, 2, 2, 2, 2, 2, 2, 2, 4 ),
 ( 2.168404344971008868E-19, 0.0002510493512354818220, 0.0005020987024709634271, 0.001004197404941950707, 0.002008394809883904883, 0.003012592214825858192, 0.004016789619767812368, 0.006025184429651660872, 0.008033579239535510244, 0.01205036885930323327, 0.01405876366918711907, 0.01506296107412906024, 0.01556505977660003169, 0.01606715847907100314 ),
 .UNSPECIFIED. ) ;
#2401 = LINE ( 'NONE', #2187, #2524 ) ;
#2402 = CARTESIAN_POINT ( 'NONE',  ( 21.85643539959774273, 10.50077279934518160, -1.805501455388072385 ) ) ;
#2403 = ORIENTED_EDGE ( 'NONE', *, *, #33054, .F. ) ;
#2404 = CARTESIAN_POINT ( 'NONE',  ( -77.68413004431236857, 11.14508354151945113, 7.383713242483813666 ) ) ;
#2405 = CARTESIAN_POINT ( 'NONE',  ( -17.69482985384422236, -39.37473357531881391, 6.000000000000000000 ) ) ;
#2406 = EDGE_CURVE ( 'NONE', #25329, #39282, #6226, .T. ) ;
#2407 = CARTESIAN_POINT ( 'NONE',  ( -0.1576164094376339420, -32.53604074034053895, 7.750000000000000888 ) ) ;
#2408 = EDGE_CURVE ( 'NONE', #3093, #24473, #34891, .T. ) ;
#2409 = CARTESIAN_POINT ( 'NONE',  ( -78.64083763406480898, 10.18485694350484927, -8.124114778902974621 ) ) ;
#2410 = DIRECTION ( 'NONE',  ( 0.000000000000000000, 1.000000000000000000, 0.000000000000000000 ) ) ;
#2411 = CARTESIAN_POINT ( 'NONE',  ( 2.486219537498463694, -26.26198458709621164, 6.911401339314955372 ) ) ;
#2412 = CARTESIAN_POINT ( 'NONE',  ( -1.761252033055642707, -30.06883868682544758, 7.766640943994345569 ) ) ;
#2413 = CARTESIAN_POINT ( 'NONE',  ( 14.73716873398060478, 12.66775802014586105, 2.506489619347135545 ) ) ;
#2414 = DIRECTION ( 'NONE',  ( 0.9848077530122080203, 0.1736481776669307198, -0.000000000000000000 ) ) ;
#2415 = DIRECTION ( 'NONE',  ( 1.000000000000000000, 0.000000000000000000, 0.000000000000000000 ) ) ;
#2416 = DIRECTION ( 'NONE',  ( 0.000000000000000000, 0.000000000000000000, 1.000000000000000000 ) ) ;
#2417 = CARTESIAN_POINT ( 'NONE',  ( 3.905425806387133214, -32.15794714433188517, 7.652160403243384756 ) ) ;
#2418 = CARTESIAN_POINT ( 'NONE',  ( -70.92837670882107659, 13.87661300689599386, 6.000000000000002665 ) ) ;
#2419 = CARTESIAN_POINT ( 'NONE',  ( 24.61164019132730374, 2.699834716109671184, -3.894731277034012340 ) ) ;
#2420 = ORIENTED_EDGE ( 'NONE', *, *, #24147, .F. ) ;
#2421 =( BOUNDED_CURVE ( )  B_SPLINE_CURVE ( 3, ( #4834, #24177, #33044, #1972 ),
 .UNSPECIFIED., .F., .T. ) 
 B_SPLINE_CURVE_WITH_KNOTS ( ( 4, 4 ),
 ( 4.708531083176467291, 4.895802057644187855 ),
 .UNSPECIFIED. ) 
 CURVE ( )  GEOMETRIC_REPRESENTATION_ITEM ( )  RATIONAL_B_SPLINE_CURVE ( ( 1.000000000000000000, 0.9970795998553221295, 0.9970795998553221295, 1.000000000000000000 ) ) 
 REPRESENTATION_ITEM ( '' )  );
#2422 = CARTESIAN_POINT ( 'NONE',  ( 0.5045334820826082867, -26.37958808575769609, 7.257242401810563237 ) ) ;
#2423=STYLED_ITEM('',(#40738),#39057);
#2424 = CARTESIAN_POINT ( 'NONE',  ( 67.83896914621323049, 57.99724189137371155, 3.982857479566772607 ) ) ;
#2425 = CARTESIAN_POINT ( 'NONE',  ( 37.05753485607799291, -2.899691229771081069, 5.990122572795006484 ) ) ;
#2426 = CARTESIAN_POINT ( 'NONE',  ( -1.666358850447297923, -30.04427921204255014, 7.759451378593096749 ) ) ;
#2427 = PLANE ( 'NONE',  #3026 ) ;
#2428 = CARTESIAN_POINT ( 'NONE',  ( 88.82472656415403378, -2.095778867207653828, 0.2190179053162402134 ) ) ;
#2430 = CARTESIAN_POINT ( 'NONE',  ( 4.846488009122917440, -30.85918098452591707, 6.865312560952602894 ) ) ;
#2429 = DIRECTION ( 'NONE',  ( -0.000000000000000000, -0.000000000000000000, 1.000000000000000000 ) ) ;
#2431 = VERTEX_POINT ( 'NONE', #31142 ) ;
#2432 = CARTESIAN_POINT ( 'NONE',  ( 1.578585683582428345, -33.06757917596850405, 7.754798119455333705 ) ) ;
#2433 = CARTESIAN_POINT ( 'NONE',  ( 85.57577930415899914, 1.015208198401525541, 5.782835925834406865 ) ) ;
#2434 = CARTESIAN_POINT ( 'NONE',  ( -69.08758708074093136, 24.84364830758653397, 3.800414904976363140 ) ) ;
#2435 = ORIENTED_EDGE ( 'NONE', *, *, #24869, .F. ) ;
#2436 = CARTESIAN_POINT ( 'NONE',  ( -70.30712919725708332, -21.57437711518543111, 5.980324962551068602 ) ) ;
#2437 = PRODUCT_DEFINITION_CONTEXT ( 'detailed design', #18152, 'design' ) ;
#2438 = ORIENTED_EDGE ( 'NONE', *, *, #17073, .F. ) ;
#2439 = EDGE_LOOP ( 'NONE', ( #15197, #32066, #23804, #27519 ) ) ;
#2440 = CARTESIAN_POINT ( 'NONE',  ( 79.20065834867790500, 65.31285345095534467, -3.018898740118490576 ) ) ;
#2441 = CARTESIAN_POINT ( 'NONE',  ( -1.534565338722829964, -28.23383362140880948, 6.877402575842993748 ) ) ;
#2442 = CARTESIAN_POINT ( 'NONE',  ( 78.70885197775000108, 65.89012877898849752, 1.994058748902171940 ) ) ;
#2443 = CARTESIAN_POINT ( 'NONE',  ( 22.37141982511144889, 0.3128190655527079977, 6.946763763332127972 ) ) ;
#2445 = ORIENTED_EDGE ( 'NONE', *, *, #4755, .F. ) ;
#2444 = CARTESIAN_POINT ( 'NONE',  ( -68.71186372058383540, 37.81212149306784909, 9.800414904976364028 ) ) ;
#2446 = CARTESIAN_POINT ( 'NONE',  ( 73.92749824250802249, 61.95374747488791201, -3.708893976703420137 ) ) ;
#2447 = CARTESIAN_POINT ( 'NONE',  ( 3.355851366112005518, -32.53968674081319534, 6.892063359921934307 ) ) ;
#2449 = CARTESIAN_POINT ( 'NONE',  ( 25.88590780377253964, -5.105876911915265381, 3.183034662934932868 ) ) ;
#2448 = CARTESIAN_POINT ( 'NONE',  ( 4.959554532356096779, -30.84580132059966573, 6.865554069792298542 ) ) ;
#2450 = DIRECTION ( 'NONE',  ( 1.000000000000000000, 0.000000000000000000, 0.000000000000000000 ) ) ;
#2451 = AXIS2_PLACEMENT_3D ( 'NONE', #38153, #18603, #31188 ) ;
#2452 = CIRCLE ( 'NONE', #7688, 0.1000000000000028644 ) ;
#2453 = CARTESIAN_POINT ( 'NONE',  ( 23.42389927133387317, 3.726266061901138738, -3.241371881706822222 ) ) ;
#2454 = EDGE_LOOP ( 'NONE', ( #3913, #20566, #18074, #14726 ) ) ;
#2455 = DIRECTION ( 'NONE',  ( -0.000000000000000000, -0.000000000000000000, 1.000000000000000000 ) ) ;
#2456 = CIRCLE ( 'NONE', #12296, 95.38357402481355507 ) ;
#2457 = EDGE_CURVE ( 'NONE', #4993, #21312, #12183, .T. ) ;
#2458 = CARTESIAN_POINT ( 'NONE',  ( 24.33259761278756272, 0.1721304915443387373, 6.926443425830641765 ) ) ;
#2459 = EDGE_CURVE ( 'NONE', #32758, #699, #21468, .T. ) ;
#2460 = CARTESIAN_POINT ( 'NONE',  ( 2.868207633511080434, -32.86935470785505231, 6.894806418505347700 ) ) ;
#2461 = CARTESIAN_POINT ( 'NONE',  ( 3.848298546108438245, -32.20554951821143419, 6.894806418505343260 ) ) ;
#2462 = CARTESIAN_POINT ( 'NONE',  ( 79.48860182481728032, 65.82309781974731777, 2.578835243349295148 ) ) ;
#2463 = CARTESIAN_POINT ( 'NONE',  ( 87.68748590470411841, -1.878626560869070872, 3.708385665356400906 ) ) ;
#2464 = CARTESIAN_POINT ( 'NONE',  ( -70.92837670882107659, -37.87473357531881391, 0.000000000000000000 ) ) ;
#2465 = ORIENTED_EDGE ( 'NONE', *, *, #16374, .T. ) ;
#2466 = DIRECTION ( 'NONE',  ( 0.000000000000000000, 0.000000000000000000, 1.000000000000000000 ) ) ;
#2467 = PLANE ( 'NONE',  #8 ) ;
#2468 = CARTESIAN_POINT ( 'NONE',  ( 14.79422032056577052, -5.583071962950631573, -2.503592320680073424 ) ) ;
#2469 = CARTESIAN_POINT ( 'NONE',  ( 29.09904249065658277, 0.3518783346174893523, -4.748007362305766144 ) ) ;
#2470 = CYLINDRICAL_SURFACE ( 'NONE', #25330, 0.09010775117053081151 ) ;
#2471 = FACE_OUTER_BOUND ( 'NONE', #39837, .T. ) ;
#2472 = ORIENTED_EDGE ( 'NONE', *, *, #17443, .T. ) ;
#2473 = CARTESIAN_POINT ( 'NONE',  ( 2.805807153542528187, -32.88323007867923309, 7.776484688137380807 ) ) ;
#2474 = CARTESIAN_POINT ( 'NONE',  ( 86.56125476490799997, 1.128014799767447229, 4.962829853851403961 ) ) ;
#2475 = EDGE_LOOP ( 'NONE', ( #24880, #22470, #13430, #38232 ) ) ;
#2476 = ORIENTED_EDGE ( 'NONE', *, *, #32019, .T. ) ;
#2478 = CARTESIAN_POINT ( 'NONE',  ( 36.20144388887960218, -3.653144936024889322, 5.716525466092109653 ) ) ;
#2477 = CARTESIAN_POINT ( 'NONE',  ( 79.73516162904324744, 65.38506083608318420, -3.083955809406671467 ) ) ;
#2479 = CARTESIAN_POINT ( 'NONE',  ( 22.73643742276861346, -2.655319355651748925, 3.754968961276796247 ) ) ;
#2480 = CARTESIAN_POINT ( 'NONE',  ( 3.481437286441587453, -32.58288071328335178, 7.686927408461905031 ) ) ;
#2481 = VECTOR ( 'NONE', #30760, 1000.000000000000000 ) ;
#2482 = CARTESIAN_POINT ( 'NONE',  ( 4.667181775993622495, -31.24519220632647887, 7.257242401810564125 ) ) ;
#2483 = VECTOR ( 'NONE', #26320, 1000.000000000000000 ) ;
#2484 = EDGE_LOOP ( 'NONE', ( #3436, #28923, #6825, #34739 ) ) ;
#2485 = DIRECTION ( 'NONE',  ( 1.000000000000000000, -0.000000000000000000, 0.000000000000000000 ) ) ;
#2486 = ORIENTED_EDGE ( 'NONE', *, *, #18879, .T. ) ;
#2487 = ORIENTED_EDGE ( 'NONE', *, *, #24774, .T. ) ;
#2488 = PLANE ( 'NONE',  #30568 ) ;
#2489 = CARTESIAN_POINT ( 'NONE',  ( 80.51591231855056208, 63.60920045316173344, -3.640670270625564253 ) ) ;
#2490 = CARTESIAN_POINT ( 'NONE',  ( -58.69259491913187787, 29.82092612118092489, -5.479210374447095688 ) ) ;
#2492 = CARTESIAN_POINT ( 'NONE',  ( 31.33775714179567373, 0.5243197422169587618, 4.587784402887622903 ) ) ;
#2491 = CARTESIAN_POINT ( 'NONE',  ( 22.96819900907483358, 2.437540201623891623, 4.628877954886912782 ) ) ;
#2493 = ORIENTED_EDGE ( 'NONE', *, *, #16858, .T. ) ;
#2494 = CARTESIAN_POINT ( 'NONE',  ( 81.93064166251112113, 62.10341262211372992, -1.859759604986998882 ) ) ;
#2495 = CARTESIAN_POINT ( 'NONE',  ( 5.401390093233090717, -29.51577928193538369, 7.695279973900954751 ) ) ;
#2496 = CARTESIAN_POINT ( 'NONE',  ( -71.45033707005815415, -21.67496598542010489, 3.980161455544446891 ) ) ;
#2498 = CARTESIAN_POINT ( 'NONE',  ( 22.18386873814171878, -2.652701146302887558, -3.668727254116632253 ) ) ;
#2497 = CARTESIAN_POINT ( 'NONE',  ( -30.97867591359219119, -24.55319635012989110, 6.700000000000000178 ) ) ;
#2499 = CARTESIAN_POINT ( 'NONE',  ( -1.795329325813683541, -29.39687274210862711, 7.009310105710486738 ) ) ;
#2500 = CARTESIAN_POINT ( 'NONE',  ( 73.18282872914367942, 62.10277071170013841, 3.478821770299028948 ) ) ;
#2501 = CARTESIAN_POINT ( 'NONE',  ( 23.03775345957872389, 3.287047143578627484, -3.951504299623971317 ) ) ;
#2502 = ORIENTED_EDGE ( 'NONE', *, *, #20115, .F. ) ;
#2503 = AXIS2_PLACEMENT_3D ( 'NONE', #38822, #35761, #7535 ) ;
#2504 = CARTESIAN_POINT ( 'NONE',  ( 21.85643539959777115, 4.792808800112425160, -12.41435969090265523 ) ) ;
#2506 = EDGE_CURVE ( 'NONE', #6019, #35491, #30780, .T. ) ;
#2505 = DIRECTION ( 'NONE',  ( 1.000000000000000000, 0.000000000000000000, 0.000000000000000000 ) ) ;
#2507 = VERTEX_POINT ( 'NONE', #466 ) ;
#2508 = DIRECTION ( 'NONE',  ( -0.9396926207859007674, 0.3420201433256899737, 0.000000000000000000 ) ) ;
#2509 = CARTESIAN_POINT ( 'NONE',  ( 81.16598293928451824, 61.30266375757629049, 1.057717897339646163 ) ) ;
#2510 = CARTESIAN_POINT ( 'NONE',  ( 86.42578330747443260, 1.280182770620154953, -5.202446006352976937 ) ) ;
#2511 = CARTESIAN_POINT ( 'NONE',  ( 5.135506051709807451, -30.24079465769465358, 6.870737987065013819 ) ) ;
#2512 = AXIS2_PLACEMENT_3D ( 'NONE', #3061, #34548, #38005 ) ;
#2513 = CARTESIAN_POINT ( 'NONE',  ( 2.716088600019323618, -32.91931299483255202, 6.971170733404099984 ) ) ;
#2514 = CARTESIAN_POINT ( 'NONE',  ( 14.84236729553075129, -4.537698572362919514, 2.514786686759733048 ) ) ;
#2515 = CARTESIAN_POINT ( 'NONE',  ( 21.54943548333990577, 7.328808947467964963, 1.955308278464419347 ) ) ;
#2516 = CARTESIAN_POINT ( 'NONE',  ( 34.33397697960574391, -1.483043513302994443, -5.565045496675192993 ) ) ;
#2517 = DIRECTION ( 'NONE',  ( 0.000000000000000000, 0.000000000000000000, -1.000000000000000000 ) ) ;
#2518 = CARTESIAN_POINT ( 'NONE',  ( 5.197301300333582397, -29.56993018336890700, 7.767301406056524193 ) ) ;
#2519 = FACE_OUTER_BOUND ( 'NONE', #33487, .T. ) ;
#2520 = DIRECTION ( 'NONE',  ( 0.000000000000000000, 0.000000000000000000, 1.000000000000000000 ) ) ;
#2521 = CARTESIAN_POINT ( 'NONE',  ( 1.728381123661779206, -33.06982220562891683, 7.733670252284492008 ) ) ;
#2522 = ORIENTED_EDGE ( 'NONE', *, *, #25016, .F. ) ;
#2523 = CARTESIAN_POINT ( 'NONE',  ( 36.99646211313889665, -3.220648697242111780, 5.952655130425513974 ) ) ;
#2524 = VECTOR ( 'NONE', #17586, 1000.000000000000000 ) ;
#2525 = CARTESIAN_POINT ( 'NONE',  ( -11.81496944966682960, -21.25669541281728669, -1.000000000000000000 ) ) ;
#2526 = EDGE_CURVE ( 'NONE', #5538, #38785, #4624, .T. ) ;
#2527 = CARTESIAN_POINT ( 'NONE',  ( 67.00300875778714271, 58.01168839481970707, -3.999354069328931782 ) ) ;
#2528 = CARTESIAN_POINT ( 'NONE',  ( 1.700390093233090871, -29.56993018339339940, 7.750000000000000888 ) ) ;
#2529 = DIRECTION ( 'NONE',  ( 0.000000000000000000, 0.000000000000000000, 1.000000000000000000 ) ) ;
#2530 = AXIS2_PLACEMENT_3D ( 'NONE', #10971, #23551, #33449 ) ;
#2531 = ORIENTED_EDGE ( 'NONE', *, *, #15578, .T. ) ;
#2532 = CARTESIAN_POINT ( 'NONE',  ( -0.5234024681467984719, -32.14186482873412842, 7.785868773668302545 ) ) ;
#2533 = CARTESIAN_POINT ( 'NONE',  ( -77.20907466686004739, -6.116245841690640894, -7.791481786428602341 ) ) ;
#2534 = CARTESIAN_POINT ( 'NONE',  ( 73.85944157702037671, 62.69931772841422202, 3.253003066526747755 ) ) ;
#2535 = CARTESIAN_POINT ( 'NONE',  ( 1.751251297819361730, -26.64985754041175525, 6.800000000000000711 ) ) ;
#2536 = CARTESIAN_POINT ( 'NONE',  ( 5.029344116975409840, -28.48940719755995588, 7.753200566781599079 ) ) ;
#2537 = VERTEX_POINT ( 'NONE', #34449 ) ;
#2538 = CARTESIAN_POINT ( 'NONE',  ( 22.63321249055432816, 4.548868538501633196, 3.119291088745934637 ) ) ;
#2539 = CARTESIAN_POINT ( 'NONE',  ( 79.68852728668518637, 66.33522678087791746, -1.065376284871803803 ) ) ;
#2540 = EDGE_CURVE ( 'NONE', #21166, #26423, #18557, .T. ) ;
#2541 = CARTESIAN_POINT ( 'NONE',  ( 80.56654867478538051, 63.26449302893301052, 3.600689860192759717 ) ) ;
#2542 = DIRECTION ( 'NONE',  ( 1.000000000000000000, 0.000000000000000000, 0.000000000000000000 ) ) ;
#2543 = ORIENTED_EDGE ( 'NONE', *, *, #24789, .T. ) ;
#2544 = CARTESIAN_POINT ( 'NONE',  ( 78.51266523469813308, 61.01400193535545213, -3.220231295875733757 ) ) ;
#2546 = CARTESIAN_POINT ( 'NONE',  ( 14.75858788393853160, -5.151706771557507558, -2.499999999916640014 ) ) ;
#2545 = CARTESIAN_POINT ( 'NONE',  ( 27.44076331759783116, 0.9565809941908112179, 4.489197854688308453 ) ) ;
#2547 = CARTESIAN_POINT ( 'NONE',  ( 81.47459903045408680, 62.11139297693658534, -2.556731990913030828 ) ) ;
#2548 = CARTESIAN_POINT ( 'NONE',  ( 5.051054751933684805, -30.14703185982037681, 7.635761828346577573 ) ) ;
#2549 = CARTESIAN_POINT ( 'NONE',  ( 79.57681890279650361, 60.99726435378330081, 2.643019404357117352 ) ) ;
#2550 = ORIENTED_EDGE ( 'NONE', *, *, #23247, .T. ) ;
#2551 = ORIENTED_EDGE ( 'NONE', *, *, #18908, .T. ) ;
#2552 = DIRECTION ( 'NONE',  ( 1.000000000000000000, 0.000000000000000000, 0.000000000000000000 ) ) ;
#2553 = EDGE_CURVE ( 'NONE', #3797, #27685, #19466, .T. ) ;
#2554 = CARTESIAN_POINT ( 'NONE',  ( 81.46991160412491695, 61.46693516840312554, 1.070820504726896827 ) ) ;
#2556 = CARTESIAN_POINT ( 'NONE',  ( -80.92837670882107659, 2.429809908903242555, -12.50000000000000000 ) ) ;
#2555 = LINE ( 'NONE', #37703, #38851 ) ;
#2557 = AXIS2_PLACEMENT_3D ( 'NONE', #15181, #27740, #40293 ) ;
#2558 = CARTESIAN_POINT ( 'NONE',  ( 27.86875652909539980, 2.635651561731235493, 0.006556038081918813022 ) ) ;
#2559 = CARTESIAN_POINT ( 'NONE',  ( 14.73423124852490318, -5.107548947968362008, -2.500000000000001776 ) ) ;
#2560 = CARTESIAN_POINT ( 'NONE',  ( -1.333134932519906446, -31.10541900397473825, 7.013842709614101167 ) ) ;
#2561 = CARTESIAN_POINT ( 'NONE',  ( -81.58016648964061801, -5.624404198090563689, 2.451861983733245598 ) ) ;
#2562 = CARTESIAN_POINT ( 'NONE',  ( 21.99020519201814849, 0.2365064862963604797, -7.678606242944151283 ) ) ;
#2563 = LINE ( 'NONE', #40201, #30748 ) ;
#2564 = ORIENTED_EDGE ( 'NONE', *, *, #16447, .T. ) ;
#2565 = DIRECTION ( 'NONE',  ( 0.6427876096865369204, 0.7660444431189800119, 0.000000000000000000 ) ) ;
#2566 = CARTESIAN_POINT ( 'NONE',  ( 80.01459546602684725, 60.89228396117896835, 2.037903991281934335 ) ) ;
#2567 = CARTESIAN_POINT ( 'NONE',  ( 5.153279172109078488, -30.14225614731512337, 7.695279973900954751 ) ) ;
#2568 = CARTESIAN_POINT ( 'NONE',  ( 33.44571278339331144, -3.711821305012397598, -5.220872097300803816 ) ) ;
#2569 = CARTESIAN_POINT ( 'NONE',  ( -61.24591834330252027, -49.47158280949359010, 2.500000000000000000 ) ) ;
#2570 = DIRECTION ( 'NONE',  ( 0.000000000000000000, 0.000000000000000000, 1.000000000000000000 ) ) ;
#2571 = CARTESIAN_POINT ( 'NONE',  ( -0.08061302505832330934, -26.55695359817150347, 7.698786668945011513 ) ) ;
#2572 = DIRECTION ( 'NONE',  ( 0.5000000000000101030, -0.8660254037844328234, -0.000000000000000000 ) ) ;
#2573 = DIRECTION ( 'NONE',  ( -0.000000000000000000, -1.000000000000000000, -0.000000000000000000 ) ) ;
#2574 = CARTESIAN_POINT ( 'NONE',  ( 4.631989694572121508, -27.84779834644859875, 7.652160403243386533 ) ) ;
#2575 = CARTESIAN_POINT ( 'NONE',  ( 4.999814617694763541, -28.40211264311544070, 6.894806418505347700 ) ) ;
#2576 = CIRCLE ( 'NONE', #38044, 4.357836081054403010 ) ;
#2577 = ADVANCED_FACE ( 'NONE', ( #3172 ), #15687, .T. ) ;
#2578 = CARTESIAN_POINT ( 'NONE',  ( 20.95047569564395573, 9.633251686941981973, 2.522532965598568211 ) ) ;
#2579 = CARTESIAN_POINT ( 'NONE',  ( 22.53785975336948155, 1.420150480624714273, -5.804402300735387321 ) ) ;
#2580 = EDGE_CURVE ( 'NONE', #29188, #40280, #39417, .T. ) ;
#2581 = VERTEX_POINT ( 'NONE', #12796 ) ;
#2582 = FILL_AREA_STYLE_COLOUR ( '', #898 ) ;
#2583 = CARTESIAN_POINT ( 'NONE',  ( 69.48201546320520094, 59.78788955577742570, -3.863726395435664873 ) ) ;
#2584 = VERTEX_POINT ( 'NONE', #63 ) ;
#2585 = CARTESIAN_POINT ( 'NONE',  ( 86.53727031679849802, -0.6854317443871157378, -5.678301933988063155 ) ) ;
#2586 = VECTOR ( 'NONE', #39592, 1000.000000000000000 ) ;
#2587 = LINE ( 'NONE', #15923, #15386 ) ;
#2588 = CARTESIAN_POINT ( 'NONE',  ( 70.04419837359742473, 58.36171959603688464, 3.883859131414874710 ) ) ;
#2589 = CARTESIAN_POINT ( 'NONE',  ( 4.999814617694763541, -28.40211264311544070, 6.894806418505347700 ) ) ;
#2590 = ADVANCED_FACE ( 'NONE', ( #9502 ), #22085, .T. ) ;
#2591 = ADVANCED_FACE ( 'NONE', ( #15889 ), #28448, .F. ) ;
#2592 = CARTESIAN_POINT ( 'NONE',  ( -75.45330471031414277, 33.71485196875532608, 8.800414904976364028 ) ) ;
#2593 = ITEM_DEFINED_TRANSFORMATION ( 'NONE', 'NONE', #15617,  #30744 ) ;
#2594 = CARTESIAN_POINT ( 'NONE',  ( -75.45330471031414277, 33.71485196875532608, -46.17089178453873188 ) ) ;
#2595 = VERTEX_POINT ( 'NONE', #28110 ) ;
#2596 = EDGE_CURVE ( 'NONE', #17770, #15824, #30395, .T. ) ;
#2597 = CARTESIAN_POINT ( 'NONE',  ( 24.42167434069570930, 3.172085603352147842, 3.233354437090341094 ) ) ;
#2598 =( LENGTH_UNIT ( ) NAMED_UNIT ( * ) SI_UNIT ( .MILLI., .METRE. ) );
#2599 = CARTESIAN_POINT ( 'NONE',  ( 22.15639445573606992, -3.079419702076586329, 3.567612438417096410 ) ) ;
#2600 = ORIENTED_EDGE ( 'NONE', *, *, #26276, .F. ) ;
#2601 = VERTEX_POINT ( 'NONE', #5892 ) ;
#2602 = CARTESIAN_POINT ( 'NONE',  ( 80.39157904934594967, 62.27158585385627987, -3.322373183921394801 ) ) ;
#2603 = DIRECTION ( 'NONE',  ( -0.000000000000000000, -0.000000000000000000, -1.000000000000000000 ) ) ;
#2604 = CARTESIAN_POINT ( 'NONE',  ( 81.86163085503896752, 62.85586669281862982, -2.670779692148389728 ) ) ;
#2605 = CARTESIAN_POINT ( 'NONE',  ( 79.79522905248630593, 63.61080392591205168, 3.730195463674649492 ) ) ;
#2606 = ORIENTED_EDGE ( 'NONE', *, *, #8684, .T. ) ;
#2607 = CARTESIAN_POINT ( 'NONE',  ( 4.370501521683438639, -27.46502734687952341, 6.864651958020305145 ) ) ;
#2608 = DIRECTION ( 'NONE',  ( -0.000000000000000000, -1.000000000000000000, -0.000000000000000000 ) ) ;
#2609 = CARTESIAN_POINT ( 'NONE',  ( 21.85643539959776760, 6.468309080218945795, -8.875946301973074881 ) ) ;
#2610 = ORIENTED_EDGE ( 'NONE', *, *, #24418, .T. ) ;
#2611 = DIRECTION ( 'NONE',  ( 0.000000000000000000, 0.000000000000000000, 1.000000000000000000 ) ) ;
#2612 = CYLINDRICAL_SURFACE ( 'NONE', #25913, 0.09010775117053089478 ) ;
#2613 = CARTESIAN_POINT ( 'NONE',  ( -69.08758708074093136, 37.96445039004638033, -9.800414904976365804 ) ) ;
#2614 = CARTESIAN_POINT ( 'NONE',  ( -72.63917791570506211, 6.521876929970503056, -9.854674157099612586 ) ) ;
#2615 = CARTESIAN_POINT ( 'NONE',  ( 29.48920755849628605, -3.189424998377129228, -4.808902057303421351 ) ) ;
#2616 = CARTESIAN_POINT ( 'NONE',  ( 36.13397042527238057, -1.528216537091738214, -5.641571063127631014 ) ) ;
#2617 = CARTESIAN_POINT ( 'NONE',  ( -70.92837670882107659, -31.30579396504363388, 0.000000000000000000 ) ) ;
#2618 = CARTESIAN_POINT ( 'NONE',  ( 15.49758433003794877, 11.04722695288106671, 2.625170863832550605 ) ) ;
#2619 = CARTESIAN_POINT ( 'NONE',  ( -77.92837670882107659, 2.429809908903242999, 12.50000000000000000 ) ) ;
#2620 = CARTESIAN_POINT ( 'NONE',  ( -67.52519766902113929, 36.12526529565825939, -8.800414904976360475 ) ) ;
#2621 = CARTESIAN_POINT ( 'NONE',  ( -6.878675913592188884, -26.64985754041175525, 6.700000000000000178 ) ) ;
#2622 = EDGE_CURVE ( 'NONE', #23841, #33142, #10877, .T. ) ;
#2623 = CARTESIAN_POINT ( 'NONE',  ( 19.92985266052819782, 11.61392316146510240, -2.499999999999999556 ) ) ;
#2624 = CARTESIAN_POINT ( 'NONE',  ( 37.18189302406424446, -2.607975392620101474, -5.985526701086073764 ) ) ;
#2625 = CARTESIAN_POINT ( 'NONE',  ( 24.88192582561759636, 2.551848270425359555, -3.964384284743410092 ) ) ;
#2626 = ORIENTED_EDGE ( 'NONE', *, *, #34903, .T. ) ;
#2627 = CARTESIAN_POINT ( 'NONE',  ( 67.08333554474984339, 58.24655189615426565, 3.990981480864018938 ) ) ;
#2628 = CARTESIAN_POINT ( 'NONE',  ( 36.68763091036087332, -2.387583900041891027, 5.932390115904950356 ) ) ;
#2629 = CARTESIAN_POINT ( 'NONE',  ( -1.661009635141104557, -30.08088777829730986, 7.782034975670476307 ) ) ;
#2630 = EDGE_CURVE ( 'NONE', #2431, #25345, #244, .T. ) ;
#2631 = AXIS2_PLACEMENT_3D ( 'NONE', #35079, #25792, #32188 ) ;
#2632 = CARTESIAN_POINT ( 'NONE',  ( -0.7779991009897547771, -25.20532047864482905, 7.695279973900954751 ) ) ;
#2634 = ADVANCED_FACE ( 'NONE', ( #40252 ), #27292, .F. ) ;
#2633 = CARTESIAN_POINT ( 'NONE',  ( 86.85482141032015591, 0.6757441427909987031, 5.750446197363288547 ) ) ;
#2636 = CARTESIAN_POINT ( 'NONE',  ( 37.01725082149712875, -2.757042412250769292, -5.983835274925594305 ) ) ;
#2635 = FACE_OUTER_BOUND ( 'NONE', #28603, .T. ) ;
#2637 = PRODUCT_DEFINITION_SHAPE ( 'NONE', 'NONE',  #40724 ) ;
#2638 = ORIENTED_EDGE ( 'NONE', *, *, #3054, .F. ) ;
#2639 = DIRECTION ( 'NONE',  ( -0.000000000000000000, -0.000000000000000000, 1.000000000000000000 ) ) ;
#2640 = CARTESIAN_POINT ( 'NONE',  ( -24.24874870218063450, -26.64985754041175525, 6.700000000000000178 ) ) ;
#2641 = EDGE_CURVE ( 'NONE', #20325, #9389, #7639, .T. ) ;
#2642 = EDGE_LOOP ( 'NONE', ( #34392, #28768, #2335, #15418, #11291, #197, #25108 ) ) ;
#2643 = CARTESIAN_POINT ( 'NONE',  ( -31.07867591359219617, -26.64985754041175525, 6.800000000000000711 ) ) ;
#2644 = AXIS2_PLACEMENT_3D ( 'NONE', #36252, #14213, #20586 ) ;
#2645 = ORIENTED_EDGE ( 'NONE', *, *, #17327, .T. ) ;
#2646 = CARTESIAN_POINT ( 'NONE',  ( 79.76446817951413948, 64.32424044856641387, -3.638935937159315515 ) ) ;
#2647 = CARTESIAN_POINT ( 'NONE',  ( -1.517898193795411688, -28.19420277047165513, 6.965379264086543287 ) ) ;
#2648 = CARTESIAN_POINT ( 'NONE',  ( 80.89004220740271478, 62.15918302697193099, 3.003915454719618960 ) ) ;
#2650 = ORIENTED_EDGE ( 'NONE', *, *, #1328, .T. ) ;
#2649 = CARTESIAN_POINT ( 'NONE',  ( -1.799609906766908463, -29.35564777783850232, 7.376841543590335171 ) ) ;
#2651 = CARTESIAN_POINT ( 'NONE',  ( 74.86006972221214539, 59.87270642427902345, -3.642458757454620777 ) ) ;
#2652 = CARTESIAN_POINT ( 'NONE',  ( 3.221468612762000028, -32.61070642268291664, 6.988553391373222290 ) ) ;
#2654 = LINE ( 'NONE', #25067, #28202 ) ;
#2653 = CARTESIAN_POINT ( 'NONE',  ( 4.924757601813157137, -30.93136360911756455, 6.903112506833882556 ) ) ;
#2655 = CARTESIAN_POINT ( 'NONE',  ( 3.435168117181346847, -26.53010312597114506, 7.640616322432100205 ) ) ;
#2656 = DIRECTION ( 'NONE',  ( 0.000000000000000000, 0.000000000000000000, 1.000000000000000000 ) ) ;
#2657 = CARTESIAN_POINT ( 'NONE',  ( 22.01200767717710605, 5.505276828284054069, -3.148064352147821765 ) ) ;
#2658 = VERTEX_POINT ( 'NONE', #30607 ) ;
#2659 = CARTESIAN_POINT ( 'NONE',  ( 4.262268152916126596, -27.17521612592422287, 7.139344958878409919 ) ) ;
#2660 = CIRCLE ( 'NONE', #9179, 0.1000000000000028644 ) ;
#2661 = CARTESIAN_POINT ( 'NONE',  ( 26.66483005201559564, 2.460286195115170216, -3.284910328407702806 ) ) ;
#2662 = CARTESIAN_POINT ( 'NONE',  ( -0.9575113486053222767, -31.84711263666175540, 7.695279973900954751 ) ) ;
#2663 = CARTESIAN_POINT ( 'NONE',  ( -12.44874870218064267, -26.64985754041175525, 6.800000000000000711 ) ) ;
#2664 = CARTESIAN_POINT ( 'NONE',  ( 80.26863108949500258, 64.98620546077047777, 3.307636073424107703 ) ) ;
#2665 = CARTESIAN_POINT ( 'NONE',  ( 87.02687067233559048, -1.029203037998749570, 5.291918051785640564 ) ) ;
#2666 =( BOUNDED_CURVE ( )  B_SPLINE_CURVE ( 3, ( #16614, #29198, #1011, #13545 ),
 .UNSPECIFIED., .F., .T. ) 
 B_SPLINE_CURVE_WITH_KNOTS ( ( 4, 4 ),
 ( 1.570796326794896558, 2.438744940551181184 ),
 .UNSPECIFIED. ) 
 CURVE ( )  GEOMETRIC_REPRESENTATION_ITEM ( )  RATIONAL_B_SPLINE_CURVE ( ( 1.000000000000000000, 0.9382012019593851671, 0.9382012019593851671, 1.000000000000000000 ) ) 
 REPRESENTATION_ITEM ( '' )  );
#2667 = CARTESIAN_POINT ( 'NONE',  ( -2.585338981833881000, -32.18494463595775557, 7.754798119455333705 ) ) ;
#2668 = ORIENTED_EDGE ( 'NONE', *, *, #302, .F. ) ;
#2669 = FACE_OUTER_BOUND ( 'NONE', #24846, .T. ) ;
#2670 = CARTESIAN_POINT ( 'NONE',  ( -32.24874870218063450, -25.49307895267003587, 6.800000000000000711 ) ) ;
#2671 = CARTESIAN_POINT ( 'NONE',  ( 0.1825688514504806015, 0.5999999999999995337, 3.931742364880953744 ) ) ;
#2672 = TOROIDAL_SURFACE ( 'NONE', #9877, 3.449999999999999289, 0.05000000000000000278 ) ;
#2673 = CARTESIAN_POINT ( 'NONE',  ( 14.89421247541311999, -5.922026149921197913, -2.519984706040779621 ) ) ;
#2674 = CARTESIAN_POINT ( 'NONE',  ( 36.64490972802850166, -2.463767798561049549, -5.925722442186287076 ) ) ;
#2675 = DIRECTION ( 'NONE',  ( 0.000000000000000000, 0.000000000000000000, -1.000000000000000000 ) ) ;
#2676 = CARTESIAN_POINT ( 'NONE',  ( -0.3920297796076317454, -26.89004521068930487, 7.757178535559532406 ) ) ;
#2677 = ORIENTED_EDGE ( 'NONE', *, *, #39884, .T. ) ;
#2678 = CARTESIAN_POINT ( 'NONE',  ( 36.91034452848013814, -2.639964513169326565, 5.967149962361803617 ) ) ;
#2679 = CARTESIAN_POINT ( 'NONE',  ( 86.83829259450851623, 0.8168327605515373069, 4.998615091244022146 ) ) ;
#2680 = ORIENTED_EDGE ( 'NONE', *, *, #21939, .F. ) ;
#2681 = ORIENTED_EDGE ( 'NONE', *, *, #18740, .T. ) ;
#2683 = CARTESIAN_POINT ( 'NONE',  ( 37.11018018669391694, -2.403351589215351414, 5.951538865951512491 ) ) ;
#2682 = CARTESIAN_POINT ( 'NONE',  ( 79.37790743583136077, 65.75409067367344562, -2.639511535887587801 ) ) ;
#2684 =( REPRESENTATION_RELATIONSHIP ('NONE','NONE', #24012, #39533 ) REPRESENTATION_RELATIONSHIP_WITH_TRANSFORMATION ( #2384 )SHAPE_REPRESENTATION_RELATIONSHIP( ) );
#2685 = CARTESIAN_POINT ( 'NONE',  ( 18.09051835526576824, -2.859643911663029225, 3.029860928815728549 ) ) ;
#2686 = CARTESIAN_POINT ( 'NONE',  ( 14.62858089720442401, 12.62725169013372550, -2.499999999999999556 ) ) ;
#2687 = PLANE ( 'NONE',  #5345 ) ;
#2688 = EDGE_CURVE ( 'NONE', #30686, #3289, #9189, .T. ) ;
#2689 = ORIENTED_EDGE ( 'NONE', *, *, #24932, .T. ) ;
#2690 = CIRCLE ( 'NONE', #3347, 6.681288188914807691 ) ;
#2691 = CARTESIAN_POINT ( 'NONE',  ( 0.09894228122565373873, -26.45779829264445482, 7.013842709614101167 ) ) ;
#2692 = EDGE_CURVE ( 'NONE', #18497, #35180, #36018, .T. ) ;
#2693 = VERTEX_POINT ( 'NONE', #8956 ) ;
#2694 = ADVANCED_FACE ( 'NONE', ( #40446 ), #2672, .T. ) ;
#2695 = ORIENTED_EDGE ( 'NONE', *, *, #15247, .F. ) ;
#2696 = CARTESIAN_POINT ( 'NONE',  ( 81.09687786842310686, 61.96238702813622723, -2.735335646780895580 ) ) ;
#2697 = CARTESIAN_POINT ( 'NONE',  ( -58.36416262933996535, 28.31210393328041519, -5.221062780410251847 ) ) ;
#2698 = VERTEX_POINT ( 'NONE', #18225 ) ;
#2700 = CARTESIAN_POINT ( 'NONE',  ( 21.46987128311033999, 7.825037809131126565, -2.777605031916560829 ) ) ;
#2699 = CARTESIAN_POINT ( 'NONE',  ( 24.63365376234076010, 2.464256406091844376, 4.030237559253687429 ) ) ;
#2701 = ORIENTED_EDGE ( 'NONE', *, *, #24022, .T. ) ;
#2702 = CARTESIAN_POINT ( 'NONE',  ( 82.08208307362210121, 62.96685751817972232, -2.430878896394279121 ) ) ;
#2703 = LINE ( 'NONE', #40134, #23291 ) ;
#2705 = CARTESIAN_POINT ( 'NONE',  ( -22.24874870218063094, -26.64985754041175525, 6.800000000000000711 ) ) ;
#2704 = CARTESIAN_POINT ( 'NONE',  ( -70.92837670882012446, 0.2170085631207802901, 6.000000000001379341 ) ) ;
#2706 = CARTESIAN_POINT ( 'NONE',  ( 0.8146142450545547087, -34.26560873126469176, 7.013842709614101167 ) ) ;
#2707 = CARTESIAN_POINT ( 'NONE',  ( -64.08758708074093136, 42.21690229090457791, -2.785273623167488388 ) ) ;
#2708 = CARTESIAN_POINT ( 'NONE',  ( 74.14280505202560789, 59.94172787350157705, 3.795548882712136418 ) ) ;
#2709 = CARTESIAN_POINT ( 'NONE',  ( 23.24073689758073513, 3.246734186628089880, -3.866034852107397057 ) ) ;
#2710 = ORIENTED_EDGE ( 'NONE', *, *, #14447, .F. ) ;
#2711 = CARTESIAN_POINT ( 'NONE',  ( 21.85643539959777115, 5.662525507098640887, -13.61651877770312957 ) ) ;
#2712 = CARTESIAN_POINT ( 'NONE',  ( 16.09990961988970426, 15.28674628019742343, -3.774899269766144538 ) ) ;
#2713 = ORIENTED_EDGE ( 'NONE', *, *, #16177, .T. ) ;
#2714 = ORIENTED_EDGE ( 'NONE', *, *, #3312, .F. ) ;
#2715 = CARTESIAN_POINT ( 'NONE',  ( 80.35914242818654429, 65.73759417665652904, 2.670779692148245399 ) ) ;
#2716 = CARTESIAN_POINT ( 'NONE',  ( 88.68641656676298624, -1.259067802340008146, 0.2042187262504959744 ) ) ;
#2717 = DIRECTION ( 'NONE',  ( -0.000000000000000000, -0.000000000000000000, -1.000000000000000000 ) ) ;
#2718 = AXIS2_PLACEMENT_3D ( 'NONE', #26055, #337, #6713 ) ;
#2719 = CARTESIAN_POINT ( 'NONE',  ( -0.9253594976165760988, -27.40996412519702830, 7.670860738520320687 ) ) ;
#2720 = CARTESIAN_POINT ( 'NONE',  ( 31.36708859361117518, -3.142839770289761692, 5.101990809574796337 ) ) ;
#2721 = CARTESIAN_POINT ( 'NONE',  ( -58.99872204295123623, 28.48507918597066180, 6.834244957304007606 ) ) ;
#2722 = CARTESIAN_POINT ( 'NONE',  ( 34.33342975363300553, -1.484566801286986371, -5.564960088827437978 ) ) ;
#2723 = CARTESIAN_POINT ( 'NONE',  ( 5.100370998373280784, -29.55708692423313622, 7.756377446753162097 ) ) ;
#2724 = CARTESIAN_POINT ( 'NONE',  ( 4.639361780851547934, -31.47058591824991680, 6.903112506833880779 ) ) ;
#2725 = FACE_OUTER_BOUND ( 'NONE', #4617, .T. ) ;
#2726 = CARTESIAN_POINT ( 'NONE',  ( 4.200390093233091093, -29.56993018339339940, -8.199999999999999289 ) ) ;
#2727 = CARTESIAN_POINT ( 'NONE',  ( -64.15669616364040451, -60.53509472482660669, 1.328953532546354177 ) ) ;
#2728 = AXIS2_PLACEMENT_3D ( 'NONE', #22101, #24775, #37711 ) ;
#2729 = VERTEX_POINT ( 'NONE', #21541 ) ;
#2730 = CARTESIAN_POINT ( 'NONE',  ( 36.84734063698446249, -2.123997533844214747, 5.880499845153348559 ) ) ;
#2731 = CARTESIAN_POINT ( 'NONE',  ( -71.92837670882107659, -0.7434385580723641418, 3.916079783099621014 ) ) ;
#2732 = CARTESIAN_POINT ( 'NONE',  ( 66.82989622468531365, 58.03237508814455481, -3.998112125426342978 ) ) ;
#2733 = CARTESIAN_POINT ( 'NONE',  ( -0.4535387154642924190, -26.81129727883429581, 7.753200566781576875 ) ) ;
#2734 = LINE ( 'NONE', #30105, #10837 ) ;
#2735 = EDGE_LOOP ( 'NONE', ( #2713, #31186, #38254, #24909 ) ) ;
#2736 = CARTESIAN_POINT ( 'NONE',  ( 88.34928245270404545, -0.8803827640786102693, 0.5788234153557996198 ) ) ;
#2738 = EDGE_CURVE ( 'NONE', #7186, #30246, #32234, .T. ) ;
#2737 = CARTESIAN_POINT ( 'NONE',  ( -73.85267074163550660, -3.621953098407464378, -9.567270356371031070 ) ) ;
#2739 = CARTESIAN_POINT ( 'NONE',  ( 15.23433789938383320, 11.32867894725656477, 2.584084891689991448 ) ) ;
#2740 = VERTEX_POINT ( 'NONE', #32927 ) ;
#2741 = CYLINDRICAL_SURFACE ( 'NONE', #12887, 3.399999999999999911 ) ;
#2742 = DIRECTION ( 'NONE',  ( -1.000000000000000000, 0.000000000000000000, 0.000000000000000000 ) ) ;
#2743 = ORIENTED_EDGE ( 'NONE', *, *, #11848, .T. ) ;
#2744 = CARTESIAN_POINT ( 'NONE',  ( 22.88829950429575533, 4.274613241398780517, 3.138138624598397541 ) ) ;
#2745 = CARTESIAN_POINT ( 'NONE',  ( 81.74784679736075077, 61.69507302169112251, -1.045691535380373960 ) ) ;
#2746 = CARTESIAN_POINT ( 'NONE',  ( 81.14230761098953337, 61.33243076862672183, 1.577285172236835287 ) ) ;
#2747 = CARTESIAN_POINT ( 'NONE',  ( -0.1692143551933917855, -32.40975312335586267, 6.997764925645182821 ) ) ;
#2748 = EDGE_LOOP ( 'NONE', ( #28656, #3105, #29221, #32948, #5854 ) ) ;
#2749 = CARTESIAN_POINT ( 'NONE',  ( 77.74497067125915351, 61.15868661831865438, -3.539370024157715733 ) ) ;
#2751 = CARTESIAN_POINT ( 'NONE',  ( 1.823599949180766178, -26.07217602587316563, 7.753200566781576875 ) ) ;
#2750 = CARTESIAN_POINT ( 'NONE',  ( 2.340111981911837002, -33.01097012869268355, 7.670465701733748531 ) ) ;
#2752 = CARTESIAN_POINT ( 'NONE',  ( 0.5849256341846700291, -26.35810200982117735, 7.785868773668302545 ) ) ;
#2753 = CARTESIAN_POINT ( 'NONE',  ( 81.34501369141619875, 61.50378551383992942, -1.741375869723593706 ) ) ;
#2754 = CARTESIAN_POINT ( 'NONE',  ( 77.88532341798187986, 63.74564772441265603, 3.640295653904954243 ) ) ;
#2755 = CARTESIAN_POINT ( 'NONE',  ( 1.694295730800539301, -26.07130837915405053, 7.762796336881262249 ) ) ;
#2756 = CIRCLE ( 'NONE', #17813, 0.1000000000000028644 ) ;
#2757 = EDGE_LOOP ( 'NONE', ( #4590, #16075, #13154, #2079 ) ) ;
#2758 = CARTESIAN_POINT ( 'NONE',  ( 79.96508732583362189, 66.32411498806379768, 1.465650077276458241 ) ) ;
#2760 = CARTESIAN_POINT ( 'NONE',  ( -1.693160655833844785, -29.36061310642847033, 6.969307238440506147 ) ) ;
#2759 = CARTESIAN_POINT ( 'NONE',  ( -64.08758708074093136, 42.22117905496008916, 2.795515496173683889 ) ) ;
#2761 = CARTESIAN_POINT ( 'NONE',  ( 30.56085893896448269, -1.894852608703655017, -5.974852047816421319 ) ) ;
#2762 = ADVANCED_FACE ( 'NONE', ( #17811 ), #18848, .F. ) ;
#2763 = CARTESIAN_POINT ( 'NONE',  ( -1.349486950856045642, -31.28699069785708531, 6.887161170156906209 ) ) ;
#2764 = CARTESIAN_POINT ( 'NONE',  ( -1.266467741383816348, -27.71311663036093620, 7.751599049952198506 ) ) ;
#2765 = CARTESIAN_POINT ( 'NONE',  ( -63.48867051204930334, 35.67471974816369595, 6.899503081314800390 ) ) ;
#2766 = CARTESIAN_POINT ( 'NONE',  ( 27.32964825819615839, 1.127509148772342762, -4.470608802228491108 ) ) ;
#2767 = DIRECTION ( 'NONE',  ( 1.000000000000000000, 0.000000000000000000, 0.000000000000000000 ) ) ;
#2768 = CARTESIAN_POINT ( 'NONE',  ( -20.34874870218063947, -25.49307895267003587, 6.700000000000000178 ) ) ;
#2769 = FACE_OUTER_BOUND ( 'NONE', #7988, .T. ) ;
#2770 = CARTESIAN_POINT ( 'NONE',  ( 2.474049714983521664, -26.15650803111381606, 7.013842709614101167 ) ) ;
#2771 = CARTESIAN_POINT ( 'NONE',  ( -71.59355962058776868, -48.46505220862084684, 9.978265513184469526 ) ) ;
#2772 = CARTESIAN_POINT ( 'NONE',  ( 33.67397214766437941, -3.719464542966671949, -5.264060338108396131 ) ) ;
#2773 = CARTESIAN_POINT ( 'NONE',  ( 78.50958624606134606, 60.39254520314257491, -2.557033454456006272 ) ) ;
#2774 = DIRECTION ( 'NONE',  ( 1.000000000000000000, 0.000000000000000000, 0.000000000000000000 ) ) ;
#2775 = CYLINDRICAL_SURFACE ( 'NONE', #5545, 0.1000000000000028644 ) ;
#2776 = LINE ( 'NONE', #2988, #4179 ) ;
#2777 = CARTESIAN_POINT ( 'NONE',  ( -30.97867591359219119, -26.64985754041175525, 6.700000000000000178 ) ) ;
#2778 = CARTESIAN_POINT ( 'NONE',  ( -74.72254313616608101, 7.619260614993313752, 10.58017416545770928 ) ) ;
#2779 = CARTESIAN_POINT ( 'NONE',  ( 87.04213330793400871, 0.5878691963681514920, -4.891134986362597914 ) ) ;
#2780 = EDGE_CURVE ( 'NONE', #28971, #27835, #28277, .T. ) ;
#2781 = LINE ( 'NONE', #6053, #36218 ) ;
#2782 = CARTESIAN_POINT ( 'NONE',  ( 22.80421717993787567, 1.676252718750713688, -5.327314847823195088 ) ) ;
#2783 = LINE ( 'NONE', #92, #29740 ) ;
#2784 = VERTEX_POINT ( 'NONE', #15763 ) ;
#2785 = DIRECTION ( 'NONE',  ( 1.000000000000000000, 0.000000000000000000, 0.000000000000000000 ) ) ;
#2786 = CARTESIAN_POINT ( 'NONE',  ( 69.21678231378241719, 58.76388891306111617, -3.990151341881419622 ) ) ;
#2787 = ORIENTED_EDGE ( 'NONE', *, *, #38252, .F. ) ;
#2788 = CARTESIAN_POINT ( 'NONE',  ( 87.65251942239244443, -2.181810347267220340, 2.926837865475490297 ) ) ;
#2789 = CIRCLE ( 'NONE', #25780, 8.080217238368755162 ) ;
#2791 = EDGE_CURVE ( 'NONE', #34298, #15456, #334, .T. ) ;
#2790 = FACE_OUTER_BOUND ( 'NONE', #30369, .T. ) ;
#2792 = CARTESIAN_POINT ( 'NONE',  ( 2.960323002949313054, -26.41197514024928950, 6.864651958020303368 ) ) ;
#2793 = CARTESIAN_POINT ( 'NONE',  ( 1.263448930281367844, -26.19810903602668617, 6.871394612369934762 ) ) ;
#2794 = CONTEXT_DEPENDENT_SHAPE_REPRESENTATION ( #22929, #11 ) ;
#2795 = DIRECTION ( 'NONE',  ( -0.000000000000000000, -1.000000000000000000, -0.000000000000000000 ) ) ;
#2796 = EDGE_LOOP ( 'NONE', ( #7777, #31240, #26410, #29295, #758, #37196, #31718, #10409, #9214, #8538 ) ) ;
#2797 = CARTESIAN_POINT ( 'NONE',  ( 23.14564712628083853, 4.056498438990249866, 3.055703889222537661 ) ) ;
#2798 = DIRECTION ( 'NONE',  ( 0.000000000000000000, 1.000000000000000000, 0.000000000000000000 ) ) ;
#2799 = VERTEX_POINT ( 'NONE', #4042 ) ;
#2800 = CARTESIAN_POINT ( 'NONE',  ( 80.21769632236902225, 61.97993766192919196, -3.195657361810719799 ) ) ;
#2801 = CARTESIAN_POINT ( 'NONE',  ( -0.9949275067606662137, -27.33715503357474930, 7.743886751744253338 ) ) ;
#2802 = CARTESIAN_POINT ( 'NONE',  ( 78.90307038293785524, 66.16006992971016132, -1.301239782962685609 ) ) ;
#2803 = CARTESIAN_POINT ( 'NONE',  ( 79.46360196572364032, 64.13050462409741215, 3.681573067026199464 ) ) ;
#2804 = ORIENTED_EDGE ( 'NONE', *, *, #10458, .F. ) ;
#2805 = ADVANCED_FACE ( 'NONE', ( #6299 ), #37457, .T. ) ;
#2806 = DIRECTION ( 'NONE',  ( 0.000000000000000000, 1.000000000000000000, 0.000000000000000000 ) ) ;
#2808 = VERTEX_POINT ( 'NONE', #34933 ) ;
#2807 = DIRECTION ( 'NONE',  ( -1.000000000000000000, 0.000000000000000000, 0.000000000000000000 ) ) ;
#2809 = CARTESIAN_POINT ( 'NONE',  ( 21.85643539959777826, -4.710037025930063237, 11.93878138912534226 ) ) ;
#2810 = ORIENTED_EDGE ( 'NONE', *, *, #3895, .T. ) ;
#2811 = CARTESIAN_POINT ( 'NONE',  ( -71.75745688627573315, 2.666801288543074300, 9.965618436493368648 ) ) ;
#2812 = CARTESIAN_POINT ( 'NONE',  ( 36.00450899137167227, -3.689287878764249573, 5.669280554162174468 ) ) ;
#2813 = CARTESIAN_POINT ( 'NONE',  ( -1.315742883474435132, -31.34558487397897508, 7.660770905198780234 ) ) ;
#2814 = CARTESIAN_POINT ( 'NONE',  ( -80.58960834254915540, 10.55424001629280717, -2.612171128296283396 ) ) ;
#2815 = CARTESIAN_POINT ( 'NONE',  ( 29.48024936498151405, -3.085360730154540043, -4.807503914550576241 ) ) ;
#2816 = CARTESIAN_POINT ( 'NONE',  ( 37.21202728235306978, -2.743901910341996153, -6.000907511358490432 ) ) ;
#2817 = CARTESIAN_POINT ( 'NONE',  ( -1.739541145475530959, -30.13246378897379429, 7.785096263473211486 ) ) ;
#2818 = CARTESIAN_POINT ( 'NONE',  ( 14.95701748268968778, 12.36391905844671513, 2.521938411237070632 ) ) ;
#2819 = DIRECTION ( 'NONE',  ( 1.000000000000000000, 0.000000000000000000, 0.000000000000000000 ) ) ;
#2820 = CARTESIAN_POINT ( 'NONE',  ( 28.82542678208081455, -3.983772535877290633, 4.161834042892701646 ) ) ;
#2821 = EDGE_CURVE ( 'NONE', #15366, #19353, #12874, .T. ) ;
#2822 = ADVANCED_FACE ( 'NONE', ( #31419 ), #7105, .T. ) ;
#2823 = CARTESIAN_POINT ( 'NONE',  ( 5.057121750476042621, -29.02914024523307646, 7.785868773668302545 ) ) ;
#2824 = VECTOR ( 'NONE', #17716, 1000.000000000000000 ) ;
#2825 = EDGE_CURVE ( 'NONE', #17549, #39112, #30931, .T. ) ;
#2826 = FACE_OUTER_BOUND ( 'NONE', #30564, .T. ) ;
#2827 = CARTESIAN_POINT ( 'NONE',  ( 23.61982383042622402, 0.4723780055816908519, -5.491273804847549123 ) ) ;
#2828 = CARTESIAN_POINT ( 'NONE',  ( 36.84340344443402415, -2.068064908961660731, -5.856630628969484498 ) ) ;
#2829 = CARTESIAN_POINT ( 'NONE',  ( 24.52266067897431157, 2.754179337185791887, -3.866659408860876557 ) ) ;
#2830 = ORIENTED_EDGE ( 'NONE', *, *, #18925, .T. ) ;
#2831 = CARTESIAN_POINT ( 'NONE',  ( 67.02270721038308920, 57.95726884087558517, 3.999016414675010900 ) ) ;
#2832 = CARTESIAN_POINT ( 'NONE',  ( 27.48828073121227433, 1.193421157888713946, 4.496609033324144633 ) ) ;
#2833 = CARTESIAN_POINT ( 'NONE',  ( -1.656341564009858214, -30.11072012155374367, 7.785868773668302545 ) ) ;
#2834 = DIRECTION ( 'NONE',  ( -0.1736481776669340227, 0.9848077530122074652, -0.000000000000000000 ) ) ;
#2835 = CARTESIAN_POINT ( 'NONE',  ( 88.77375424906220758, -2.037038645060464503, 1.247452244799444276 ) ) ;
#2836 = EDGE_CURVE ( 'NONE', #29646, #9655, #23675, .T. ) ;
#2838 = CARTESIAN_POINT ( 'NONE',  ( 36.65097534261938250, -3.107212338371014848, -5.926669128040790824 ) ) ;
#2837 = CARTESIAN_POINT ( 'NONE',  ( 33.33276309746427302, -3.557760156652166383, 5.357383698657358195 ) ) ;
#2839 = B_SPLINE_CURVE_WITH_KNOTS ( 'NONE', 3,
 ( #25557, #657, #10300, #22480 ),
 .UNSPECIFIED., .F., .F.,
 ( 4, 4 ),
 ( 9.697399036122160616E-19, 6.391136169900461152E-06 ),
 .UNSPECIFIED. ) ;
#2840 = EDGE_LOOP ( 'NONE', ( #20264, #20844, #34094, #10773 ) ) ;
#2841 = CARTESIAN_POINT ( 'NONE',  ( 24.37720413515472018, 2.941578208236205416, 3.719711831669278546 ) ) ;
#2842 = CARTESIAN_POINT ( 'NONE',  ( 0.3635682928745467835, -32.69609516209911959, 7.013842709614101167 ) ) ;
#2843 = ORIENTED_EDGE ( 'NONE', *, *, #13113, .F. ) ;
#2844 = CARTESIAN_POINT ( 'NONE',  ( -71.15343164110390717, -21.75733751372833069, 6.007821842535416401 ) ) ;
#2845 = PRODUCT_DEFINITION_CONTEXT ( 'detailed design', #4008, 'design' ) ;
#2846 = ORIENTED_EDGE ( 'NONE', *, *, #34522, .F. ) ;
#2847 = CARTESIAN_POINT ( 'NONE',  ( 79.25608414939210888, 65.04333590781634200, -3.260928702718599581 ) ) ;
#2848 = CARTESIAN_POINT ( 'NONE',  ( -1.699073845469069255, -29.50955693216743114, 7.785172627573962778 ) ) ;
#2849 = CARTESIAN_POINT ( 'NONE',  ( 80.21880177947251411, 63.46656020078421534, 3.697630003121159525 ) ) ;
#2852 = ORIENTED_EDGE ( 'NONE', *, *, #22531, .T. ) ;
#2851 = CARTESIAN_POINT ( 'NONE',  ( -1.338764679050899131, -31.09425634719163867, 6.911401339314953596 ) ) ;
#2850 = AXIS2_PLACEMENT_3D ( 'NONE', #2385, #39204, #18198 ) ;
#2853 = EDGE_CURVE ( 'NONE', #28333, #35369, #3846, .T. ) ;
#2854 = CARTESIAN_POINT ( 'NONE',  ( -58.95285064334387215, 28.35919974994700965, 6.323895744698114996 ) ) ;
#2856 = DIRECTION ( 'NONE',  ( 1.000000000000000000, 1.486905836551549118E-14, 0.000000000000000000 ) ) ;
#2855 = CARTESIAN_POINT ( 'NONE',  ( 4.926836536535178723, -30.92641363086458384, 7.011627023500182965 ) ) ;
#2857 = PLANE ( 'NONE',  #34746 ) ;
#2858 = CARTESIAN_POINT ( 'NONE',  ( -63.08758708074093136, 38.76906266698303227, 4.000000000000000000 ) ) ;
#2859 = CARTESIAN_POINT ( 'NONE',  ( 22.63048122002746965, 4.558493641243840599, -3.110483684673575056 ) ) ;
#2860 = ORIENTED_EDGE ( 'NONE', *, *, #3948, .F. ) ;
#2861 = FACE_OUTER_BOUND ( 'NONE', #19747, .T. ) ;
#2862 = EDGE_CURVE ( 'NONE', #1010, #27757, #28317, .T. ) ;
#2863 = CARTESIAN_POINT ( 'NONE',  ( 25.40259394636483137, -3.746514978370850457, -4.387842602613081233 ) ) ;
#2864 = EDGE_CURVE ( 'NONE', #14158, #12025, #25641, .T. ) ;
#2865 = CARTESIAN_POINT ( 'NONE',  ( -81.72866360994999013, -5.611003566215041261, -1.550695278273204414 ) ) ;
#2866 = DIRECTION ( 'NONE',  ( 0.6751708784618154491, -0.7376613619250370624, 0.000000000000000000 ) ) ;
#2867 = CARTESIAN_POINT ( 'NONE',  ( 80.52090910898030529, 64.76150916408880676, 3.396356880840907699 ) ) ;
#2868 = CARTESIAN_POINT ( 'NONE',  ( 87.21044761576042958, -0.9232309944945271685, 5.337239039084527015 ) ) ;
#2869 = CARTESIAN_POINT ( 'NONE',  ( -105.6213936588467135, -59.15536422891795354, -9.800414904976365804 ) ) ;
#2870 = VERTEX_POINT ( 'NONE', #12666 ) ;
#2871 = CARTESIAN_POINT ( 'NONE',  ( -60.75950795826495465, 23.17721540975219696, -46.17089178453873188 ) ) ;
#2872 = CARTESIAN_POINT ( 'NONE',  ( -72.27608653515989090, -46.45118525884571881, 9.908840844397285963 ) ) ;
#2873 = EDGE_CURVE ( 'NONE', #699, #18231, #22, .T. ) ;
#2874 = DIRECTION ( 'NONE',  ( 1.000000000000000000, 0.000000000000000000, 0.000000000000000000 ) ) ;
#2875 = CARTESIAN_POINT ( 'NONE',  ( 14.99834168678628821, -6.074323333651953760, -2.528087544903816042 ) ) ;
#2876 = PLANE ( 'NONE',  #36603 ) ;
#2877 = CARTESIAN_POINT ( 'NONE',  ( -26.44874870218064089, -25.49307895267003587, 6.700000000000000178 ) ) ;
#2878 = CARTESIAN_POINT ( 'NONE',  ( 1.804255514706574859, -26.17150069821536462, 6.864651958020304257 ) ) ;
#2879 = CARTESIAN_POINT ( 'NONE',  ( 33.62692633095992534, -1.233801386824908697, 5.454693142869670552 ) ) ;
#2880=STYLED_ITEM('',(#40759),#26229);
#2881 = CARTESIAN_POINT ( 'NONE',  ( 86.23508606437836477, 1.494382965102754923, 4.690504771849753674 ) ) ;
#2882 = ORIENTED_EDGE ( 'NONE', *, *, #26330, .T. ) ;
#2884 = CARTESIAN_POINT ( 'NONE',  ( 14.61802081865033820, -4.461849342347350422, 2.500000000000000000 ) ) ;
#2883 = CARTESIAN_POINT ( 'NONE',  ( 80.69089980977658172, 64.07786826041910899, -3.533418250979443620 ) ) ;
#2885 = CARTESIAN_POINT ( 'NONE',  ( -1.324540874619418718, -31.33056052611255637, 7.756742906098587298 ) ) ;
#2886 = EDGE_CURVE ( 'NONE', #7569, #10217, #33549, .T. ) ;
#2887 = CARTESIAN_POINT ( 'NONE',  ( 22.12814134479806327, -2.652490312909201009, 3.660029646613253362 ) ) ;
#2888 = CARTESIAN_POINT ( 'NONE',  ( 1.686887486498432676, -33.27093018339341768, 7.635761828346577573 ) ) ;
#2889 = PLANE ( 'NONE',  #3419 ) ;
#2890 = EDGE_LOOP ( 'NONE', ( #24900, #29553, #8918, #31388 ) ) ;
#2891 = CARTESIAN_POINT ( 'NONE',  ( 27.39224238248323928, -4.425241401586402112, -3.685821984149812547 ) ) ;
#2892 = EDGE_LOOP ( 'NONE', ( #752, #2843, #31101, #8869 ) ) ;
#2893 = AXIS2_PLACEMENT_3D ( 'NONE', #6882, #28906, #25819 ) ;
#2894 = ORIENTED_EDGE ( 'NONE', *, *, #5735, .F. ) ;
#2895 = CARTESIAN_POINT ( 'NONE',  ( 79.82480777417542583, 64.72726844050399109, -3.473545878414593613 ) ) ;
#2896 = CARTESIAN_POINT ( 'NONE',  ( -59.65099889957328116, 26.74201272916461747, -6.661192808835155965 ) ) ;
#2897 = VERTEX_POINT ( 'NONE', #31621 ) ;
#2899 = FACE_OUTER_BOUND ( 'NONE', #9131, .T. ) ;
#2898 = CARTESIAN_POINT ( 'NONE',  ( 22.94192414811271874, 2.589169918962352934, 4.530654349547726945 ) ) ;
#2900 = VERTEX_POINT ( 'NONE', #10181 ) ;
#2901 = CARTESIAN_POINT ( 'NONE',  ( 81.51784234612458135, 64.89972252180021428, -2.776691787112390397 ) ) ;
#2902 = EDGE_CURVE ( 'NONE', #30637, #7963, #23317, .T. ) ;
#2903 = CARTESIAN_POINT ( 'NONE',  ( 4.747787266833422670, -31.29137887042594812, 7.720710062488892689 ) ) ;
#2904 =( BOUNDED_CURVE ( )  B_SPLINE_CURVE ( 3, ( #18996, #40389, #3380, #3180 ),
 .UNSPECIFIED., .F., .T. ) 
 B_SPLINE_CURVE_WITH_KNOTS ( ( 4, 4 ),
 ( 4.708531083176465515, 4.895802057644187855 ),
 .UNSPECIFIED. ) 
 CURVE ( )  GEOMETRIC_REPRESENTATION_ITEM ( )  RATIONAL_B_SPLINE_CURVE ( ( 1.000000000000000000, 0.9970795998553221295, 0.9970795998553221295, 1.000000000000000000 ) ) 
 REPRESENTATION_ITEM ( '' )  );
#2906 = CARTESIAN_POINT ( 'NONE',  ( 86.41267556467273891, 1.294906009465945695, -4.859934084155808520 ) ) ;
#2905 = CARTESIAN_POINT ( 'NONE',  ( -70.66670089265474530, 0.1910294010741415138, 5.995519781525873171 ) ) ;
#2907 = CARTESIAN_POINT ( 'NONE',  ( 0.5786059417041748976, -26.26757555510396713, 7.782861076432730840 ) ) ;
#2908 = CARTESIAN_POINT ( 'NONE',  ( 72.70998213798715426, 61.65396340192921798, 3.619654763610430592 ) ) ;
#2909 = VERTEX_POINT ( 'NONE', #28525 ) ;
#2910 = CARTESIAN_POINT ( 'NONE',  ( 22.87293662167099484, 3.020083017603196751, -4.246090233063728903 ) ) ;
#2911 = ORIENTED_EDGE ( 'NONE', *, *, #27478, .T. ) ;
#2912 = CARTESIAN_POINT ( 'NONE',  ( 7.121324086407810228, -26.64985754041175525, 6.800000000000000711 ) ) ;
#2913 = CARTESIAN_POINT ( 'NONE',  ( 21.85643539959776760, 8.744094842958308078, -10.51782716378651550 ) ) ;
#2914 = ADVANCED_FACE ( 'NONE', ( #17160 ), #29137, .F. ) ;
#2915 = FACE_OUTER_BOUND ( 'NONE', #13802, .T. ) ;
#2916 = ORIENTED_EDGE ( 'NONE', *, *, #7749, .T. ) ;
#2917 = CARTESIAN_POINT ( 'NONE',  ( 1.057242960569752199, -26.12952878737186424, 7.695279973900954751 ) ) ;
#2918 = CARTESIAN_POINT ( 'NONE',  ( 81.88543442889059065, 63.19940289366435593, 2.771525467261982456 ) ) ;
#2919 = CARTESIAN_POINT ( 'NONE',  ( 88.25065740119208613, -0.7696024251930051463, 2.713887439742028285 ) ) ;
#2920 = EDGE_LOOP ( 'NONE', ( #22448, #11812, #22923, #24483, #26225 ) ) ;
#2921 = EDGE_CURVE ( 'NONE', #37024, #36180, #4023, .T. ) ;
#2922 = CARTESIAN_POINT ( 'NONE',  ( 2.853954305276058090, -32.87437726030070451, 6.880608371227949327 ) ) ;
#2923 = CARTESIAN_POINT ( 'NONE',  ( 14.70875212460786585, -5.604200338437857809, 2.501448141494666544 ) ) ;
#2924 = VECTOR ( 'NONE', #30398, 1000.000000000000000 ) ;
#2925 = AXIS2_PLACEMENT_3D ( 'NONE', #16486, #12390, #9496 ) ;
#2926 = DIRECTION ( 'NONE',  ( 0.000000000000000000, 0.000000000000000000, -1.000000000000000000 ) ) ;
#2927 = ADVANCED_FACE ( 'NONE', ( #23160 ), #23562, .T. ) ;
#2928 = CARTESIAN_POINT ( 'NONE',  ( 36.14168653043503809, -3.145492948648968667, -5.847182291702903711 ) ) ;
#2929 = CARTESIAN_POINT ( 'NONE',  ( 5.142386813909727294, -29.02333768617571508, 7.785593909369613819 ) ) ;
#2930 = CARTESIAN_POINT ( 'NONE',  ( -1.347007080367232490, -27.84848149636083647, 7.720710062488895353 ) ) ;
#2931 = CARTESIAN_POINT ( 'NONE',  ( -68.98442902999595105, 21.93515443114010210, -46.17089178453873188 ) ) ;
#2932 = CARTESIAN_POINT ( 'NONE',  ( 21.95193868331012155, 4.960489846753153742, -3.632506201283221881 ) ) ;
#2933 = FACE_OUTER_BOUND ( 'NONE', #10768, .T. ) ;
#2934 = B_SPLINE_CURVE_WITH_KNOTS ( 'NONE', 3,
 ( #8373, #17839, #39671, #1828, #26919, #27121, #5304, #39463, #11454, #23815 ),
 .UNSPECIFIED., .F., .F.,
 ( 4, 2, 2, 2, 4 ),
 ( 0.001566344281586717164, 0.001957551653609773592, 0.002348759025632830236, 0.002739966397655886447, 0.003131173769678943092 ),
 .UNSPECIFIED. ) ;
#2935 = ORIENTED_EDGE ( 'NONE', *, *, #27522, .T. ) ;
#2936 = VECTOR ( 'NONE', #14406, 1000.000000000000000 ) ;
#2937 = VERTEX_POINT ( 'NONE', #1749 ) ;
#2938 = CARTESIAN_POINT ( 'NONE',  ( 36.71867153785819937, -3.456726483225898594, 5.861373841279237773 ) ) ;
#2939 = CARTESIAN_POINT ( 'NONE',  ( -29.07867591359219617, -26.64985754041175525, 6.700000000000000178 ) ) ;
#2940 = ORIENTED_EDGE ( 'NONE', *, *, #7153, .T. ) ;
#2941 = CARTESIAN_POINT ( 'NONE',  ( 66.82596693864583415, 58.04328079001189877, -3.997688572870336188 ) ) ;
#2942 = CARTESIAN_POINT ( 'NONE',  ( 87.43068102542478925, -1.906665703887821417, -3.819564193719649392 ) ) ;
#2943 = B_SPLINE_CURVE_WITH_KNOTS ( 'NONE', 3,
 ( #8887, #21469, #10802, #7928, #24543, #21673, #27827, #4846, #20683, #12184, #29958, #26869, #1984, #39004, #2752, #24754, #39415, #6024, #8114, #33060, #9098, #37302, #14504, #11206, #14301 ),
 .UNSPECIFIED., .F., .F.,
 ( 4, 3, 3, 3, 3, 3, 3, 3, 4 ),
 ( 6.468151674593461604E-05, 9.076621574722018343E-05, 0.0001210204262067970314, 0.0001512763324577426978, 0.0001815301820994211321, 0.0002117781465860719796, 0.0002420274594459745029, 0.0002722905548971148127, 0.0002816827545175550475 ),
 .UNSPECIFIED. ) ;
#2944 = VERTEX_POINT ( 'NONE', #38584 ) ;
#2945 = CARTESIAN_POINT ( 'NONE',  ( -55.57018072619605675, 31.35870463729802538, 3.952748674019340935 ) ) ;
#2946 = CARTESIAN_POINT ( 'NONE',  ( -79.61006498529616238, -6.642554117411252790, -4.980146162474928140 ) ) ;
#2947 = CARTESIAN_POINT ( 'NONE',  ( 66.82540811322722618, 58.08308925668564626, 3.996046963204149094 ) ) ;
#2948 = ORIENTED_EDGE ( 'NONE', *, *, #17006, .T. ) ;
#2949 = DIRECTION ( 'NONE',  ( -0.000000000000000000, -0.000000000000000000, -1.000000000000000000 ) ) ;
#2950 = DIRECTION ( 'NONE',  ( -0.000000000000000000, 1.000000000000000000, -0.000000000000000000 ) ) ;
#2951 = VERTEX_POINT ( 'NONE', #10390 ) ;
#2952 = CARTESIAN_POINT ( 'NONE',  ( 22.20283045833796365, 5.199714587881895334, 3.119843736163353309 ) ) ;
#2953 = CARTESIAN_POINT ( 'NONE',  ( 80.99740051111608352, 66.07939114927816604, -1.509105202935689061 ) ) ;
#2954 = PLANE ( 'NONE',  #20224 ) ;
#2955 = CARTESIAN_POINT ( 'NONE',  ( 79.14683388637743633, 65.58698894143067548, 2.758686562281585264 ) ) ;
#2956 = DIRECTION ( 'NONE',  ( 0.8660254037844449249, -0.4999999999999888423, -0.000000000000000000 ) ) ;
#2957 = ORIENTED_EDGE ( 'NONE', *, *, #17175, .T. ) ;
#2958 = CARTESIAN_POINT ( 'NONE',  ( 75.81058488580238475, 63.71552251304081693, -3.121245466998380902 ) ) ;
#2960 = CARTESIAN_POINT ( 'NONE',  ( 1.551251297819356001, -26.64985754041175525, 6.700000000000000178 ) ) ;
#2959 = DIRECTION ( 'NONE',  ( 0.3420201433256790380, -0.9396926207859046531, -0.000000000000000000 ) ) ;
#2961 = CARTESIAN_POINT ( 'NONE',  ( 17.19129603292001818, 9.338074606371669972, -2.827989852679653637 ) ) ;
#2962 = CARTESIAN_POINT ( 'NONE',  ( 79.12689763788452524, 66.01933680498308377, -2.028924249969750182 ) ) ;
#2963 = CARTESIAN_POINT ( 'NONE',  ( 76.72614680668753806, 63.26816225425361040, 3.643081266322642175 ) ) ;
#2964 = ORIENTED_EDGE ( 'NONE', *, *, #5617, .T. ) ;
#2965 = VECTOR ( 'NONE', #35031, 1000.000000000000000 ) ;
#2966 = CYLINDRICAL_SURFACE ( 'NONE', #10935, 3.399999999999999911 ) ;
#2967 = DIRECTION ( 'NONE',  ( 0.000000000000000000, -1.000000000000000000, -0.000000000000000000 ) ) ;
#2968 = CARTESIAN_POINT ( 'NONE',  ( 80.18989135007177538, 66.21456565649060622, 1.848245342697199645 ) ) ;
#2970 = CARTESIAN_POINT ( 'NONE',  ( -1.698585778792500500, -29.48648546284218597, 6.870716933885664623 ) ) ;
#2969 = CARTESIAN_POINT ( 'NONE',  ( 4.285954546368581752, -31.92892498175183746, 6.875780273367530171 ) ) ;
#2971 = CARTESIAN_POINT ( 'NONE',  ( 32.04447592720433136, -5.114560573210904515, 0.4782324236124577688 ) ) ;
#2972 = CARTESIAN_POINT ( 'NONE',  ( -1.422033770034941691, -31.15121742542976335, 6.941203072598476354 ) ) ;
#2973 = CARTESIAN_POINT ( 'NONE',  ( -1.784526601892259201, -29.51671012356495893, 7.785387725071483800 ) ) ;
#2974 = CARTESIAN_POINT ( 'NONE',  ( -63.02437332573799011, 35.53684452423013340, 6.244480380086192994 ) ) ;
#2975 = CARTESIAN_POINT ( 'NONE',  ( 27.29033202111899570, 1.163606810116843082, -4.463626990047735887 ) ) ;
#2976 = EDGE_CURVE ( 'NONE', #8430, #5452, #25174, .T. ) ;
#2977 = DIRECTION ( 'NONE',  ( 0.9396926207859001012, 0.3420201433256914170, 0.000000000000000000 ) ) ;
#2978 = ORIENTED_EDGE ( 'NONE', *, *, #30502, .F. ) ;
#2979 = CARTESIAN_POINT ( 'NONE',  ( 5.751251297819365504, -26.64985754041175525, 6.800000000000000711 ) ) ;
#2980 = CARTESIAN_POINT ( 'NONE',  ( 0.5338855275361950037, -32.86981913579896286, 7.670465701733744979 ) ) ;
#2981 = ADVANCED_FACE ( 'NONE', ( #4231 ), #39188, .F. ) ;
#2982 = CARTESIAN_POINT ( 'NONE',  ( 1.700390093233090871, -29.56993018339339940, 7.800000000000000711 ) ) ;
#2983 = CARTESIAN_POINT ( 'NONE',  ( -77.95330471031414277, 33.71485196875532608, -8.800414904976364028 ) ) ;
#2984 = CARTESIAN_POINT ( 'NONE',  ( 33.88299691088344190, -0.6033410658551250361, -5.261223570660462201 ) ) ;
#2985 = CARTESIAN_POINT ( 'NONE',  ( 80.01441196509479425, 60.89222036820343220, -2.037985562400662420 ) ) ;
#2986 = DIRECTION ( 'NONE',  ( -1.000000000000000000, 0.000000000000000000, 0.000000000000000000 ) ) ;
#2987 = CARTESIAN_POINT ( 'NONE',  ( -0.9235197406764784622, -31.73212748787619120, 7.782167645815905921 ) ) ;
#2988 = CARTESIAN_POINT ( 'NONE',  ( -28.87867591359218977, -24.55319635012989110, 6.700000000000000178 ) ) ;
#2989 = DIRECTION ( 'NONE',  ( -1.000000000000000000, 0.000000000000000000, 0.000000000000000000 ) ) ;
#2990 = CARTESIAN_POINT ( 'NONE',  ( 2.082411851988426932, -32.94840020570687500, 6.949473656533219135 ) ) ;
#2991 = FACE_OUTER_BOUND ( 'NONE', #3896, .T. ) ;
#2992 = VECTOR ( 'NONE', #23154, 1000.000000000000000 ) ;
#2993 = CARTESIAN_POINT ( 'NONE',  ( 14.76635595020048086, -4.521629488604276048, -2.511015163609813250 ) ) ;
#2994 = AXIS2_PLACEMENT_3D ( 'NONE', #26694, #30179, #11019 ) ;
#2996 = EDGE_LOOP ( 'NONE', ( #19757, #16021, #33769, #26644 ) ) ;
#2995 = VECTOR ( 'NONE', #37718, 1000.000000000000000 ) ;
#2997 = EDGE_LOOP ( 'NONE', ( #12758, #22042, #7381, #30565 ) ) ;
#2998 = FACE_OUTER_BOUND ( 'NONE', #35857, .T. ) ;
#2999 = CARTESIAN_POINT ( 'NONE',  ( 70.60245471852235255, 60.31942058782808402, -3.837797619696055929 ) ) ;
#3000 = CIRCLE ( 'NONE', #2300, 7.538952224936807056 ) ;
#3001 = ORIENTED_EDGE ( 'NONE', *, *, #18169, .T. ) ;
#3002 = LINE ( 'NONE', #37943, #39012 ) ;
#3003 = DIRECTION ( 'NONE',  ( -0.000000000000000000, -1.000000000000000000, -0.000000000000000000 ) ) ;
#3004 = CARTESIAN_POINT ( 'NONE',  ( -1.423076598144291882, -28.22681595598903215, 6.903372536218456368 ) ) ;
#3005 = FACE_OUTER_BOUND ( 'NONE', #40567, .T. ) ;
#3006 = CARTESIAN_POINT ( 'NONE',  ( 5.049684637985137670, -30.15498985193316983, 7.763628509615285722 ) ) ;
#3007 = ORIENTED_EDGE ( 'NONE', *, *, #4349, .F. ) ;
#3008 = CARTESIAN_POINT ( 'NONE',  ( 22.61636450491116079, 4.630129225324790987, 3.032335577038935526 ) ) ;
#3009 = FACE_OUTER_BOUND ( 'NONE', #16422, .T. ) ;
#3010 = EDGE_CURVE ( 'NONE', #3356, #17087, #33242, .T. ) ;
#3011 = VERTEX_POINT ( 'NONE', #1354 ) ;
#3012 = CARTESIAN_POINT ( 'NONE',  ( 80.00843888008158444, 62.42993222482911619, -3.516968106976306796 ) ) ;
#3013 = CARTESIAN_POINT ( 'NONE',  ( -0.9919418010453353585, -27.33356058713898307, 7.750000000000000888 ) ) ;
#3014 = CARTESIAN_POINT ( 'NONE',  ( 81.30277405988975659, 64.78683171160533050, -3.017922835037759377 ) ) ;
#3015 = CARTESIAN_POINT ( 'NONE',  ( 80.39157904934594967, 62.27158585385627987, 3.322373183921395245 ) ) ;
#3016 = VECTOR ( 'NONE', #6358, 1000.000000000000000 ) ;
#3017 = CIRCLE ( 'NONE', #26005, 0.1000000000000028644 ) ;
#3018 = DIRECTION ( 'NONE',  ( -1.000000000000000000, 0.000000000000000000, 0.000000000000000000 ) ) ;
#3019 = CARTESIAN_POINT ( 'NONE',  ( -1.607058046179752786, -30.68314444182777478, 7.780491323090173772 ) ) ;
#3020 = CARTESIAN_POINT ( 'NONE',  ( -36.44874870218064444, -25.49307895267003587, 6.800000000000000711 ) ) ;
#3021 = CARTESIAN_POINT ( 'NONE',  ( 21.85643539959777826, -3.517407513333692837, -12.34883488727242806 ) ) ;
#3022 = CARTESIAN_POINT ( 'NONE',  ( -28.24874870218063805, -25.49307895267003587, 6.700000000000000178 ) ) ;
#3023 = VERTEX_POINT ( 'NONE', #33034 ) ;
#3024 = CARTESIAN_POINT ( 'NONE',  ( -73.53826198524987490, 5.721180179705736002, 10.86979427268231646 ) ) ;
#3025 = DIRECTION ( 'NONE',  ( -0.000000000000000000, -1.000000000000000000, 0.000000000000000000 ) ) ;
#3026 = AXIS2_PLACEMENT_3D ( 'NONE', #14948, #11231, #40066 ) ;
#3027 = B_SPLINE_CURVE_WITH_KNOTS ( 'NONE', 3,
 ( #5222, #11777, #8288, #21076 ),
 .UNSPECIFIED., .F., .F.,
 ( 4, 4 ),
 ( 1.084202172485504434E-18, 6.391136169897158570E-06 ),
 .UNSPECIFIED. ) ;
#3028 = CARTESIAN_POINT ( 'NONE',  ( -1.318021224226250565, -31.34171659909466001, 7.651421919295144036 ) ) ;
#3029 = LINE ( 'NONE', #32031, #40065 ) ;
#3030 = ADVANCED_FACE ( 'NONE', ( #29337 ), #13887, .F. ) ;
#3031 = CARTESIAN_POINT ( 'NONE',  ( 31.99223528116318960, -3.505258990368231409, -5.093870457845899757 ) ) ;
#3032 = CARTESIAN_POINT ( 'NONE',  ( 35.83255119622532447, -3.731021559448283842, -5.622473652077308870 ) ) ;
#3033 = LINE ( 'NONE', #31212, #6500 ) ;
#3034 = CARTESIAN_POINT ( 'NONE',  ( 14.62015730672339231, 13.26385897396263402, 2.488227156191563427 ) ) ;
#3035 = CARTESIAN_POINT ( 'NONE',  ( 1.700390093233090871, -29.56993018339339940, -8.199999999999999289 ) ) ;
#3036 = CARTESIAN_POINT ( 'NONE',  ( 29.91572391670933939, -3.747096582641243234, 4.516102143398081026 ) ) ;
#3037 = CARTESIAN_POINT ( 'NONE',  ( 5.053861318879985021, -29.00936730667186936, 7.782167645815905033 ) ) ;
#3038 = CARTESIAN_POINT ( 'NONE',  ( -69.95453796102918886, -0.5206348589351952327, 3.920659437262051128 ) ) ;
#3039 = CARTESIAN_POINT ( 'NONE',  ( 22.71381320255807168, 0.3598457172671483684, -6.352659116514114856 ) ) ;
#3040 = CARTESIAN_POINT ( 'NONE',  ( 30.95657945650521370, -3.766297307885082546, -4.594095185586652974 ) ) ;
#3041 = CARTESIAN_POINT ( 'NONE',  ( 25.18369925879074600, 2.393806484869988704, -4.034630338149852058 ) ) ;
#3042 = ORIENTED_EDGE ( 'NONE', *, *, #26643, .F. ) ;
#3043 = CARTESIAN_POINT ( 'NONE',  ( 66.99808371854801692, 58.02529356684345885, 3.999241514195644331 ) ) ;
#3044 = CARTESIAN_POINT ( 'NONE',  ( 25.38651582566222231, 1.982134986759825246, 4.168577788436554243 ) ) ;
#3045 = CARTESIAN_POINT ( 'NONE',  ( 4.990103580310159437, -30.76080248691535957, 7.762796336881261361 ) ) ;
#3046 = CIRCLE ( 'NONE', #18788, 3.499999999999999556 ) ;
#3047 = FACE_OUTER_BOUND ( 'NONE', #40193, .T. ) ;
#3048 = VECTOR ( 'NONE', #16281, 1000.000000000000000 ) ;
#3049 = CARTESIAN_POINT ( 'NONE',  ( 85.39132736373097998, 1.761725527925377399, -5.190388716534374502 ) ) ;
#3051 = CARTESIAN_POINT ( 'NONE',  ( 36.94799853101055476, -2.665675819573480432, -5.973026780122190793 ) ) ;
#3050 = DIRECTION ( 'NONE',  ( 1.000000000000000000, 0.000000000000000000, 0.000000000000000000 ) ) ;
#3052 = ORIENTED_EDGE ( 'NONE', *, *, #12468, .T. ) ;
#3053 = CARTESIAN_POINT ( 'NONE',  ( 24.38485034621638192, 2.855400732331458080, 3.806845948903719634 ) ) ;
#3054 = EDGE_CURVE ( 'NONE', #37103, #6285, #28374, .T. ) ;
#3055 = DIRECTION ( 'NONE',  ( 0.000000000000000000, 0.000000000000000000, 1.000000000000000000 ) ) ;
#3056 = AXIS2_PLACEMENT_3D ( 'NONE', #11972, #24550, #34052 ) ;
#3057 = DIRECTION ( 'NONE',  ( -1.000000000000000000, 0.000000000000000000, 0.000000000000000000 ) ) ;
#3058 = ORIENTED_EDGE ( 'NONE', *, *, #31222, .F. ) ;
#3059 = CARTESIAN_POINT ( 'NONE',  ( -71.26311553261176357, -21.73200267494512161, 3.991660656778087901 ) ) ;
#3060 = ORIENTED_EDGE ( 'NONE', *, *, #38073, .T. ) ;
#3061 = CARTESIAN_POINT ( 'NONE',  ( -34.34874870218063592, -25.49307895267003587, 6.800000000000000711 ) ) ;
#3062 = ORIENTED_EDGE ( 'NONE', *, *, #33806, .T. ) ;
#3063 = CARTESIAN_POINT ( 'NONE',  ( 80.68879072954297271, 62.10584950744627974, -3.070011659370638579 ) ) ;
#3064 = EDGE_CURVE ( 'NONE', #19164, #31083, #15949, .T. ) ;
#3065 = CARTESIAN_POINT ( 'NONE',  ( -18.34874870218063947, -26.64985754041175525, 6.700000000000000178 ) ) ;
#3066 = CARTESIAN_POINT ( 'NONE',  ( 79.73288524454797255, 64.30401648905856860, 3.644176963625960664 ) ) ;
#3068 = ORIENTED_EDGE ( 'NONE', *, *, #28132, .F. ) ;
#3067 = DIRECTION ( 'NONE',  ( 0.000000000000000000, 0.000000000000000000, 1.000000000000000000 ) ) ;
#3069 = EDGE_CURVE ( 'NONE', #4028, #40382, #32262, .T. ) ;
#3070 = CARTESIAN_POINT ( 'NONE',  ( -59.00631990433781482, 28.04920808151690181, 6.320701908730214313 ) ) ;
#3072 = CARTESIAN_POINT ( 'NONE',  ( 23.36039791900657292, -7.521532571658541499, 2.500000000000001332 ) ) ;
#3071 = CARTESIAN_POINT ( 'NONE',  ( 4.930099663604494253, -30.91864233902528980, 6.887547729233684635 ) ) ;
#3073 = DIRECTION ( 'NONE',  ( 1.000000000000000000, 0.000000000000000000, 0.000000000000000000 ) ) ;
#3074 = CARTESIAN_POINT ( 'NONE',  ( 33.88948527724345183, -5.411818363456161407, -1.181565996586838363 ) ) ;
#3075 = CARTESIAN_POINT ( 'NONE',  ( 23.42457730801429250, 3.736864044906049287, -3.223246337197901212 ) ) ;
#3076 = VERTEX_POINT ( 'NONE', #11584 ) ;
#3077 = CARTESIAN_POINT ( 'NONE',  ( -76.86283903552966024, -4.590577806607137212, -8.068255941560765976 ) ) ;
#3078 = EDGE_CURVE ( 'NONE', #32722, #20830, #19948, .T. ) ;
#3079 = CARTESIAN_POINT ( 'NONE',  ( 1.300000000000000044, 0.5999999999999995337, 4.250000000000000000 ) ) ;
#3080 = CARTESIAN_POINT ( 'NONE',  ( 81.47459903045201202, 62.11139297693598849, 2.556731990914077546 ) ) ;
#3081 = CARTESIAN_POINT ( 'NONE',  ( 84.20866968570335587, 3.050835305001676101, 0.3231758755354003920 ) ) ;
#3082 = CARTESIAN_POINT ( 'NONE',  ( -6.448748702180637338, -25.49307895267003587, 6.800000000000000711 ) ) ;
#3083 = ORIENTED_EDGE ( 'NONE', *, *, #35411, .T. ) ;
#3084 = DIRECTION ( 'NONE',  ( 0.000000000000000000, 0.000000000000000000, 1.000000000000000000 ) ) ;
#3085 = DIRECTION ( 'NONE',  ( -0.3757233601570931225, -0.9267318687906784813, 0.000000000000000000 ) ) ;
#3086 = AXIS2_PLACEMENT_3D ( 'NONE', #1559, #23578, #33051 ) ;
#3087 = AXIS2_PLACEMENT_3D ( 'NONE', #26295, #10224, #16595 ) ;
#3088 = ORIENTED_EDGE ( 'NONE', *, *, #8921, .T. ) ;
#3089 = CARTESIAN_POINT ( 'NONE',  ( 4.093676667351576093, -27.01607437347052354, 6.941203072598475465 ) ) ;
#3090 = CARTESIAN_POINT ( 'NONE',  ( 1.300000000000000044, 0.5999999999999995337, 4.030609108440248889 ) ) ;
#3091 = CARTESIAN_POINT ( 'NONE',  ( -1.771784689607549979, -30.01038707958819174, 7.013842709614101167 ) ) ;
#3092 = CARTESIAN_POINT ( 'NONE',  ( -26.24874870218063450, -26.64985754041175525, 6.700000000000000178 ) ) ;
#3093 = VERTEX_POINT ( 'NONE', #21702 ) ;
#3094 = CARTESIAN_POINT ( 'NONE',  ( 22.91933054147514781, 2.648295867847167084, 3.783513855737346443 ) ) ;
#3095 = EDGE_CURVE ( 'NONE', #17020, #3093, #14479, .T. ) ;
#3096 = CARTESIAN_POINT ( 'NONE',  ( -4.266520354791871306, -48.67644278316300444, 2.500000000000000000 ) ) ;
#3097 = ORIENTED_EDGE ( 'NONE', *, *, #6200, .T. ) ;
#3099 = CARTESIAN_POINT ( 'NONE',  ( 0.1330790777139393422, 0.5999999999999995337, 3.927362444725310819 ) ) ;
#3098 = CARTESIAN_POINT ( 'NONE',  ( 81.16399599188275715, 62.84525499041613017, -3.248659383495559272 ) ) ;
#3100 = DIRECTION ( 'NONE',  ( -1.000000000000000000, 0.000000000000000000, 0.000000000000000000 ) ) ;
#3101 = VERTEX_POINT ( 'NONE', #21288 ) ;
#3102 = CARTESIAN_POINT ( 'NONE',  ( -1.646010885000422919, -28.96854075337417100, 7.775108481317160702 ) ) ;
#3103 = ORIENTED_EDGE ( 'NONE', *, *, #31523, .T. ) ;
#3104 = DIRECTION ( 'NONE',  ( 1.000000000000000000, 0.000000000000000000, -0.000000000000000000 ) ) ;
#3105 = ORIENTED_EDGE ( 'NONE', *, *, #12178, .T. ) ;
#3106 = CARTESIAN_POINT ( 'NONE',  ( 79.89218238839933406, 64.40427343574535257, -3.614403801066810473 ) ) ;
#3107 = EDGE_CURVE ( 'NONE', #23038, #25920, #2184, .T. ) ;
#3108 = VECTOR ( 'NONE', #34384, 1000.000000000000000 ) ;
#3109 = CARTESIAN_POINT ( 'NONE',  ( 34.16819525005292491, -3.144580783072454810, 5.539171248332353414 ) ) ;
#3110 = EDGE_CURVE ( 'NONE', #2909, #32120, #34138, .T. ) ;
#3111 = ORIENTED_EDGE ( 'NONE', *, *, #5354, .F. ) ;
#3112 = AXIS2_PLACEMENT_3D ( 'NONE', #38420, #10221, #7739 ) ;
#3114 = CARTESIAN_POINT ( 'NONE',  ( 36.09558223311753267, -1.516586179111547361, 5.636573198050853328 ) ) ;
#3113 = CARTESIAN_POINT ( 'NONE',  ( 22.25424755511076214, 2.880317739159906854, 4.805666700857594620 ) ) ;
#3115 = ORIENTED_EDGE ( 'NONE', *, *, #17962, .T. ) ;
#3116 = CIRCLE ( 'NONE', #34051, 0.1000000000000028644 ) ;
#3117 = EDGE_CURVE ( 'NONE', #20830, #6937, #38043, .T. ) ;
#3118 = CARTESIAN_POINT ( 'NONE',  ( 81.76287911024830635, 64.24668757703146582, -2.864610283900680621 ) ) ;
#3119 = DIRECTION ( 'NONE',  ( 1.000000000000000000, 0.000000000000000000, 0.000000000000000000 ) ) ;
#3120 = AXIS2_PLACEMENT_3D ( 'NONE', #24190, #36749, #29962 ) ;
#3122 = CARTESIAN_POINT ( 'NONE',  ( 8.290806648384990041, 0.000000000000000000, -2.500000000000000000 ) ) ;
#3121 = FACE_OUTER_BOUND ( 'NONE', #16633, .T. ) ;
#3123 = CARTESIAN_POINT ( 'NONE',  ( 0.6225211420409756391, -26.24003551177748861, 7.750000000000000888 ) ) ;
#3124 = CARTESIAN_POINT ( 'NONE',  ( 0.4980641348985772043, -26.28438548574166234, 7.762796336881262249 ) ) ;
#3125 = CARTESIAN_POINT ( 'NONE',  ( 73.33958664722344167, 61.75625940721956653, 3.692213121420756305 ) ) ;
#3126 = ORIENTED_EDGE ( 'NONE', *, *, #16718, .F. ) ;
#3127 = EDGE_CURVE ( 'NONE', #38408, #2507, #39654, .T. ) ;
#3128 = CARTESIAN_POINT ( 'NONE',  ( 23.92392269211408617, 2.966294017613217981, -3.818242420704017537 ) ) ;
#3129 = CARTESIAN_POINT ( 'NONE',  ( 21.85643539959775339, 7.579478879252558698, 11.98046644763472024 ) ) ;
#3130 = CARTESIAN_POINT ( 'NONE',  ( 3.549680971525970286, -26.59936163035850498, 7.761113333117554802 ) ) ;
#3131 = ORIENTED_EDGE ( 'NONE', *, *, #5528, .T. ) ;
#3132 = DIRECTION ( 'NONE',  ( 0.000000000000000000, 1.000000000000000000, 0.000000000000000000 ) ) ;
#3133 = CARTESIAN_POINT ( 'NONE',  ( 79.13116897371948255, 66.19293011460084131, 1.571309534768041694 ) ) ;
#3134 = B_SPLINE_CURVE_WITH_KNOTS ( 'NONE', 3,
 ( #14995, #40109, #8603, #8803, #6148, #30869, #18689, #11483, #33554, #30446, #33749, #5529, #18073, #11889, #24886, #37424, #15400, #24672, #21388, #5738, #18480, #31068, #2878, #27957, #40501, #12311, #22064, #9696, #16074, #24271, #31646 ),
 .UNSPECIFIED., .F., .F.,
 ( 4, 3, 3, 3, 3, 3, 3, 3, 3, 3, 4 ),
 ( 2.168404344971008627E-19, 2.999644130997765844E-05, 6.002588995694966905E-05, 8.960886084588222161E-05, 0.0001190604700446502449, 0.0001489538463052725336, 0.0001796139255493988849, 0.0002109707048517092470, 0.0002426195318110382839, 0.0002740640997890069971, 0.0002849778069099863169 ),
 .UNSPECIFIED. ) ;
#3135 = CARTESIAN_POINT ( 'NONE',  ( 86.01579553793663990, 1.740700492558412193, -4.743980989581940477 ) ) ;
#3136 = ORIENTED_EDGE ( 'NONE', *, *, #2345, .T. ) ;
#3137 = CARTESIAN_POINT ( 'NONE',  ( 0.5678122933612703704, -32.77574794603017949, 7.721096864323903297 ) ) ;
#3138 = CARTESIAN_POINT ( 'NONE',  ( 23.84092335974494148, -2.965170422622688040, 3.897202789918388977 ) ) ;
#3139 = AXIS2_PLACEMENT_3D ( 'NONE', #13570, #7789, #3936 ) ;
#3140 = CARTESIAN_POINT ( 'NONE',  ( 33.46241809521923471, -3.087400495052112781, -5.429017654035560803 ) ) ;
#3141 = CARTESIAN_POINT ( 'NONE',  ( 5.100196023652643795, -29.53360033513232352, 7.701140543647732706 ) ) ;
#3142 = CYLINDRICAL_SURFACE ( 'NONE', #4266, 0.09010775117052743921 ) ;
#3143 = AXIS2_PLACEMENT_3D ( 'NONE', #25763, #7221, #859 ) ;
#3144 = ORIENTED_EDGE ( 'NONE', *, *, #28255, .F. ) ;
#3145 = AXIS2_PLACEMENT_3D ( 'NONE', #32185, #12812, #28876 ) ;
#3146 = VECTOR ( 'NONE', #27938, 999.9999999999998863 ) ;
#3147 = CARTESIAN_POINT ( 'NONE',  ( -9.078675913592196167, -24.55319635012989110, 6.700000000000000178 ) ) ;
#3148 = ORIENTED_EDGE ( 'NONE', *, *, #13426, .F. ) ;
#3149 = B_SPLINE_CURVE_WITH_KNOTS ( 'NONE', 3,
 ( #24103, #33803, #37069, #5791, #33190, #11733, #39546, #11329, #38794, #35729, #24519, #11532, #4975, #10588, #34019, #36466, #2309, #8655, #7505 ),
 .UNSPECIFIED., .F., .F.,
 ( 4, 3, 3, 3, 3, 3, 4 ),
 ( 1.939479807224432123E-18, 2.546128104244549286E-05, 5.711050680484235597E-05, 8.113074941676337777E-05, 0.0001053129305727048827, 0.0001360598016347113902, 0.0001612931755702018660 ),
 .UNSPECIFIED. ) ;
#3150 = CARTESIAN_POINT ( 'NONE',  ( -70.92661119047551210, 0.2232129446074198609, 6.013069300985390164 ) ) ;
#3151 = CARTESIAN_POINT ( 'NONE',  ( 66.43088956075783358, 57.76580747938971427, -4.000000000000008882 ) ) ;
#3152 = EDGE_CURVE ( 'NONE', #5452, #37103, #727, .T. ) ;
#3153 = CARTESIAN_POINT ( 'NONE',  ( 87.67937458983125509, -2.214055474509613930, -2.742479142822641602 ) ) ;
#3154 = EDGE_LOOP ( 'NONE', ( #19142, #36431, #6585, #38308 ) ) ;
#3155 = EDGE_CURVE ( 'NONE', #24578, #14209, #12519, .T. ) ;
#3156 = CARTESIAN_POINT ( 'NONE',  ( -74.78824586187189993, 9.457194952391420273, -9.226500222781202964 ) ) ;
#3157 = DIRECTION ( 'NONE',  ( 0.000000000000000000, 0.000000000000000000, 1.000000000000000000 ) ) ;
#3158 =( BOUNDED_CURVE ( )  B_SPLINE_CURVE ( 3, ( #40285, #3470, #38015, #28143 ),
 .UNSPECIFIED., .F., .T. ) 
 B_SPLINE_CURVE_WITH_KNOTS ( ( 4, 4 ),
 ( 4.712388980384689674, 5.617490880575807921 ),
 .UNSPECIFIED. ) 
 CURVE ( )  GEOMETRIC_REPRESENTATION_ITEM ( )  RATIONAL_B_SPLINE_CURVE ( ( 1.000000000000000000, 0.9328897322841716022, 0.9328897322841716022, 1.000000000000000000 ) ) 
 REPRESENTATION_ITEM ( '' )  );
#3159 = FACE_BOUND ( 'NONE', #38953, .T. ) ;
#3160 = FACE_OUTER_BOUND ( 'NONE', #26573, .T. ) ;
#3161 = ORIENTED_EDGE ( 'NONE', *, *, #7055, .F. ) ;
#3162 = CARTESIAN_POINT ( 'NONE',  ( 21.83976307972709918, 5.907766738269700113, 3.159785223916961705 ) ) ;
#3163 = EDGE_CURVE ( 'NONE', #12201, #3101, #8559, .T. ) ;
#3164 = CARTESIAN_POINT ( 'NONE',  ( 81.16949749213439702, 61.30395080096879212, -1.008685033153519983 ) ) ;
#3165 = DIRECTION ( 'NONE',  ( 1.000000000000000000, -0.000000000000000000, 0.000000000000000000 ) ) ;
#3166 = CARTESIAN_POINT ( 'NONE',  ( 79.76203521409539121, 64.68678814937342736, 3.489836119548952009 ) ) ;
#3167 = EDGE_CURVE ( 'NONE', #40638, #37085, #34918, .T. ) ;
#3168 = FACE_OUTER_BOUND ( 'NONE', #28355, .T. ) ;
#3169 = VERTEX_POINT ( 'NONE', #23311 ) ;
#3170 = CARTESIAN_POINT ( 'NONE',  ( 76.74823446354515966, 60.29158698200773614, -3.346357594037797423 ) ) ;
#3172 = FACE_OUTER_BOUND ( 'NONE', #19431, .T. ) ;
#3171 = CARTESIAN_POINT ( 'NONE',  ( 2.327231899816259997, -33.01333973636840824, 7.643192810543819604 ) ) ;
#3173 = CARTESIAN_POINT ( 'NONE',  ( 17.10588945481550383, 9.262888318566355750, -2.855260069168449988 ) ) ;
#3174 = AXIS2_PLACEMENT_3D ( 'NONE', #3861, #34750, #28748 ) ;
#3175 = CARTESIAN_POINT ( 'NONE',  ( 81.09339258687016638, 63.16289930221478954, -3.352621494407070024 ) ) ;
#3176 = CARTESIAN_POINT ( 'NONE',  ( 77.55533639035668614, 62.99992453720928864, 3.808649511194677650 ) ) ;
#3177 = TOROIDAL_SURFACE ( 'NONE', #25503, 10.99999999999998579, 3.000000000000000000 ) ;
#3178 = ORIENTED_EDGE ( 'NONE', *, *, #7572, .F. ) ;
#3179 = CARTESIAN_POINT ( 'NONE',  ( 4.746218651982971437, -31.29415061712129287, 7.660770905198780234 ) ) ;
#3180 = CARTESIAN_POINT ( 'NONE',  ( 3.973866779147308570, -26.90885826429679284, 6.894806418505347700 ) ) ;
#3181 = CARTESIAN_POINT ( 'NONE',  ( 81.67240355425563791, 65.37253450681799904, 2.134985007309429861 ) ) ;
#3183 = CARTESIAN_POINT ( 'NONE',  ( -1.696924646384579738, -29.43445957933605683, 6.865312560952603782 ) ) ;
#3182 = CARTESIAN_POINT ( 'NONE',  ( 4.312771555195475059, -31.89921506522781058, 6.863784140767622333 ) ) ;
#3184 = CARTESIAN_POINT ( 'NONE',  ( 32.03962978398497796, -5.076534887360421244, -0.9488177176524058565 ) ) ;
#3185 = CARTESIAN_POINT ( 'NONE',  ( -12.99139449055068596, 10.37661300689600097, 6.000000000000000000 ) ) ;
#3186 = CARTESIAN_POINT ( 'NONE',  ( 24.20305058822417266, -8.556106420403189361, 2.499999999999995115 ) ) ;
#3187 = CARTESIAN_POINT ( 'NONE',  ( -64.08758708074091714, 36.87876644325631759, 4.900609702795900802 ) ) ;
#3188 = DIRECTION ( 'NONE',  ( -1.000000000000000000, 0.000000000000000000, -0.000000000000000000 ) ) ;
#3189 = CARTESIAN_POINT ( 'NONE',  ( -0.6373138688605560764, -32.03876546204544695, 6.920489980334476599 ) ) ;
#3190 = CARTESIAN_POINT ( 'NONE',  ( -18.44874870218064089, -26.64985754041175525, 6.700000000000000178 ) ) ;
#3191 = DIRECTION ( 'NONE',  ( 0.000000000000000000, 0.000000000000000000, 1.000000000000000000 ) ) ;
#3192 = CARTESIAN_POINT ( 'NONE',  ( 23.31574928852108286, 3.489132783961883533, -3.362529947468282820 ) ) ;
#3193 = CARTESIAN_POINT ( 'NONE',  ( -6.248748702180631831, -26.64985754041175525, 6.700000000000000178 ) ) ;
#3194 = DIRECTION ( 'NONE',  ( 0.000000000000000000, 0.000000000000000000, 1.000000000000000000 ) ) ;
#3195 = CARTESIAN_POINT ( 'NONE',  ( 0.5197218266442334977, -32.86477804699348582, 7.750000000000000888 ) ) ;
#3196 = DIRECTION ( 'NONE',  ( 1.000000000000000000, -0.000000000000000000, 0.000000000000000000 ) ) ;
#3197 = CARTESIAN_POINT ( 'NONE',  ( 2.137331256184830330, -32.94175133076011264, 6.871394612369936539 ) ) ;
#3198 = B_SPLINE_CURVE_WITH_KNOTS ( 'NONE', 3,
 ( #246, #12784, #33822, #28226 ),
 .UNSPECIFIED., .F., .F.,
 ( 4, 4 ),
 ( -1.385643128159646227E-05, 0.0002401580581033240457 ),
 .UNSPECIFIED. ) ;
#3199 = CARTESIAN_POINT ( 'NONE',  ( -64.08758708074093136, 37.74469198210380227, -4.273126118783022065 ) ) ;
#3200 = VECTOR ( 'NONE', #2455, 1000.000000000000000 ) ;
#3201 = CARTESIAN_POINT ( 'NONE',  ( 22.03054732944672267, -11.55401157302784121, 2.500000000000000000 ) ) ;
#3202 = VERTEX_POINT ( 'NONE', #39340 ) ;
#3203 = DIRECTION ( 'NONE',  ( 1.000000000000000000, 0.000000000000000000, 0.000000000000000000 ) ) ;
#3204 = CARTESIAN_POINT ( 'NONE',  ( 68.55047844998404116, 58.76352648041117277, -3.988324671431286106 ) ) ;
#3205 = CARTESIAN_POINT ( 'NONE',  ( 2.949167456357904893, -26.30028875085877971, 6.875671892026063325 ) ) ;
#3206 = ORIENTED_EDGE ( 'NONE', *, *, #18499, .F. ) ;
#3207 = DIRECTION ( 'NONE',  ( -0.000000000000000000, -0.000000000000000000, -1.000000000000000000 ) ) ;
#3208 = CARTESIAN_POINT ( 'NONE',  ( -11.81496944966682960, -21.25669541281728669, -1.000000000000000000 ) ) ;
#3209 = CARTESIAN_POINT ( 'NONE',  ( 5.041426625178103471, -28.52708634086149431, 6.887547729233689964 ) ) ;
#3210 = LINE ( 'NONE', #35497, #6955 ) ;
#3212 = ADVANCED_FACE ( 'NONE', ( #20406 ), #22912, .F. ) ;
#3211 = CARTESIAN_POINT ( 'NONE',  ( 5.026336154413283630, -30.27568385775391491, 7.759451378593097637 ) ) ;
#3213 = CARTESIAN_POINT ( 'NONE',  ( 23.75242797775258197, 3.571880847392433722, 3.151661273409955832 ) ) ;
#3214 = EDGE_CURVE ( 'NONE', #21048, #17583, #11200, .T. ) ;
#3215 = CYLINDRICAL_SURFACE ( 'NONE', #32680, 6.000000000000005329 ) ;
#3216 = CARTESIAN_POINT ( 'NONE',  ( 18.04466435519415768, -3.159710396077179517, 2.979303362740127081 ) ) ;
#3217 = ORIENTED_EDGE ( 'NONE', *, *, #18879, .F. ) ;
#3218 = EDGE_CURVE ( 'NONE', #39042, #34269, #36079, .T. ) ;
#3219 = CARTESIAN_POINT ( 'NONE',  ( 1.700390093233090871, -29.56993018339339940, 7.800000000000000711 ) ) ;
#3220 = ORIENTED_EDGE ( 'NONE', *, *, #22577, .F. ) ;
#3221 = CARTESIAN_POINT ( 'NONE',  ( 78.35540530300707474, 65.82096406625564100, -1.612955153530279739 ) ) ;
#3222 = AXIS2_PLACEMENT_3D ( 'NONE', #8894, #9305, #21477 ) ;
#3224 = CARTESIAN_POINT ( 'NONE',  ( -1.676831472725793137, -29.96287608038002759, 6.911401339314957148 ) ) ;
#3223 = CARTESIAN_POINT ( 'NONE',  ( 22.00621292889270819, 0.2476518612282572751, 7.633907389783355590 ) ) ;
#3225 = CARTESIAN_POINT ( 'NONE',  ( 79.60170308687696661, 66.12598108333446589, -2.076176908533889698 ) ) ;
#3226 = CARTESIAN_POINT ( 'NONE',  ( 80.34542504610526237, 62.25824679691980634, 3.331801170923413213 ) ) ;
#3227 = CARTESIAN_POINT ( 'NONE',  ( 82.56222392620333039, 63.90769089702598649, 1.000000000000000000 ) ) ;
#3228 = CARTESIAN_POINT ( 'NONE',  ( 2.769712674093031790, -32.79741141385554215, 7.774064877406527962 ) ) ;
#3229 = CARTESIAN_POINT ( 'NONE',  ( 21.85643539959779957, 2.883972393613821072, 11.80804406839454046 ) ) ;
#3230 = PLANE ( 'NONE',  #27251 ) ;
#3231 = ORIENTED_EDGE ( 'NONE', *, *, #15623, .F. ) ;
#3232 = CARTESIAN_POINT ( 'NONE',  ( -74.60456144785419497, 9.286899217492273095, 9.301175053638090162 ) ) ;
#3233 = CARTESIAN_POINT ( 'NONE',  ( 37.06055832016893703, -3.177318995967190585, 5.963242555153861701 ) ) ;
#3234 = ORIENTED_EDGE ( 'NONE', *, *, #28324, .F. ) ;
#3235 = AXIS2_PLACEMENT_3D ( 'NONE', #7498, #1745, #26450 ) ;
#3236 = CARTESIAN_POINT ( 'NONE',  ( -1.321885274144181555, -31.33510862625826121, 7.640616322432100205 ) ) ;
#3237 = EDGE_LOOP ( 'NONE', ( #16370, #19178, #33564, #34234 ) ) ;
#3238 = CARTESIAN_POINT ( 'NONE',  ( -81.11237078102703890, 10.50958725180905873, -4.125641042171466211 ) ) ;
#3239 = DIRECTION ( 'NONE',  ( 1.000000000000000000, 0.000000000000000000, 0.000000000000000000 ) ) ;
#3240 = CARTESIAN_POINT ( 'NONE',  ( 20.92112071914918303, 4.582339863481973197, -2.646876999278094278 ) ) ;
#3241 = CARTESIAN_POINT ( 'NONE',  ( 3.844353976790406247, -32.20876071027002041, 6.889465824494255486 ) ) ;
#3242 = CARTESIAN_POINT ( 'NONE',  ( 20.81473064669264161, 6.282592952945772247, 3.335602345720931172 ) ) ;
#3243 = CARTESIAN_POINT ( 'NONE',  ( -10.34874870218063769, -26.64985754041175525, 6.700000000000000178 ) ) ;
#3244 = CARTESIAN_POINT ( 'NONE',  ( 4.326139684082770387, -31.72989624158975630, 7.670860738520324240 ) ) ;
#3245 = CARTESIAN_POINT ( 'NONE',  ( 3.346956565312060761, -25.15115677713068365, 7.695279973900954751 ) ) ;
#3246 = DIRECTION ( 'NONE',  ( -0.1736481776669207000, -0.9848077530122097967, -0.000000000000000000 ) ) ;
#3247 = CARTESIAN_POINT ( 'NONE',  ( 23.18753022366955108, 0.6683388799240479461, -5.710891331619152744 ) ) ;
#3248 = CARTESIAN_POINT ( 'NONE',  ( 28.66920249112477848, -4.024975064351027143, -4.110187144531254333 ) ) ;
#3249 = CLOSED_SHELL ( 'NONE', ( #31808, #4835, #38901, #19241, #34, #170, #3534, #4397, #23902, #38393, #36869, #25308, #14226, #22297, #26408, #11362, #10317, #4872, #23394, #33780, #28320, #28838, #21359, #19161, #37285, #13937, #4285, #28559, #33246, #15901, #34295, #13889, #28837, #29190, #21592, #9071, #7757, #26997, #7122, #39813, #37440, #21489, #3571, #4345, #18597, #7169, #4571, #26471, #24956, #18628, #17638, #36175, #15823, #26445, #20171, #12910, #9380, #8391, #20723, #30445, #20956, #20536, #12698, #37317, #31515, #20151, #37641, #1052, #3452, #37971, #33505, #6672, #28022, #35316, #34160, #31971, #9060, #27872, #20168, #7872, #24310, #35138, #1327, #23124 ) ) ;
#3250 = CARTESIAN_POINT ( 'NONE',  ( 26.62467638871712339, 1.621415574385618008, -4.335577499637811805 ) ) ;
#3251 = ORIENTED_EDGE ( 'NONE', *, *, #28369, .T. ) ;
#3252 = CARTESIAN_POINT ( 'NONE',  ( 67.05715689120697220, 57.86208461462646113, 3.995640437668404044 ) ) ;
#3253 = CARTESIAN_POINT ( 'NONE',  ( 37.06592056232945254, -2.656377846863923864, 5.990200015405097389 ) ) ;
#3254 = CARTESIAN_POINT ( 'NONE',  ( 3.926249267005272436, -32.27095793936597090, 6.894806418505347700 ) ) ;
#3255 = CARTESIAN_POINT ( 'NONE',  ( 86.42495861400665547, -0.1300389677119091758, -5.942483626122943896 ) ) ;
#3256 = CARTESIAN_POINT ( 'NONE',  ( 21.58863229896841673, 7.203270328900314823, 2.924123313244538558 ) ) ;
#3257 = ORIENTED_EDGE ( 'NONE', *, *, #36684, .T. ) ;
#3258 = CARTESIAN_POINT ( 'NONE',  ( 25.63475025744274305, 2.159471803233731446, 4.132560422135860279 ) ) ;
#3259 = FACE_OUTER_BOUND ( 'NONE', #13167, .T. ) ;
#3260 = DIRECTION ( 'NONE',  ( -0.000000000000000000, -0.000000000000000000, -1.000000000000000000 ) ) ;
#3261 = VECTOR ( 'NONE', #12879, 1000.000000000000000 ) ;
#3262 = ORIENTED_EDGE ( 'NONE', *, *, #30791, .T. ) ;
#3263 = CARTESIAN_POINT ( 'NONE',  ( 6.921324086407803833, -26.64985754041175525, 6.700000000000000178 ) ) ;
#3264 = EDGE_CURVE ( 'NONE', #29308, #8770, #34652, .T. ) ;
#3265 = EDGE_LOOP ( 'NONE', ( #16864, #16195, #34493, #16904 ) ) ;
#3266 = CARTESIAN_POINT ( 'NONE',  ( 79.97265554092989248, 63.70311272660515556, -3.710743084827438754 ) ) ;
#3267 = CARTESIAN_POINT ( 'NONE',  ( -1.724485732198442367, -28.92201308620781930, 7.785096263473211486 ) ) ;
#3268 = CARTESIAN_POINT ( 'NONE',  ( 79.40192692649263506, 64.80415203875446650, 3.426353657592664526 ) ) ;
#3271 = ORIENTED_EDGE ( 'NONE', *, *, #40629, .T. ) ;
#3270 = ORIENTED_EDGE ( 'NONE', *, *, #36036, .F. ) ;
#3269 = CARTESIAN_POINT ( 'NONE',  ( 14.68065631944699412, 12.91438177319650649, 2.499999999999999556 ) ) ;
#3272 = FACE_OUTER_BOUND ( 'NONE', #21935, .T. ) ;
#3273 = CARTESIAN_POINT ( 'NONE',  ( -58.94223801633730631, 28.40373775090870012, 6.290611457194089873 ) ) ;
#3274 = AXIS2_PLACEMENT_3D ( 'NONE', #21161, #28351, #30847 ) ;
#3275 =( BOUNDED_CURVE ( )  B_SPLINE_CURVE ( 3, ( #2328, #14444, #8060, #14849 ),
 .UNSPECIFIED., .F., .T. ) 
 B_SPLINE_CURVE_WITH_KNOTS ( ( 4, 4 ),
 ( 4.748221474220560623, 4.941946782021394924 ),
 .UNSPECIFIED. ) 
 CURVE ( )  GEOMETRIC_REPRESENTATION_ITEM ( )  RATIONAL_B_SPLINE_CURVE ( ( 1.000000000000000000, 0.9968749865767494445, 0.9968749865767494445, 1.000000000000000000 ) ) 
 REPRESENTATION_ITEM ( '' )  );
#3276 = CARTESIAN_POINT ( 'NONE',  ( -64.08758708074093136, 38.13199975834724142, -3.043809435734133206 ) ) ;
#3277 = DIRECTION ( 'NONE',  ( 0.000000000000000000, -0.000000000000000000, -1.000000000000000000 ) ) ;
#3278 = CARTESIAN_POINT ( 'NONE',  ( 14.66962918947507788, -4.461849342347338876, 2.500000000000000000 ) ) ;
#3279 = CARTESIAN_POINT ( 'NONE',  ( 22.87815214592131952, 4.326272378261545981, -3.076133176055316554 ) ) ;
#3280 = ORIENTED_EDGE ( 'NONE', *, *, #23460, .F. ) ;
#3281 = ORIENTED_EDGE ( 'NONE', *, *, #24500, .T. ) ;
#3282 = LINE ( 'NONE', #28358, #12863 ) ;
#3283 = CARTESIAN_POINT ( 'NONE',  ( -68.71186372058384961, 37.81212149306785619, 8.800414904976364028 ) ) ;
#3284 = FACE_OUTER_BOUND ( 'NONE', #20019, .T. ) ;
#3285 = CARTESIAN_POINT ( 'NONE',  ( 5.014391224573804706, -30.32979629098898400, 6.882085323592686876 ) ) ;
#3286 = CARTESIAN_POINT ( 'NONE',  ( 79.68360889523903268, 65.64663933523165440, 2.797238656122799760 ) ) ;
#3287 = CARTESIAN_POINT ( 'NONE',  ( 87.93534175303985023, -2.522256948347837202, 0.2133659395812929627 ) ) ;
#3288 = DIRECTION ( 'NONE',  ( -0.000000000000000000, -1.000000000000000000, -0.000000000000000000 ) ) ;
#3289 = VERTEX_POINT ( 'NONE', #26599 ) ;
#3290 = CARTESIAN_POINT ( 'NONE',  ( 2.863609035986291573, -26.26888160889163615, 7.695279973900954751 ) ) ;
#3291 = CARTESIAN_POINT ( 'NONE',  ( 14.61802081865033287, 12.33286846116284252, -3.500000000000000000 ) ) ;
#3292 = ADVANCED_FACE ( 'NONE', ( #30917 ), #17501, .T. ) ;
#3293 = VECTOR ( 'NONE', #19856, 1000.000000000000000 ) ;
#3294 = DIRECTION ( 'NONE',  ( 0.000000000000000000, 0.000000000000000000, 1.000000000000000000 ) ) ;
#3295 = CARTESIAN_POINT ( 'NONE',  ( 0.1003003074055170557, -25.13424064674780922, 7.635761828346577573 ) ) ;
#3296 = CARTESIAN_POINT ( 'NONE',  ( 4.650447641269607857, -27.87959612855872393, 7.775108481317163367 ) ) ;
#3297 = DIRECTION ( 'NONE',  ( 0.000000000000000000, 0.000000000000000000, 1.000000000000000000 ) ) ;
#3298 = B_SPLINE_SURFACE_WITH_KNOTS ( 'NONE', 5, 3, ( 
 ( #24220, #33711, #19163, #22270, #10290, #3951, #12984 ),
 ( #3543, #13378, #28635, #35637, #35437, #38089, #847 ),
 ( #16656, #35037, #10091, #1054, #19369, #16269, #32151 ),
 ( #32347, #13586, #28841, #18958, #38289, #22469, #38690 ),
 ( #25956, #19576, #22674, #31727, #19772, #10488, #6613 ),
 ( #38487, #22868, #231, #16470, #23069, #34838, #4142 ),
 ( #25344, #35238, #3744, #16069, #29042, #649, #13185 ),
 ( #440, #37882, #31524, #9692, #28424, #7208, #9892 ) ),
 .UNSPECIFIED., .F., .F., .F.,
 ( 6, 2, 6 ),
 ( 4, 1, 1, 1, 4 ),
 ( 0.000000000000000000, 0.5000000000000000000, 1.000000000000000000 ),
 ( 0.000000000000000000, 0.001661007895493813585, 0.002768346492489689309, 0.004010280040507323805, 0.005386808539546716207 ),
 .UNSPECIFIED. ) ;
#3299 = CARTESIAN_POINT ( 'NONE',  ( 33.46282145848507383, -3.084177183246969545, 5.429080608628573223 ) ) ;
#3300 = EDGE_CURVE ( 'NONE', #25120, #25461, #5379, .T. ) ;
#3301 = CARTESIAN_POINT ( 'NONE',  ( 88.50738123939095203, -1.057966825106399389, -0.8062500484416172952 ) ) ;
#3302 = CIRCLE ( 'NONE', #5912, 0.1000000000000028644 ) ;
#3303 = ORIENTED_EDGE ( 'NONE', *, *, #38854, .T. ) ;
#3305 = DIRECTION ( 'NONE',  ( -0.8660254037844344888, -0.5000000000000069944, -0.000000000000000000 ) ) ;
#3304 = CARTESIAN_POINT ( 'NONE',  ( 80.87203728266233327, 63.05930952086730201, -3.432259906339282463 ) ) ;
#3306 = CARTESIAN_POINT ( 'NONE',  ( -66.99872204295122913, 28.48507918597134037, 4.000000000000000000 ) ) ;
#3307 = EDGE_LOOP ( 'NONE', ( #7824, #7820, #36129, #32335, #26174, #34431, #38908, #39568 ) ) ;
#3308 = CARTESIAN_POINT ( 'NONE',  ( -1.626039020774626032, -28.86646067482757871, 7.761597726988852308 ) ) ;
#3309 = EDGE_LOOP ( 'NONE', ( #36708, #38314, #1720, #31914 ) ) ;
#3310 = CARTESIAN_POINT ( 'NONE',  ( -71.75880299933005801, 2.675120194517714989, 9.965498832022653630 ) ) ;
#3311 = VERTEX_POINT ( 'NONE', #33604 ) ;
#3312 = EDGE_CURVE ( 'NONE', #23027, #9241, #5790, .T. ) ;
#3313 = EDGE_CURVE ( 'NONE', #17660, #27165, #39960, .T. ) ;
#3314 = CARTESIAN_POINT ( 'NONE',  ( 79.02959213847954345, 65.76024385718582721, -2.482170738714647218 ) ) ;
#3315 = CARTESIAN_POINT ( 'NONE',  ( 35.98118923361300858, -3.154045095838573953, 5.822132806892088119 ) ) ;
#3317 = CARTESIAN_POINT ( 'NONE',  ( 20.40287464304303100, 10.75613383955523616, -2.500000000000000000 ) ) ;
#3316 = CARTESIAN_POINT ( 'NONE',  ( 22.48367044534919401, 2.651248834843010549, 4.808582237203087750 ) ) ;
#3319 = ORIENTED_EDGE ( 'NONE', *, *, #22977, .T. ) ;
#3318 = ORIENTED_EDGE ( 'NONE', *, *, #13134, .T. ) ;
#3320 = CARTESIAN_POINT ( 'NONE',  ( 82.03499260127743753, 62.66326407617577132, -2.270757614041408079 ) ) ;
#3321 = CYLINDRICAL_SURFACE ( 'NONE', #25271, 0.1000000000000028644 ) ;
#3323 = CARTESIAN_POINT ( 'NONE',  ( 85.62084935951537545, 2.184322785437529557, -3.437511279438954404 ) ) ;
#3322 = CARTESIAN_POINT ( 'NONE',  ( -16.27783086239806210, 25.90100547710869705, -2.500000000000000000 ) ) ;
#3324 = DIRECTION ( 'NONE',  ( 0.6427876096865481337, -0.7660444431189707970, -0.000000000000000000 ) ) ;
#3325 = CARTESIAN_POINT ( 'NONE',  ( 0.3454438073185458480, -0.6000000000000004219, 3.946157045896946602 ) ) ;
#3326 = CARTESIAN_POINT ( 'NONE',  ( 74.91450450041774900, 59.74817859300106448, 3.564124015814033264 ) ) ;
#3327 = ORIENTED_EDGE ( 'NONE', *, *, #28017, .F. ) ;
#3328 = CARTESIAN_POINT ( 'NONE',  ( 23.20847637278877684, 3.432400490018996386, -3.727618341475917862 ) ) ;
#3329 = EDGE_LOOP ( 'NONE', ( #28001, #25555, #17461, #13984 ) ) ;
#3330 = EDGE_CURVE ( 'NONE', #13148, #20646, #6623, .T. ) ;
#3331 = CARTESIAN_POINT ( 'NONE',  ( 21.85643539959777826, -5.920441741711214512, 15.33489310402742234 ) ) ;
#3332 = VECTOR ( 'NONE', #34733, 1000.000000000000000 ) ;
#3333 = FACE_OUTER_BOUND ( 'NONE', #15770, .T. ) ;
#3334 = DIRECTION ( 'NONE',  ( 0.5171480877355281169, -0.2439873919671817493, 0.8203828422831251910 ) ) ;
#3335 = CARTESIAN_POINT ( 'NONE',  ( 78.88661621011570446, 66.15061626711309373, 1.323744132979558286 ) ) ;
#3336 = CARTESIAN_POINT ( 'NONE',  ( 88.48259847388298738, -1.030129646626848361, 1.133857545573457415 ) ) ;
#3337 = ORIENTED_EDGE ( 'NONE', *, *, #14439, .T. ) ;
#3338 = CARTESIAN_POINT ( 'NONE',  ( -4.878675913592187108, -26.64985754041175525, 6.800000000000000711 ) ) ;
#3339 = CARTESIAN_POINT ( 'NONE',  ( 33.10913737875220875, -3.231866217708247113, 5.373879654101829217 ) ) ;
#3340 = CARTESIAN_POINT ( 'NONE',  ( 36.99286102142031751, -2.718909609684730722, -5.980028656754092786 ) ) ;
#3341 = CARTESIAN_POINT ( 'NONE',  ( 5.100265157569299213, -29.54064031832051995, 7.730758795053803922 ) ) ;
#3342 = DIRECTION ( 'NONE',  ( 0.000000000000000000, 1.000000000000000000, 0.000000000000000000 ) ) ;
#3343 = ADVANCED_FACE ( 'NONE', ( #11328, #15246 ), #40158, .T. ) ;
#3344 = ADVANCED_FACE ( 'NONE', ( #8045 ), #2308, .F. ) ;
#3345 = CARTESIAN_POINT ( 'NONE',  ( 0.3101223678018852903, -32.78940688952906157, 7.387053503561888057 ) ) ;
#3346 = EDGE_CURVE ( 'NONE', #33732, #3833, #33188, .T. ) ;
#3347 = AXIS2_PLACEMENT_3D ( 'NONE', #8799, #33959, #30865 ) ;
#3348 = CARTESIAN_POINT ( 'NONE',  ( -1.231676799035886338, -31.29127234582281147, 7.740055089680402567 ) ) ;
#3349 = FACE_OUTER_BOUND ( 'NONE', #11070, .T. ) ;
#3350 = ORIENTED_EDGE ( 'NONE', *, *, #12600, .F. ) ;
#3351 = ORIENTED_EDGE ( 'NONE', *, *, #12414, .F. ) ;
#3352 = CARTESIAN_POINT ( 'NONE',  ( 23.38445204029254398, 3.558657874120639164, 3.098095084708739400 ) ) ;
#3353 = DIRECTION ( 'NONE',  ( 1.000000000000000000, 7.232507224765808510E-18, 0.000000000000000000 ) ) ;
#3354 = ORIENTED_EDGE ( 'NONE', *, *, #9205, .T. ) ;
#3355 = CARTESIAN_POINT ( 'NONE',  ( 66.41308122482412557, 57.81611748292259279, -4.000000000000024869 ) ) ;
#3356 = VERTEX_POINT ( 'NONE', #18327 ) ;
#3357 = CARTESIAN_POINT ( 'NONE',  ( -55.72565997008030081, 31.19966888624958301, 3.920894724096667172 ) ) ;
#3358 = VECTOR ( 'NONE', #29635, 1000.000000000000000 ) ;
#3359 = CARTESIAN_POINT ( 'NONE',  ( -14.24874870218063450, -26.64985754041175525, 6.700000000000000178 ) ) ;
#3360 = CARTESIAN_POINT ( 'NONE',  ( 4.956441579199191594, -28.59108968528456884, 6.903372536218457256 ) ) ;
#3361 = CYLINDRICAL_SURFACE ( 'NONE', #3143, 10.00000000000000888 ) ;
#3362 = ADVANCED_FACE ( 'NONE', ( #2725 ), #36464, .F. ) ;
#3363 = ORIENTED_EDGE ( 'NONE', *, *, #8317, .T. ) ;
#3364 = DIRECTION ( 'NONE',  ( -0.000000000000000000, -0.000000000000000000, 1.000000000000000000 ) ) ;
#3365 = DIRECTION ( 'NONE',  ( -0.000000000000000000, -0.000000000000000000, -1.000000000000000000 ) ) ;
#3366 = ORIENTED_EDGE ( 'NONE', *, *, #22486, .F. ) ;
#3367 = CARTESIAN_POINT ( 'NONE',  ( 82.29396208789050604, 62.51418980721555840, -1.483157530539361391 ) ) ;
#3368 = CARTESIAN_POINT ( 'NONE',  ( 79.89218238839933406, 64.40427343574535257, 3.614403801066811361 ) ) ;
#3369 = CARTESIAN_POINT ( 'NONE',  ( 2.900770107936768039, -26.38886395563813281, 7.784838882742139532 ) ) ;
#3370 = ORIENTED_EDGE ( 'NONE', *, *, #30891, .F. ) ;
#3371 = CARTESIAN_POINT ( 'NONE',  ( 77.14378789031545125, 60.95143994403622401, -3.590981437852774238 ) ) ;
#3373 = DIRECTION ( 'NONE',  ( -1.000000000000000000, 0.000000000000000000, 0.000000000000000000 ) ) ;
#3372 = CARTESIAN_POINT ( 'NONE',  ( 2.342373490399764613, -33.01054969286393259, 7.678495282201403427 ) ) ;
#3374 = CARTESIAN_POINT ( 'NONE',  ( 14.95724209851752917, 12.36297077192868166, -2.521965761379588056 ) ) ;
#3375 = CARTESIAN_POINT ( 'NONE',  ( 80.45887431248497990, 64.72775385883045374, -3.425340496581089855 ) ) ;
#3376 = CARTESIAN_POINT ( 'NONE',  ( 77.35226663217760290, 63.40502609692227765, 3.687756614093542940 ) ) ;
#3377 = VERTEX_POINT ( 'NONE', #17918 ) ;
#3378 = EDGE_CURVE ( 'NONE', #30874, #38045, #17111, .T. ) ;
#3379 = CARTESIAN_POINT ( 'NONE',  ( -51.21549048184568420, -30.38627270959228710, 4.000000000000000000 ) ) ;
#3380 = CARTESIAN_POINT ( 'NONE',  ( 3.807509736567908032, -26.76673175688157968, 7.139344958878409919 ) ) ;
#3381 = CARTESIAN_POINT ( 'NONE',  ( 81.94850308769548519, 64.73378216408571006, 2.360008641314786715 ) ) ;
#3383 = CARTESIAN_POINT ( 'NONE',  ( 17.53685866850469566, 11.96893695421128001, 2.499999999999993339 ) ) ;
#3382 = DIRECTION ( 'NONE',  ( -0.000000000000000000, 0.000000000000000000, 1.000000000000000000 ) ) ;
#3384 = CARTESIAN_POINT ( 'NONE',  ( 30.81316972100007590, -2.191302700533721115, -5.899179390191041428 ) ) ;
#3385 = FACE_OUTER_BOUND ( 'NONE', #12096, .T. ) ;
#3386 = DIRECTION ( 'NONE',  ( 1.000000000000000000, 0.000000000000000000, 0.000000000000000000 ) ) ;
#3387 = CARTESIAN_POINT ( 'NONE',  ( 1.525564357956455730, -33.06556116538863677, 7.006908160621414972 ) ) ;
#3388 = EDGE_CURVE ( 'NONE', #36741, #20650, #2105, .T. ) ;
#3389 = B_SPLINE_CURVE_WITH_KNOTS ( 'NONE', 3,
 ( #17700, #30277, #26789, #11118, #39739, #10920, #32777, #36062, #3828, #23878 ),
 .UNSPECIFIED., .F., .F.,
 ( 4, 3, 3, 4 ),
 ( 2.168404344971008868E-19, 3.025570593003233292E-05, 6.051145698344455873E-05, 6.468151674593992863E-05 ),
 .UNSPECIFIED. ) ;
#3390 = DIRECTION ( 'NONE',  ( -0.8660254037844271613, 0.5000000000000200950, 0.000000000000000000 ) ) ;
#3391 = CARTESIAN_POINT ( 'NONE',  ( -34.24874870218063450, -26.64985754041175525, 6.800000000000000711 ) ) ;
#3392 = EDGE_CURVE ( 'NONE', #22494, #28100, #32917, .T. ) ;
#3393 = AXIS2_PLACEMENT_3D ( 'NONE', #12523, #25097, #19318 ) ;
#3394 = CARTESIAN_POINT ( 'NONE',  ( -71.92837670882107659, -0.7829914368874776320, 3.916079783099624567 ) ) ;
#3395 = CARTESIAN_POINT ( 'NONE',  ( 37.07815259682215014, -3.092164982993939049, -5.980626158107812174 ) ) ;
#3396 = DIRECTION ( 'NONE',  ( -0.000000000000000000, -1.000000000000000000, -0.000000000000000000 ) ) ;
#3397 = CARTESIAN_POINT ( 'NONE',  ( -0.8852381447421843186, -31.77776508760973684, 7.730758795053809251 ) ) ;
#3398 = LINE ( 'NONE', #34886, #229 ) ;
#3399 = CARTESIAN_POINT ( 'NONE',  ( 3.390724148067801202, -32.51998773142989307, 7.775108481317163367 ) ) ;
#3400 = CARTESIAN_POINT ( 'NONE',  ( 1.667220786302370916, -26.17008988074897857, 7.670860738520328681 ) ) ;
#3401 = B_SPLINE_CURVE_WITH_KNOTS ( 'NONE', 3,
 ( #1843, #20965, #33126, #17651 ),
 .UNSPECIFIED., .F., .F.,
 ( 4, 4 ),
 ( 0.000000000000000000, 6.391136169898815367E-06 ),
 .UNSPECIFIED. ) ;
#3402 = EDGE_CURVE ( 'NONE', #408, #14576, #40133, .T. ) ;
#3403 = CARTESIAN_POINT ( 'NONE',  ( -64.08758708074093136, 38.00013147421994830, -4.165003120434588091 ) ) ;
#3404 = CARTESIAN_POINT ( 'NONE',  ( -1.452474534483126467, -28.29735402062384253, 7.759451378593095860 ) ) ;
#3405 = CARTESIAN_POINT ( 'NONE',  ( 0.7201709579117279159, -51.60714625320436255, -2.500000000000000000 ) ) ;
#3406 = EDGE_LOOP ( 'NONE', ( #32169, #39923, #28166, #25877 ) ) ;
#3407 = LINE ( 'NONE', #12829, #3475 ) ;
#3408 = CARTESIAN_POINT ( 'NONE',  ( 68.45414103466679023, 59.01732383939346249, -3.957896739784463325 ) ) ;
#3409 = CIRCLE ( 'NONE', #26389, 24.28220113893567245 ) ;
#3410 = ORIENTED_EDGE ( 'NONE', *, *, #4155, .F. ) ;
#3411 = CARTESIAN_POINT ( 'NONE',  ( 27.43879754216082389, 0.9604377377020558715, 4.488885984917203587 ) ) ;
#3412 = CARTESIAN_POINT ( 'NONE',  ( 21.85643539959777115, -15.24623503193425123, 0.9260495571226281530 ) ) ;
#3413 = CARTESIAN_POINT ( 'NONE',  ( 22.03446123967401959, 3.769041528266752206, 4.324542679607210616 ) ) ;
#3414 = CARTESIAN_POINT ( 'NONE',  ( -37.07867591359219261, -26.64985754041175525, 6.700000000000000178 ) ) ;
#3415 = LINE ( 'NONE', #15927, #25846 ) ;
#3416 = EDGE_LOOP ( 'NONE', ( #17997, #26723 ) ) ;
#3417 = CARTESIAN_POINT ( 'NONE',  ( 24.06586850339645878, 3.348230022213010137, 3.208720231193612715 ) ) ;
#3418 = FILL_AREA_STYLE ('',( #15734 ) ) ;
#3419 = AXIS2_PLACEMENT_3D ( 'NONE', #21807, #34994, #19321 ) ;
#3420 = FACE_OUTER_BOUND ( 'NONE', #15790, .T. ) ;
#3421 = EDGE_LOOP ( 'NONE', ( #32964, #17783, #23479, #38870 ) ) ;
#3422 = CARTESIAN_POINT ( 'NONE',  ( 79.52562300987042931, 63.81209149333333386, -3.741985197832885746 ) ) ;
#3424 = LINE ( 'NONE', #12444, #7899 ) ;
#3423 = CARTESIAN_POINT ( 'NONE',  ( 27.24538128678662829, 1.201849171105237479, 4.455454704251525122 ) ) ;
#3425 = CARTESIAN_POINT ( 'NONE',  ( 78.87111998578919270, 66.14166623576272741, -1.344573736155070698 ) ) ;
#3426 = CARTESIAN_POINT ( 'NONE',  ( 78.32432613507506858, 65.79895565947732905, 1.640065189519638755 ) ) ;
#3427 = EDGE_CURVE ( 'NONE', #15456, #160, #48, .T. ) ;
#3428 = CARTESIAN_POINT ( 'NONE',  ( 79.00097698949592484, 66.21430696267364624, 1.000000000000000000 ) ) ;
#3429 = B_SPLINE_CURVE_WITH_KNOTS ( 'NONE', 3,
 ( #3195, #18385, #21897, #2367, #28265, #18797, #88, #40209, #15711, #11992, #14886, #27455, #12210, #24572, #37123, #8911, #24782, #30970, #6460 ),
 .UNSPECIFIED., .F., .F.,
 ( 4, 3, 3, 3, 3, 3, 4 ),
 ( 2.453269466693398698E-18, 2.546128104244655335E-05, 5.711050680483562714E-05, 8.113074941675540888E-05, 0.0001053129305727054790, 0.0001360598016347109565, 0.0001612931755702008360 ),
 .UNSPECIFIED. ) ;
#3430 = CARTESIAN_POINT ( 'NONE',  ( -70.92837670882107659, -27.85319909218681644, 0.000000000000000000 ) ) ;
#3431 = CARTESIAN_POINT ( 'NONE',  ( 23.92272977471906614, 4.146422156947720872, -1.204255912843045229 ) ) ;
#3432 = LINE ( 'NONE', #29125, #39737 ) ;
#3433 = ORIENTED_EDGE ( 'NONE', *, *, #18925, .F. ) ;
#3434 = CARTESIAN_POINT ( 'NONE',  ( -73.70785857967193522, 6.078230591424796714, 10.83945126441197182 ) ) ;
#3435 = CARTESIAN_POINT ( 'NONE',  ( 22.59972090504111719, 0.2729357358632942265, -6.520420251158410174 ) ) ;
#3436 = ORIENTED_EDGE ( 'NONE', *, *, #18496, .F. ) ;
#3437 = DIRECTION ( 'NONE',  ( -0.000000000000000000, -0.000000000000000000, 1.000000000000000000 ) ) ;
#3438 = CARTESIAN_POINT ( 'NONE',  ( 1.601361038683358107, -32.96850034175079003, 7.774064877406528851 ) ) ;
#3439 = CARTESIAN_POINT ( 'NONE',  ( 33.44004484032286229, -3.434887717533713580, -5.408154456503273977 ) ) ;
#3440 = CARTESIAN_POINT ( 'NONE',  ( 34.79230701455888664, -3.834676760299985165, -5.377510354588529218 ) ) ;
#3441 = CARTESIAN_POINT ( 'NONE',  ( -1.557213004826014435, -30.54360219153006284, 6.997764925645186374 ) ) ;
#3442 = DIRECTION ( 'NONE',  ( 0.6834397476448847986, 0.000000000000000000, 0.7300069255418719649 ) ) ;
#3443 = DIRECTION ( 'NONE',  ( -1.000000000000000000, 0.000000000000000000, 0.000000000000000000 ) ) ;
#3444 = CARTESIAN_POINT ( 'NONE',  ( 5.200191349065117485, -29.60785068007726650, 6.887161170156909762 ) ) ;
#3445 = DIRECTION ( 'NONE',  ( 0.000000000000000000, 0.000000000000000000, 1.000000000000000000 ) ) ;
#3446 = CARTESIAN_POINT ( 'NONE',  ( 3.481437286441587453, -32.58288071328335178, 7.697032948437506406 ) ) ;
#3447 = EDGE_CURVE ( 'NONE', #19353, #20724, #23052, .T. ) ;
#3448 = EDGE_CURVE ( 'NONE', #17630, #38045, #5583, .T. ) ;
#3449 = CARTESIAN_POINT ( 'NONE',  ( -57.16504416091206053, 33.41445838748276742, -1.000000000000000000 ) ) ;
#3450 = CARTESIAN_POINT ( 'NONE',  ( 26.04966261679769346, 1.457184003380286530, -4.328181559151514257 ) ) ;
#3451 = CARTESIAN_POINT ( 'NONE',  ( 37.19960550959731194, -2.818616413669091880, -5.999884395390916225 ) ) ;
#3452 = ADVANCED_FACE ( 'NONE', ( #2519 ), #11942, .T. ) ;
#3453 = DIRECTION ( 'NONE',  ( 0.000000000000000000, 0.000000000000000000, 1.000000000000000000 ) ) ;
#3454 = ORIENTED_EDGE ( 'NONE', *, *, #18673, .T. ) ;
#3455 = CARTESIAN_POINT ( 'NONE',  ( 67.20175956769865877, 57.92120807820956685, 3.995511504169227290 ) ) ;
#3456 = FACE_OUTER_BOUND ( 'NONE', #12785, .T. ) ;
#3457 = CARTESIAN_POINT ( 'NONE',  ( 87.44477293306643162, -1.228341977218806447, 4.926563918429203603 ) ) ;
#3458 = CARTESIAN_POINT ( 'NONE',  ( 36.75914032014244270, -2.518819990878720994, -5.943550888763135198 ) ) ;
#3459 = ORIENTED_EDGE ( 'NONE', *, *, #39750, .T. ) ;
#3460 = CARTESIAN_POINT ( 'NONE',  ( 24.39461023293930708, 2.846075433827604861, 3.813165204976378231 ) ) ;
#3461 = DIRECTION ( 'NONE',  ( -0.1736481776669268062, 0.9848077530122086864, 0.000000000000000000 ) ) ;
#3462 = ORIENTED_EDGE ( 'NONE', *, *, #26675, .T. ) ;
#3463 = ORIENTED_EDGE ( 'NONE', *, *, #19206, .F. ) ;
#3464 = CARTESIAN_POINT ( 'NONE',  ( 79.94486516293694933, 63.68863865526427759, -3.714073935154548423 ) ) ;
#3465 = LINE ( 'NONE', #15792, #21382 ) ;
#3466 = CARTESIAN_POINT ( 'NONE',  ( 78.57794565308397239, 65.91709162046863923, 1.743126864185328806 ) ) ;
#3467 = ORIENTED_EDGE ( 'NONE', *, *, #10335, .T. ) ;
#3468 = CARTESIAN_POINT ( 'NONE',  ( -59.01947560891952804, 27.90920910948504385, 6.147301388271928957 ) ) ;
#3469 = CARTESIAN_POINT ( 'NONE',  ( -70.92837670882107659, -56.35932253828836025, 0.000000000000000000 ) ) ;
#3470 = CARTESIAN_POINT ( 'NONE',  ( -66.83699642652008777, 37.05199716444892744, -9.800414904976365804 ) ) ;
#3471 = CARTESIAN_POINT ( 'NONE',  ( -55.16612787639756732, 31.23053227951973199, 1.484562114140385747 ) ) ;
#3472 = CARTESIAN_POINT ( 'NONE',  ( 22.88456325795406698, 4.291280149456187409, -3.119280959484842075 ) ) ;
#3473 = ORIENTED_EDGE ( 'NONE', *, *, #26327, .F. ) ;
#3474 = CARTESIAN_POINT ( 'NONE',  ( 1.121324086407811338, -24.55319635012989110, 6.700000000000000178 ) ) ;
#3475 = VECTOR ( 'NONE', #38338, 1000.000000000000000 ) ;
#3476 = ORIENTED_EDGE ( 'NONE', *, *, #11914, .F. ) ;
#3477 = CARTESIAN_POINT ( 'NONE',  ( -16.44874870218064089, -26.64985754041175525, 6.800000000000000711 ) ) ;
#3478 = LINE ( 'NONE', #33592, #20811 ) ;
#3479 = CARTESIAN_POINT ( 'NONE',  ( -80.68571131495720294, -5.697267497185621643, -2.227797487936516774 ) ) ;
#3480 = AXIS2_PLACEMENT_3D ( 'NONE', #28312, #12661, #22155 ) ;
#3481 = PLANE ( 'NONE',  #29434 ) ;
#3482 = DIRECTION ( 'NONE',  ( 0.6159927814537400348, 0.7877517966954343809, -0.000000000000000000 ) ) ;
#3483 = CARTESIAN_POINT ( 'NONE',  ( 81.24880315266035780, 62.88501018724376479, 3.211742283750890437 ) ) ;
#3484 = CARTESIAN_POINT ( 'NONE',  ( 87.12371845299759343, -1.516527252418922833, -4.675789953527256237 ) ) ;
#3485 = CARTESIAN_POINT ( 'NONE',  ( 21.67219544786406260, 6.675102098148268936, -3.070833163645317221 ) ) ;
#3486 = ORIENTED_EDGE ( 'NONE', *, *, #17233, .F. ) ;
#3487 = CARTESIAN_POINT ( 'NONE',  ( -2.503969810797764151, -28.81487718949574983, 7.635761828346577573 ) ) ;
#3488 = DIRECTION ( 'NONE',  ( -0.9267318687906784813, 0.3757233601570931225, 0.000000000000000000 ) ) ;
#3489 = EDGE_CURVE ( 'NONE', #513, #650, #9901, .T. ) ;
#3490 = CARTESIAN_POINT ( 'NONE',  ( 1.822194502883781375, -26.17211269480022295, 7.754798119455333705 ) ) ;
#3491 = CARTESIAN_POINT ( 'NONE',  ( -0.7974450458313169232, -25.21654760013375451, 7.635761828346577573 ) ) ;
#3492 = EDGE_CURVE ( 'NONE', #31820, #30682, #34836, .T. ) ;
#3493 = CARTESIAN_POINT ( 'NONE',  ( -2.978675913592195190, -26.64985754041175525, 6.800000000000000711 ) ) ;
#3494 = CARTESIAN_POINT ( 'NONE',  ( -8.348748702180635917, -26.64985754041175525, 6.700000000000000178 ) ) ;
#3495 = ORIENTED_EDGE ( 'NONE', *, *, #811, .T. ) ;
#3496 = CARTESIAN_POINT ( 'NONE',  ( 30.51435440191163195, -0.1427370434214647044, 4.968901015505058361 ) ) ;
#3497 = CARTESIAN_POINT ( 'NONE',  ( 86.96272348114096928, 0.6770660828398197273, -5.145113290124521122 ) ) ;
#3498 = ORIENTED_EDGE ( 'NONE', *, *, #20216, .T. ) ;
#3500 = CARTESIAN_POINT ( 'NONE',  ( 0.01899362242916388319, 0.5999999999999995337, 3.829601239880993990 ) ) ;
#3499 = CARTESIAN_POINT ( 'NONE',  ( 78.66788830423078593, 66.04261347698268025, -1.159471704397126102 ) ) ;
#3501 = CARTESIAN_POINT ( 'NONE',  ( 2.927923484755866834, -32.84760645976612636, 7.670465701733751196 ) ) ;
#3502 = CARTESIAN_POINT ( 'NONE',  ( 21.63674184841064019, 6.916893520949614071, -2.999760302877421125 ) ) ;
#3503 = ORIENTED_EDGE ( 'NONE', *, *, #2976, .T. ) ;
#3504 = FACE_OUTER_BOUND ( 'NONE', #26138, .T. ) ;
#3505 = ORIENTED_EDGE ( 'NONE', *, *, #6051, .T. ) ;
#3506 = CARTESIAN_POINT ( 'NONE',  ( -72.89233069014277078, -2.171328805845720300, 9.806946677974712756 ) ) ;
#3507 = VERTEX_POINT ( 'NONE', #34632 ) ;
#3508 = CARTESIAN_POINT ( 'NONE',  ( 81.13710691025120525, 61.43629694585947476, -1.911132874451710650 ) ) ;
#3509 =( BOUNDED_CURVE ( )  B_SPLINE_CURVE ( 3, ( #29605, #26523, #39058, #13348 ),
 .UNSPECIFIED., .F., .T. ) 
 B_SPLINE_CURVE_WITH_KNOTS ( ( 4, 4 ),
 ( 4.748221474220560623, 4.941946782021394924 ),
 .UNSPECIFIED. ) 
 CURVE ( )  GEOMETRIC_REPRESENTATION_ITEM ( )  RATIONAL_B_SPLINE_CURVE ( ( 1.000000000000000000, 0.9968749865767494445, 0.9968749865767494445, 1.000000000000000000 ) ) 
 REPRESENTATION_ITEM ( '' )  );
#3510 = CARTESIAN_POINT ( 'NONE',  ( -63.08758708074093136, 36.14363715547679590, -3.800414904976364472 ) ) ;
#3511 = ADVANCED_FACE ( 'NONE', ( #40553 ), #31521, .T. ) ;
#3513 = CARTESIAN_POINT ( 'NONE',  ( 36.44317183454039366, -1.735355048105241549, 5.732832347747111257 ) ) ;
#3512 = CARTESIAN_POINT ( 'NONE',  ( 22.03874921663882347, 2.012712906550705227, 5.777197709026360428 ) ) ;
#3515 = ORIENTED_EDGE ( 'NONE', *, *, #21679, .T. ) ;
#3514 = VERTEX_POINT ( 'NONE', #19366 ) ;
#3516 = CARTESIAN_POINT ( 'NONE',  ( 80.07729437284001506, 66.15382583937143579, -2.040045296073660808 ) ) ;
#3517 = CARTESIAN_POINT ( 'NONE',  ( 4.743949789439241727, -28.05442871495747781, 6.969307238440504371 ) ) ;
#3519 = CARTESIAN_POINT ( 'NONE',  ( 85.76835188082283423, 2.018640952613007578, 3.843583708408826904 ) ) ;
#3518 = CARTESIAN_POINT ( 'NONE',  ( 4.546323995280799224, -31.43022402557198092, 6.895222827070023541 ) ) ;
#3520 = CARTESIAN_POINT ( 'NONE',  ( -63.33907144938095968, 42.38509300232142607, -3.755920398012963624 ) ) ;
#3521 = CARTESIAN_POINT ( 'NONE',  ( 69.60281991352538000, 59.48300438377392396, 3.944663542062654571 ) ) ;
#3522 = EDGE_LOOP ( 'NONE', ( #10649, #29613, #27923, #18259, #9021, #12100 ) ) ;
#3523 = CARTESIAN_POINT ( 'NONE',  ( 22.98570178199580738, 3.657932872642362998, -3.680547506993712581 ) ) ;
#3524 = VERTEX_POINT ( 'NONE', #3742 ) ;
#3525 = CARTESIAN_POINT ( 'NONE',  ( 21.85643539959773207, -2.370478073490382531, -12.58538558043069600 ) ) ;
#3526 = B_SPLINE_CURVE_WITH_KNOTS ( 'NONE', 3,
 ( #11962, #59, #31341, #22081, #252, #35256, #7025, #25770, #25564, #37689, #12791, #21867, #38307, #3369, #9912, #19387, #10103, #32168, #6222, #28654, #28233, #13000, #22691, #12588, #29060 ),
 .UNSPECIFIED., .F., .F.,
 ( 4, 3, 3, 3, 3, 3, 3, 3, 4 ),
 ( 6.468151674593313881E-05, 9.076621574722140316E-05, 0.0001210204262067985899, 0.0001512763324577444867, 0.0001815301820994240866, 0.0002117781465860715459, 0.0002420274594459770508, 0.0002722905548971173064, 0.0002816827545175549933 ),
 .UNSPECIFIED. ) ;
#3527 = CARTESIAN_POINT ( 'NONE',  ( 16.09990961988968294, 15.28674628019743942, 3.774899269766986531 ) ) ;
#3528 = CARTESIAN_POINT ( 'NONE',  ( 11.65737507970504439, -29.56993018339339940, 6.000000000000000000 ) ) ;
#3529 = CARTESIAN_POINT ( 'NONE',  ( 81.76814852625392405, 62.80907675923856459, 2.758880570191250658 ) ) ;
#3530 = CARTESIAN_POINT ( 'NONE',  ( 85.43834401013396018, 2.333645700298356829, -4.102255839672300120 ) ) ;
#3531 = ORIENTED_EDGE ( 'NONE', *, *, #10084, .T. ) ;
#3532 = CARTESIAN_POINT ( 'NONE',  ( -81.82396199936634673, -5.600653810444165437, 0.2120607140719947270 ) ) ;
#3533 = CARTESIAN_POINT ( 'NONE',  ( 33.95295690078342687, -3.700853304509699182, 5.336167209958794899 ) ) ;
#3534 = ADVANCED_FACE ( 'NONE', ( #16066 ), #227, .T. ) ;
#3535 = CARTESIAN_POINT ( 'NONE',  ( 27.40776759654589156, 0.9655315125819244892, -4.484043011441926296 ) ) ;
#3536 = CARTESIAN_POINT ( 'NONE',  ( 5.099204911771554549, -29.65969559590484650, 7.778050822775633755 ) ) ;
#3537 = CARTESIAN_POINT ( 'NONE',  ( -1.343629279779518182, -27.84251741988426687, 7.737115613922535218 ) ) ;
#3538 = CARTESIAN_POINT ( 'NONE',  ( -75.86661230596840255, -3.880840061887903758, 10.12747849425165647 ) ) ;
#3539 = DIRECTION ( 'NONE',  ( 0.000000000000000000, 0.000000000000000000, -1.000000000000000000 ) ) ;
#3540 = CARTESIAN_POINT ( 'NONE',  ( 3.852146645688039328, -32.33035474113215457, 7.750000000000000888 ) ) ;
#3541 = CIRCLE ( 'NONE', #10089, 0.1000000000000028644 ) ;
#3542 = CIRCLE ( 'NONE', #2925, 31.02204673211315011 ) ;
#3543 = CARTESIAN_POINT ( 'NONE',  ( 33.45304404609620263, -3.772033185430891500, 5.158132413726952414 ) ) ;
#3544 = ORIENTED_EDGE ( 'NONE', *, *, #35578, .F. ) ;
#3545 = ORIENTED_EDGE ( 'NONE', *, *, #17006, .F. ) ;
#3546 = CARTESIAN_POINT ( 'NONE',  ( 36.68438008943704887, -1.916626965623605683, 5.804116225272221818 ) ) ;
#3547 = LINE ( 'NONE', #25755, #31053 ) ;
#3548 = CARTESIAN_POINT ( 'NONE',  ( 66.56200747226770886, 57.85618981312373421, -3.999874661883399352 ) ) ;
#3549 = VERTEX_POINT ( 'NONE', #28836 ) ;
#3550 = CARTESIAN_POINT ( 'NONE',  ( -57.76433750236255804, 32.39122475941741186, 4.160719226838292428 ) ) ;
#3551 = LINE ( 'NONE', #1219, #16039 ) ;
#3552 = CARTESIAN_POINT ( 'NONE',  ( 4.958069736096009095, -28.59650564702042885, 6.911401339314955372 ) ) ;
#3553 = DIRECTION ( 'NONE',  ( 1.000000000000000000, 0.000000000000000000, 0.000000000000000000 ) ) ;
#3554 = VERTEX_POINT ( 'NONE', #34224 ) ;
#3555 = CARTESIAN_POINT ( 'NONE',  ( -70.92837670882107659, -23.80776546975053165, 10.00000000000001066 ) ) ;
#3556 = VERTEX_POINT ( 'NONE', #37877 ) ;
#3557 = CARTESIAN_POINT ( 'NONE',  ( 23.70115564627849736, 3.489872147238937128, 3.358116645522415844 ) ) ;
#3558 = CARTESIAN_POINT ( 'NONE',  ( 79.68325118717125122, 66.33239387230217687, -1.129532193886523261 ) ) ;
#3559 = CARTESIAN_POINT ( 'NONE',  ( 80.91173626137351960, 62.16536564854140323, 2.996423812020193367 ) ) ;
#3560 = CARTESIAN_POINT ( 'NONE',  ( -72.46964309959683703, 39.11862660440054640, 12.50000000000000000 ) ) ;
#3561 = VERTEX_POINT ( 'NONE', #9687 ) ;
#3562 = CARTESIAN_POINT ( 'NONE',  ( 75.65523814419378823, 61.17064132828575396, -3.882889210543257974 ) ) ;
#3564 = CARTESIAN_POINT ( 'NONE',  ( 0.000000000000000000, -0.6000000000000003109, 3.730072921939604047 ) ) ;
#3563 = CARTESIAN_POINT ( 'NONE',  ( -71.41272068158380648, -45.69399732294015593, 5.981110394793661023 ) ) ;
#3565 = CARTESIAN_POINT ( 'NONE',  ( 17.35526930789154676, 8.837536743741704726, -2.915107532907570853 ) ) ;
#3566 = EDGE_CURVE ( 'NONE', #2799, #10884, #18442, .T. ) ;
#3567 = CARTESIAN_POINT ( 'NONE',  ( 79.87861596566074240, 65.47018085071597682, -3.015642068896328798 ) ) ;
#3568 = CARTESIAN_POINT ( 'NONE',  ( 75.66308047697211236, 62.61957414976296121, 3.723120700747973633 ) ) ;
#3569 = ORIENTED_EDGE ( 'NONE', *, *, #24702, .F. ) ;
#3570 = EDGE_LOOP ( 'NONE', ( #27467, #36982, #29080, #9143, #27593 ) ) ;
#3571 = ADVANCED_FACE ( 'NONE', ( #12151 ), #9216, .T. ) ;
#3572 = VECTOR ( 'NONE', #28694, 1000.000000000000000 ) ;
#3573 = CARTESIAN_POINT ( 'NONE',  ( 1.728294629719529185, -26.08119623175329593, 7.781480525794719050 ) ) ;
#3574 = CIRCLE ( 'NONE', #4234, 0.1000000000000028644 ) ;
#3575 = DIRECTION ( 'NONE',  ( 0.000000000000000000, 0.000000000000000000, 1.000000000000000000 ) ) ;
#3576 = CARTESIAN_POINT ( 'NONE',  ( 82.11700085695696316, 62.19713100941785200, 1.465650077276457131 ) ) ;
#3578 = CARTESIAN_POINT ( 'NONE',  ( 17.42606411499827601, 12.01804255755900463, 2.499999999999993339 ) ) ;
#3577 = CARTESIAN_POINT ( 'NONE',  ( -0.1307851662454839470, -32.55269768341421610, 6.863805608295729499 ) ) ;
#3579 = CARTESIAN_POINT ( 'NONE',  ( 29.64656804624054942, -2.931097914703496787, 5.165983120431130615 ) ) ;
#3580 = CARTESIAN_POINT ( 'NONE',  ( -1.415111900810474443, -31.16482645844592625, 6.903112506833888773 ) ) ;
#3581 = CARTESIAN_POINT ( 'NONE',  ( -63.58520484588291311, 35.72026407271198423, 6.999999999999986677 ) ) ;
#3582 = CIRCLE ( 'NONE', #34496, 9.386006772603931125 ) ;
#3583 = FACE_OUTER_BOUND ( 'NONE', #12150, .T. ) ;
#3584 = ORIENTED_EDGE ( 'NONE', *, *, #25760, .T. ) ;
#3585 = CARTESIAN_POINT ( 'NONE',  ( 1.665108719337590415, -26.07010776075642511, 7.707984471951055738 ) ) ;
#3586 = DIRECTION ( 'NONE',  ( 0.000000000000000000, 0.000000000000000000, 1.000000000000000000 ) ) ;
#3587 = FACE_OUTER_BOUND ( 'NONE', #7625, .T. ) ;
#3588 = EDGE_CURVE ( 'NONE', #32059, #27620, #29230, .T. ) ;
#3589 = CARTESIAN_POINT ( 'NONE',  ( 33.75541762379567245, -0.8753173094601959248, -5.454573668235052963 ) ) ;
#3590 = AXIS2_PLACEMENT_3D ( 'NONE', #23486, #17281, #20381 ) ;
#3591 = CARTESIAN_POINT ( 'NONE',  ( 4.944078209288079506, -30.88464969939810345, 7.750000000000000888 ) ) ;
#3592 = CARTESIAN_POINT ( 'NONE',  ( -0.9721080757342911438, -31.67178857246723211, 7.768425012602590662 ) ) ;
#3593 = CARTESIAN_POINT ( 'NONE',  ( 1.713892699967800581, -32.96990337146582561, 7.635761828346577573 ) ) ;
#3594 = CARTESIAN_POINT ( 'NONE',  ( 1.664433243520564876, -26.17012032033359148, 7.693875151218753317 ) ) ;
#3595 = DIRECTION ( 'NONE',  ( -0.9594800004753906153, -0.2817767355331954326, 0.000000000000000000 ) ) ;
#3596 = CARTESIAN_POINT ( 'NONE',  ( 22.02701111391718314, -11.57978826329849475, 2.500000000000000444 ) ) ;
#3597 = CARTESIAN_POINT ( 'NONE',  ( 8.290806648384990041, -35.94265729135299381, -6.000000000000000000 ) ) ;
#3598 = VERTEX_POINT ( 'NONE', #23066 ) ;
#3599 = DIRECTION ( 'NONE',  ( 0.000000000000000000, -0.7126435865141248494, 0.7015262779114442848 ) ) ;
#3600 = CARTESIAN_POINT ( 'NONE',  ( 68.61500287773905882, 58.59333675578601230, -3.993768376023893563 ) ) ;
#3601 = EDGE_LOOP ( 'NONE', ( #37257, #11839, #2804, #30674 ) ) ;
#3602 = CIRCLE ( 'NONE', #30524, 27.95745752244933158 ) ;
#3603 = AXIS2_PLACEMENT_3D ( 'NONE', #15289, #14464, #24558 ) ;
#3604 = CARTESIAN_POINT ( 'NONE',  ( 1.700390093233090871, -29.56993018339339940, 7.800000000000000711 ) ) ;
#3605 = CARTESIAN_POINT ( 'NONE',  ( 30.79191905210313251, -3.554283433601253428, 4.832056180595072803 ) ) ;
#3606 = CARTESIAN_POINT ( 'NONE',  ( 22.23240669476004783, 3.462061741365346279, 4.374547872445481822 ) ) ;
#3607 = DIRECTION ( 'NONE',  ( 1.000000000000000000, 3.965082230804130614E-15, 0.000000000000000000 ) ) ;
#3608 = DIRECTION ( 'NONE',  ( 1.000000000000000000, 0.000000000000000000, 0.000000000000000000 ) ) ;
#3609 = ORIENTED_EDGE ( 'NONE', *, *, #7770, .T. ) ;
#3610 = CARTESIAN_POINT ( 'NONE',  ( -1.635225080001443621, -33.52415522258557701, 7.635761828346577573 ) ) ;
#3611 = AXIS2_PLACEMENT_3D ( 'NONE', #8446, #26995, #5378 ) ;
#3612 = CARTESIAN_POINT ( 'NONE',  ( 81.27646189173411528, 61.63998710316791829, 2.098997056522959426 ) ) ;
#3613 = EDGE_LOOP ( 'NONE', ( #15107, #25975, #24061, #17576 ) ) ;
#3614 = DIRECTION ( 'NONE',  ( -1.000000000000000000, 0.000000000000000000, 0.000000000000000000 ) ) ;
#3615 = ORIENTED_EDGE ( 'NONE', *, *, #37587, .T. ) ;
#3616 = CARTESIAN_POINT ( 'NONE',  ( 80.55759259636404579, 61.16327383424329156, -2.033355767895908883 ) ) ;
#3618 = CARTESIAN_POINT ( 'NONE',  ( -1.659981793545334039, -30.08761321148581658, 6.874555630061442102 ) ) ;
#3617 = CARTESIAN_POINT ( 'NONE',  ( 21.81113558402230268, 0.2595215699418438327, 8.250542685949572075 ) ) ;
#3619 = ADVANCED_FACE ( 'NONE', ( #4724 ), #36028, .F. ) ;
#3620 = CARTESIAN_POINT ( 'NONE',  ( 81.28907188958018537, 64.38987696229560243, -3.179853676209052793 ) ) ;
#3621 = CARTESIAN_POINT ( 'NONE',  ( 78.62541471602109766, 65.39282990155331277, 2.732428818688203087 ) ) ;
#3622 = ORIENTED_EDGE ( 'NONE', *, *, #38845, .F. ) ;
#3623 = EDGE_CURVE ( 'NONE', #33723, #7222, #28297, .T. ) ;
#3624 = B_SPLINE_SURFACE_WITH_KNOTS ( 'NONE', 3, 3, ( 
 ( #36799, #3428, #6280, #34505, #15539, #28298, #22550, #19043, #33730, #18052, #31199, #40646, #12449, #25018, #37555, #3227, #15745, #118, #19242, #31605, #25224, #37752, #25422, #3625, #22351 ),
 ( #6694, #29321, #720, #35319, #38364, #38568, #35711, #7691, #7086, #10966, #1138, #19447, #39168, #10161, #20238, #17143, #38964, #6891, #32822, #19651, #7487, #16735, #13670, #3826, #4613 ),
 ( #14058, #28917, #10569, #22752, #13459, #1334, #35113, #29122, #32626, #32222, #4024, #26438, #20046, #925, #26240, #16542, #29523, #26034, #32020, #10763, #10374, #16943, #26634, #29715, #22950 ),
 ( #38774, #4421, #16344, #13261, #13871, #25827, #35513, #23340, #1524, #35912, #7284, #19847, #32417, #4215, #23143, #11563, #36908, #23733, #27438, #2138, #14657, #26833, #27636, #2554, #24139 ),
 ( #36700, #14866, #17747, #23930, #8483, #1731, #27228, #21065, #33639, #21268, #39994, #39372, #18159, #39794, #5414, #20439, #36303, #17952, #30126, #8076, #30536, #30753, #2347, #11764, #24345 ),
 ( #8689, #15077, #5210, #30332, #27033, #23546, #33841, #5619, #39578, #40194, #36110, #7888, #33019, #11163, #4807, #17336, #11363, #29913, #14262, #20639, #33221, #5007, #17538, #1941, #14460 ),
 ( #36502, #8274, #20848, #33440, #2758, #11974, #40390, #12192, #24761, #24552, #8892, #37915, #24971, #18367, #37106, #6646, #9105, #15695, #22092, #21475, #3576, #34667, #15284, #37309, #12604 ),
 ( #16103, #25170, #34053, #5826, #30954, #71, #25376, #21682, #15897, #31355, #3181, #27836, #28669, #31760, #37702, #37508, #12805, #34260, #28458, #12403, #6031, #31558, #265, #18565, #9722 ),
 ( #22303, #31152, #19197, #28247, #9510, #2968, #15486, #6445, #28045, #40596, #18997, #9303, #3381, #34870, #21880, #34458, #6234, #18778, #879, #10520, #9924, #38318, #16895, #25782, #22900 ),
 ( #13015, #25577, #22506, #16301, #32374, #26193, #29073, #4373, #35667, #13825, #31972, #19803, #32779, #26394, #13216, #35866, #6842, #22703, #38122, #38725, #19996, #32578, #35070, #13618, #4568 ),
 ( #23295, #7644, #38924, #23100, #10115, #13411, #19400, #10716, #25986, #3777, #35271, #28869, #20193, #676, #16688, #7038, #19606, #7435, #475, #32180, #29475, #3977, #16496, #1288, #17095 ),
 ( #38518, #10322, #35468, #7240, #4172, #29275, #1087, #1480, #39125, #4758, #20800, #14610, #17488, #33593, #24088, #2294, #20391, #8229, #21219, #14820, #1686, #24298, #36064, #11120, #26586 ),
 ( #32973, #29668, #17292, #7843, #39330, #30081, #11723, #36859, #27386, #2094, #14216, #1896, #10922, #39947, #14418, #29870, #23689, #26791, #8644, #23498, #5165, #36255, #8032, #36656, #14014 ),
 ( #23880, #20590, #26986, #8435, #33790, #5570, #33175, #30279, #4962, #39532, #11314, #36454, #33393, #17701, #27182, #39742, #11521, #21017, #5368, #17906, #30488, #9673, #28197, #8845, #5778 ),
 ( #31311, #22258, #3133, #40147, #15033, #27594, #6187, #31511, #18316, #22044, #37461, #9257, #21430, #34826, #37869, #18731, #2918, #18946, #27789, #34622, #18522, #18109, #37657, #6395, #30907 ),
 ( #15851, #3335, #34004, #12756, #34414, #21837, #11929, #2715, #15651, #24714, #15236, #27, #25334, #12555, #28409, #216, #9459, #40344, #30703, #31106, #25127, #24505, #12138, #37057, #2509 ),
 ( #37262, #21632, #9055, #34213, #5983, #15438, #12353, #27998, #40542, #24925, #4325, #13778, #428, #7194, #6797, #19351, #6602, #3529, #32525, #19561, #12968, #19147, #1242, #3731, #10275 ),
 ( #19754, #16053, #19946, #29028, #10072, #16846, #25534, #38276, #3937, #32332, #22656, #13362, #38078, #28826, #7392, #4128, #26346, #38471, #35620, #10670, #38878, #25937, #22853, #35425, #16641 ),
 ( #6996, #23251, #26143, #29428, #31922, #31713, #831, #16255, #29226, #35224, #1039, #9880, #28622, #22454, #35023, #632, #13173, #25733, #32137, #13571, #38677, #16454, #10474, #23055, #20962 ),
 ( #5113, #4523, #32921, #11468, #20342, #17436, #1629, #14168, #20539, #30026, #30230, #33543, #36405, #39072, #14364, #13969, #32727, #2044, #17043, #33338, #36204, #23637, #4712, #1841, #14765 ),
 ( #20748, #27133, #39684, #29622, #8176, #39897, #10871, #8385, #17853, #24036, #7595, #5319, #7790, #17649, #26932, #39477, #1436, #30434, #20147, #7983, #27337, #36607, #2244, #36012, #11671 ),
 ( #23447, #35817, #11264, #23828, #26537, #17245, #26740, #39279, #11067, #33124, #4904, #15390, #40705, #28151, #15599, #37009, #34572, #24659, #34366, #33737, #21373, #12506, #8791, #5932, #18265 ),
 ( #36809, #5517, #40096, #27946, #9208, #12085, #25081, #18677, #37611, #14983, #2867, #15808, #9407, #33952, #18896, #30650, #5727, #21172, #21788, #3080, #21995, #18059, #37412, #28362, #27543 ),
 ( #6346, #31463, #6136, #30857, #37211, #2462, #3286, #9004, #11877, #2664, #24452, #175, #15183, #40488, #27742, #40295, #31263, #24245, #21584, #8594, #34166, #18471, #31056, #12300, #24873 ),
 ( #13312, #12916, #25482, #12711, #9621, #38632, #25683, #19098, #25285, #7342, #9830, #16404, #22808, #22208, #4272, #35378, #3483, #380, #25885, #10431, #38424, #16795, #10225, #34775, #6553 ),
 ( #34976, #13523, #7147, #32474, #3889, #987, #29376, #19901, #32084, #19509, #28978, #19707, #4082, #782, #29178, #16596, #26094, #38028, #23006, #13124, #32282, #31667, #22406, #35573, #6751 ),
 ( #37816, #16008, #28573, #19301, #31872, #3683, #16207, #585, #28778, #38226, #10023, #22606, #35174, #6947, #36362, #29574, #33283, #35769, #26492, #26296, #20492, #14316, #26886, #10622, #33074 ),
 ( #20291, #5064, #17597, #23783, #4858, #1390, #32874, #38828, #8129, #4664, #7543, #39017, #20098, #30177, #23197, #23597, #32675, #10821, #1787, #1196, #23397, #17391, #13921, #4476, #39427 ),
 ( #26692, #35962, #11217, #7743, #13733, #14516, #39227, #1998, #16998, #17200, #20700, #29767, #1582, #14113, #11016, #36161, #29972, #7940, #19639, #711, #10556, #3612, #28905, #35304, #22939 ),
 ( #34908, #26022, #23132, #38154, #1126, #16531, #29109, #516, #1321, #16934, #38553, #22740, #38763, #6881, #13659, #38354, #29511, #16723, #26228, #9958, #35700, #32213, #19434, #10363, #13248 ),
 ( #913, #6682, #22540, #35501, #3814, #35102, #13449, #32613, #7473, #25817, #7274, #20032, #10151, #7075, #19837, #19231, #4409, #4014, #32409, #13860, #16141, #4203, #29310, #37952, #9759 ),
 ( #32009, #22339, #31797, #28702, #13047, #25610, #16331, #33626, #4996, #33211, #1926, #27020, #17730, #20625, #26821, #14449, #4601, #17521, #39566, #36492, #24123, #30317, #29703, #21054, #11350 ),
 ( #8470, #5401, #20427, #36690, #2332, #38955, #30117, #20833, #27217, #17324, #29904, #11552, #17941, #8064, #23914, #1718, #26426, #2127, #30522, #14248, #10749, #23330, #35899, #7677, #1514 ),
 ( #14047, #8262, #17129, #20229, #33429, #32812, #5198, #39360, #11152, #36100, #14644, #26622, #39779, #39157, #10952, #23535, #7877, #33005, #4794, #23722, #36288, #37688, #9493, #28231, #28032 ),
 ( #15471, #37296, #9093, #24332, #58, #39982, #21666, #21255, #15065, #18148, #18352, #40578, #12587, #27623, #31545, #34245, #11754, #40372, #9289, #25154, #22080, #8674, #12389, #40180, #11961 ),
 ( #34654, #27820, #33826, #6425, #18983, #5609, #24957, #24537, #37092, #14853, #36896, #27421, #12177, #30736, #2541, #8881, #21463, #18552, #37492, #34039, #5812, #21866, #30940, #2746, #34443 ),
 ( #15269, #24747, #6220, #6016, #31136, #2955, #18766, #15682, #31340, #3166, #35797, #32904, #7967, #11048, #23231, #10652, #20128, #4505, #35993, #38861, #4306, #32710, #22288, #7575, #17027 ),
 ( #12998, #29602, #7371, #1417, #34857, #20518, #26720, #23623, #38107, #14147, #3368, #15884, #13953, #39052, #4694, #35055, #19928, #29800, #36187, #26324, #26519, #32506, #28443, #7774, #1612 ),
 ( #22491, #29412, #10851, #23428, #39257, #20322, #6634, #17226, #19181, #251, #12788, #25364, #37901, #16828, #1226, #25563, #9708, #31746, #3559, #16087, #28653, #460, #9911, #13760, #11245 ),
 ( #5708, #15165, #36993, #4887, #18250, #5094, #33719, #14745, #27316, #1821, #30838, #17418, #39876, #39456, #33314, #36385, #36590, #5498, #2648, #17627, #8984, #11653, #30003, #17833, #27529 ),
 ( #14343, #24228, #23809, #30207, #8157, #8367, #18041, #27723, #2024, #33102, #36789, #26914, #30416, #40081, #40278, #12064, #20729, #30634, #14540, #27114, #39664, #11448, #24643, #5296, #24014 ),
 ( #20939, #8574, #2442, #33525, #37194, #14964, #2223, #21153, #11859, #24435, #8773, #21360, #33934, #2849, #18456, #31042, #9604, #34956, #21768, #25464, #158, #12691, #24857, #25664, #567 ),
 ( #22391, #31245, #38009, #21977, #13105, #362, #9811, #34351, #6733, #15793, #3066, #22187, #25061, #37800, #40472, #38206, #3665, #28757, #15582, #31850, #21570, #34148, #25267, #15984, #19283 ),
 ( #6121, #16192, #34554, #31650, #15370, #18656, #5916, #28137, #3268, #40689, #12494, #6326, #28344, #28551, #27928, #34761, #37398, #6535, #12281, #9193, #12899, #37595, #19082, #18874, #9392 ),
 ( #31446, #3466, #6929, #35750, #29556, #1376, #3870, #23180, #14097, #13294, #23379, #32861, #13907, #22589, #35947, #22789, #10607, #32455, #4255, #16386, #7524, #10207, #35357, #10006, #19491 ),
 ( #1567, #7729, #26077, #1180, #4650, #10414, #7325, #20085, #28960, #20276, #16780, #13505, #17183, #763, #968, #29360, #32663, #38610, #13714, #25867, #32265, #10801, #4462, #29752, #26280 ),
 ( #26676, #35157, #38814, #35557, #38406, #19689, #26475, #22990, #7129, #39003, #4063, #16578, #29159, #16984, #8113, #39841, #1983, #14701, #17376, #15124, #21316, #5668, #33267, #8733, #39211 ),
 ( #30379, #14920, #2395, #30588, #11205, #33888, #39624, #8531, #7927, #36345, #27488, #23769, #20896, #5050, #17581, #23970, #33483, #33681, #24395, #11610, #1771, #17793, #29957, #36147, #5461 ),
 ( #30797, #11811, #20682, #18205, #4845, #30163, #20476, #24189, #18002, #40038, #33058, #36745, #2605, #14300, #36953, #10999, #23583, #26868, #39414, #14503, #21113, #5253, #2183, #27079, #11404 ),
 ( #36545, #8322, #27270, #31000, #6075, #34713, #27680, #21723, #25221, #27882, #2803, #19041, #12647, #34306, #21928, #19240, #25420, #3015, #18825, #9767, #28092, #25013, #115, #37151, #314 ),
 ( #12851, #5874, #18608, #37552, #37751, #31196, #34502, #21525, #9147, #28502, #9556, #6692, #31397, #15937, #31806, #34917, #6277, #3226, #15742, #28294, #31603, #22141, #40643, #6489, #18412 ),
 ( #3426, #37961, #22347, #15328, #3621, #40237, #12020, #24597, #40427, #8940, #15535, #12238, #24812, #37353, #12446, #9347, #20040, #7483, #28913, #26435, #16539, #26238, #25618, #13256, #32621 ),
 ( #32219, #10758, #28711, #523, #38161, #32017, #7281, #1134, #4022, #4417, #10566, #29519, #6888, #35509, #7687, #1330, #718, #23337, #22548, #38361, #13057, #13666, #35708, #16941, #9967 ),
 ( #25825, #29116, #38962, #35906, #13867, #29317, #10158, #922, #35110, #20236, #13457, #19442, #22747, #3824, #32819, #16341, #32416, #35314, #7082, #23140, #16148, #19649, #38770, #26029, #38561 ),
 ( #10371, #22947, #19846, #16732, #4211, #4802, #4608, #1522, #30531, #17948, #17333, #39990, #10960, #26828, #14055, #30326, #24133, #36697, #26631, #17738, #8681, #7885, #2341, #27431, #8478 ),
 ( #29911, #5004, #39164, #14862, #17530, #23543, #39369, #36108, #24340, #20434, #20842, #33015, #23730, #11559, #17139, #11159, #2134, #1727, #14257, #21061, #14652, #36297, #39573, #8073, #39789 ),
 ( #29712, #20633, #11761, #30124, #33219, #1936, #36904, #14457, #8270, #27224, #27029, #21263, #33633, #11357, #23925, #5207, #36499, #5409, #33436, #6229, #15074, #30747, #2549, #21875, #6436 ),
 ( #12398, #24967, #37102, #37910, #12799, #34453, #18560, #34663, #2754, #9505, #34253, #25372, #12597, #22088, #34048, #18992, #28041, #15278, #18774, #37304, #9297, #11970, #9716, #15892, #259 ),
 ( #5822, #31348, #28452, #37502, #31553, #37697, #25163, #18361, #3376, #6026, #3176, #27631, #30949, #33836, #27829, #15479, #40381, #12187, #31145, #40590, #28241, #5616, #15690, #8889, #66 ),
 ( #18156, #24545, #40188, #21471, #24756, #9100, #21677, #2963, #22892, #22500, #35063, #22295, #19189, #7429, #35264, #28664, #34866, #16887, #19394, #25980, #32368, #31755, #13816, #4164, #13009 ),
 ( #35659, #470, #13208, #19601, #7234, #25776, #29066, #16097, #3769, #23094, #35462, #1280, #13406, #10514, #26385, #29468, #873, #38513, #10315, #19795, #13612, #16492, #22698, #16681, #25572 ),
 ( #29268, #19987, #26185, #38116, #38916, #1080, #38718, #3568, #6837, #32571, #28864, #31967, #4367, #6642, #9919, #16294, #671, #38313, #10110, #7032, #32174, #3973, #20186, #7834, #27173 ),
 ( #26782, #5361, #23287, #35856, #32771, #26577, #1884, #36446, #39320, #14601, #5156, #24080, #1473, #30072, #2286, #36649, #23489, #17899, #17086, #32963, #7635, #8221, #30273, #2089, #4560 ),
 ( #20384, #11110, #33584, #30480, #8428, #23870, #36056, #23681, #29660, #21006, #36247, #14006, #4750, #39117, #14810, #10913, #26978, #17284, #29863, #17693, #10708, #1677, #20792, #14208, #8024 ),
 ( #33166, #20580, #4953, #17480, #14409, #39730, #27378, #11305, #39523, #33387, #11513, #36852, #34407, #21212, #37452, #40336, #27782, #8836, #21624, #18937, #15428, #3326, #15844, #30693, #39941 ),
 ( #11714, #2500, #12547, #22035, #3125, #24290, #25118, #11920, #40535, #34204, #5972, #8635, #37648, #33784, #18513, #5561, #40139, #15024, #2708, #12343, #9452, #24495, #18102, #31098, #27587 ),
 ( #24916, #33994, #2908, #37050, #6179, #21420, #5769, #15641, #18308, #21826, #31503, #34612, #15228, #27988, #6389, #12128, #37255, #9249, #30898, #24707, #18721, #9046, #31303, #28189, #16 ),
 ( #9664, #25327, #37860, #16443, #1027, #28613, #32320, #6986, #19552, #31705, #32516, #7380, #29019, #13164, #29217, #38069, #4119, #28818, #19938, #7184, #16632, #420, #13561, #22648, #9871 ),
 ( #23045, #3928, #32128, #22250, #12959, #823, #35014, #25524, #13354, #35610, #25928, #26134, #38666, #19745, #22446, #10465, #621, #38461, #34816, #6788, #4315, #19342, #25725, #6594, #28402 ),
 ( #209, #12750, #35214, #19139, #31912, #3521, #3723, #10264, #16044, #16247, #38267, #22844, #10062, #35417, #27669, #12006, #8720, #33875, #40224, #5654, #18192, #21299, #30784, #2588, #15110 ),
 ( #22819, #35584, #29584, #7158, #998, #19913, #28788, #32688, #13534, #10239, #4487, #13135, #38433, #7355, #4283, #35388, #29390, #595, #13321, #7553, #1209, #26502, #13743, #17009, #10832 ),
 ( #32294, #1400, #16417, #23212, #19720, #39033, #26307, #13931, #6959, #23408, #38840, #25898, #10635, #19313, #31885, #25693, #3696, #10036, #22618, #35186, #19518, #32098, #3902, #27098, #30401 ),
 ( #27297, #7952, #5483, #36369, #5278, #4675, #33082, #11634, #20500, #17609, #29984, #14325, #20709, #30186, #2206, #21137, #36567, #39237, #14527, #14125, #32888, #14727, #17210, #33507, #8140 ),
 ( #30615, #1595, #17401, #29777, #20923, #39863, #24211, #26703, #8347, #40061, #11026, #8556, #18026, #36772, #7755, #20302, #23606, #36171, #39648, #17818, #23795, #33703, #2424, #14944, #4867 ),
 ( #33295, #5078, #1800, #2007, #27510, #11432, #11842, #35975, #26894, #39437, #11228, #23996, #34128, #12263, #6518, #19065, #37779, #37578, #8962, #24835, #33912, #9587, #37383, #30821, #5897 ),
 ( #2627, #24623, #27706, #27909, #25046, #22169, #37176, #341, #18638, #8757, #9176, #18855, #34740, #31629, #18232, #9374, #21551, #18435, #24420, #21340, #3455, #21748, #15146, #36976, #15969 ),
 ( #34331, #6101, #21959, #5691, #28533, #31224, #40452, #40260, #12044, #15353, #3043, #34533, #15563, #28119, #31023, #2831, #25249, #6306, #40671, #12475, #12673, #31428, #3252, #15771, #28327 ),
 ( #143, #29342, #13281, #4443, #32440, #1164, #13087, #26264, #7113, #22572, #13486, #16372, #29145, #31835, #29543, #35734, #20070, #6914, #23166, #12882, #25447, #4049, #7311, #13695, #3854 ),
 ( #32646, #35343, #19676, #28943, #37992, #16762, #10591, #747, #7507, #9794, #26061, #16970, #16172, #38796, #22374, #34940, #6718, #19269, #25647, #38593, #16563, #951, #3648, #28740, #551 ),
 ( #38191, #10399, #9993, #32047, #19869, #35141, #19472, #22975, #25854, #38387, #4237, #35539, #10192, #22776, #26659, #36528, #10986, #17979, #17772, #20460, #23951, #33662, #39822, #17359, #33248 ),
 ( #11386, #10786, #5439, #8301, #32846, #29734, #1967, #27253, #14485, #1359, #27058, #23364, #38987, #35932, #30149, #14685, #1548, #5235, #20664, #5033, #4635, #13894, #21091, #39604, #26854 ),
 ( #30359, #1754, #26457, #20877, #2164, #14080, #11590, #36327, #23566, #33467, #4829, #17563, #20260, #7711, #24170, #8511, #36130, #36727, #17165, #39193, #7911, #33039, #29937, #14284, #39395 ) ),
 .UNSPECIFIED., .F., .F., .F.,
 ( 4, 3, 3, 3, 3, 3, 3, 3, 3, 3, 3, 3, 3, 3, 3, 3, 3, 3, 3, 3, 3, 3, 3, 3, 3, 3, 3, 4 ),
 ( 4, 3, 3, 3, 3, 3, 3, 3, 4 ),
 ( -2.505502282154539045E-17, 9.220626685347035532E-07, 1.844125337094462129E-06, 3.688250674213979493E-06, 5.532376011333496433E-06, 7.376501348453014221E-06, 1.106475202269204810E-05, 1.475300269693108368E-05, 2.212950404540915483E-05, 2.950600539388722259E-05, 4.425900809084336150E-05, 5.901201078779949702E-05, 8.851801618171178162E-05, 0.0001180240215756240527, 0.0001770360323634486083, 0.0002360480431512731504, 0.0003540720647269222617, 0.0004720960863025713459, 0.0009441921726051677368, 0.001888384345210360627, 0.003776768690420746408, 0.005665153035631132622, 0.007553537380841517969, 0.01133030607126228953, 0.01321869041647267401, 0.01416288258907786798, 0.01463497867538046324, 0.01510707476168306022 ),
 ( 0.000000000000000000, 0.1250000000000000000, 0.2500000000000000000, 0.3750000000000000000, 0.5000000000000000000, 0.6250000000000000000, 0.7500000000000000000, 0.8750000000000000000, 1.000000000000000000 ),
 .UNSPECIFIED. ) ;
#3625 = CARTESIAN_POINT ( 'NONE',  ( 81.47505553675506462, 61.46950381087522430, 1.000000000000000000 ) ) ;
#3627 = ORIENTED_EDGE ( 'NONE', *, *, #26001, .T. ) ;
#3626 = CARTESIAN_POINT ( 'NONE',  ( -64.08758708074093136, 42.22117905423280604, 2.795515491199095148 ) ) ;
#3628 = CARTESIAN_POINT ( 'NONE',  ( 24.87384391889476021, -2.282154821806516409, -6.307558310060713325 ) ) ;
#3629 = EDGE_LOOP ( 'NONE', ( #35747, #24009, #39614, #18985 ) ) ;
#3630 = CARTESIAN_POINT ( 'NONE',  ( -77.28818573224673116, 9.645729766875481559, 9.280166210047219977 ) ) ;
#3631 = CARTESIAN_POINT ( 'NONE',  ( 23.05078809043722643, 0.3400200871709115336, -5.963306588542081066 ) ) ;
#3632 = CARTESIAN_POINT ( 'NONE',  ( -0.03896179826184579392, -32.60714627078814942, 7.756742906098588186 ) ) ;
#3633 = VECTOR ( 'NONE', #35875, 1000.000000000000000 ) ;
#3634 = AXIS2_PLACEMENT_3D ( 'NONE', #8388, #17438, #33545 ) ;
#3635 = CARTESIAN_POINT ( 'NONE',  ( -1.013064772776306688, -31.75849859061222347, 7.784725160561910329 ) ) ;
#3636 = CARTESIAN_POINT ( 'NONE',  ( 29.60526006017712319, -3.794915248219668857, -4.412248584793623252 ) ) ;
#3637 = CARTESIAN_POINT ( 'NONE',  ( 29.48812867847481556, 1.219306054872145273, -4.222749534284976569 ) ) ;
#3638 = CYLINDRICAL_SURFACE ( 'NONE', #18982, 6.329987104167475565 ) ;
#3639 = CARTESIAN_POINT ( 'NONE',  ( 15.98747256189193777, 10.21191258246141587, 2.701629770405024722 ) ) ;
#3640 = DIRECTION ( 'NONE',  ( -0.000000000000000000, -0.000000000000000000, -1.000000000000000000 ) ) ;
#3641 = CARTESIAN_POINT ( 'NONE',  ( -30.34874870218063947, -26.64985754041175525, 6.700000000000000178 ) ) ;
#3642 = CARTESIAN_POINT ( 'NONE',  ( -30.34874870218063947, -26.64985754041175525, 6.800000000000000711 ) ) ;
#3643 = CARTESIAN_POINT ( 'NONE',  ( 21.58862418887968460, 7.202556094215188054, 2.923978954502209682 ) ) ;
#3644 = CARTESIAN_POINT ( 'NONE',  ( 24.05048767930056641, 0.8437649274697022195, -5.043273178371332932 ) ) ;
#3645 = CARTESIAN_POINT ( 'NONE',  ( 36.43378600387098487, -1.733243984275257166, -5.730557465163646391 ) ) ;
#3646 = DIRECTION ( 'NONE',  ( -0.000000000000000000, -1.000000000000000000, -0.000000000000000000 ) ) ;
#3647 = ORIENTED_EDGE ( 'NONE', *, *, #7287, .F. ) ;
#3648 = CARTESIAN_POINT ( 'NONE',  ( 66.74404603967394678, 57.81040951471371159, 3.998354769210576976 ) ) ;
#3649 = CARTESIAN_POINT ( 'NONE',  ( -64.08758708074093136, 38.43534281692316767, 4.049547700704724029 ) ) ;
#3650 = CARTESIAN_POINT ( 'NONE',  ( 87.89980060869044109, -1.794189136469996004, 3.743635721206352684 ) ) ;
#3651 = ORIENTED_EDGE ( 'NONE', *, *, #40468, .T. ) ;
#3652 = CARTESIAN_POINT ( 'NONE',  ( 24.37736685700319939, 2.941625658114979558, 3.719599273349688762 ) ) ;
#3653 = CARTESIAN_POINT ( 'NONE',  ( 0.000000000000000000, 0.000000000000000000, -28.00000000000000000 ) ) ;
#3654 = EDGE_CURVE ( 'NONE', #13108, #18315, #10536, .T. ) ;
#3655 = CARTESIAN_POINT ( 'NONE',  ( 5.671973749040267521, -26.25500220387225170, 7.635761828346577573 ) ) ;
#3656 = FACE_OUTER_BOUND ( 'NONE', #39726, .T. ) ;
#3657 = VERTEX_POINT ( 'NONE', #26550 ) ;
#3658 = AXIS2_PLACEMENT_3D ( 'NONE', #36462, #5377, #8237 ) ;
#3659 = VECTOR ( 'NONE', #11289, 1000.000000000000000 ) ;
#3660 = EDGE_CURVE ( 'NONE', #2270, #27725, #32936, .T. ) ;
#3661 = ORIENTED_EDGE ( 'NONE', *, *, #24979, .F. ) ;
#3662 = CARTESIAN_POINT ( 'NONE',  ( 78.77165107407959965, 65.73683965358550552, -2.311104455577570160 ) ) ;
#3663 = AXIS2_PLACEMENT_3D ( 'NONE', #7452, #13230, #35679 ) ;
#3664 = CARTESIAN_POINT ( 'NONE',  ( -40.97867591359219119, -26.64985754041175525, 6.700000000000000178 ) ) ;
#3665 = CARTESIAN_POINT ( 'NONE',  ( 80.57935153413077956, 62.61414007970553541, 3.419027627190931451 ) ) ;
#3668 = ORIENTED_EDGE ( 'NONE', *, *, #57, .F. ) ;
#3667 = VERTEX_POINT ( 'NONE', #22671 ) ;
#3666 = DIRECTION ( 'NONE',  ( 0.000000000000000000, 0.000000000000000000, -1.000000000000000000 ) ) ;
#3669 = EDGE_CURVE ( 'NONE', #12826, #5793, #19960, .T. ) ;
#3670 = AXIS2_PLACEMENT_3D ( 'NONE', #28952, #13288, #38399 ) ;
#3672 = EDGE_CURVE ( 'NONE', #3169, #15928, #20158, .T. ) ;
#3671 = CARTESIAN_POINT ( 'NONE',  ( -56.90680744419238124, 30.56621156453423183, 3.329292219611507342 ) ) ;
#3673 = CARTESIAN_POINT ( 'NONE',  ( -23.07867591359219617, -24.55319635012989110, 6.700000000000000178 ) ) ;
#3674 = LINE ( 'NONE', #6934, #555 ) ;
#3675 = CARTESIAN_POINT ( 'NONE',  ( 33.88049027533028124, -5.353668869269942121, -1.604319996572373785 ) ) ;
#3676 = CARTESIAN_POINT ( 'NONE',  ( 24.38812970663561330, 3.155185924440667478, -3.309899503823893419 ) ) ;
#3677 = VERTEX_POINT ( 'NONE', #844 ) ;
#3678 = CARTESIAN_POINT ( 'NONE',  ( -1.757012188144002840, -30.11440263980361465, 6.870737987065013819 ) ) ;
#3679 = CARTESIAN_POINT ( 'NONE',  ( 4.285952550363297142, -27.36202013534370181, 7.661510568013097711 ) ) ;
#3680 = CARTESIAN_POINT ( 'NONE',  ( -81.80090188080515645, -5.603160304130403446, -0.6545554231109701471 ) ) ;
#3681 = PLANE ( 'NONE',  #7034 ) ;
#3682 = CARTESIAN_POINT ( 'NONE',  ( -61.24591834330252027, -49.47158280949359010, -2.500000000000000000 ) ) ;
#3683 = CARTESIAN_POINT ( 'NONE',  ( 79.39921707337094858, 65.76781561079134519, 2.628317182735757651 ) ) ;
#3684 = DIRECTION ( 'NONE',  ( -0.000000000000000000, 0.000000000000000000, 1.000000000000000000 ) ) ;
#3685 = CARTESIAN_POINT ( 'NONE',  ( 22.22910988738226834, 4.118587929658937163, -2.394959132921147038 ) ) ;
#3686 = CARTESIAN_POINT ( 'NONE',  ( -1.327607472881008110, -27.82106663299630611, 7.767720160662274331 ) ) ;
#3687 = CARTESIAN_POINT ( 'NONE',  ( 21.56937222159085010, 7.264334593773944526, -2.455214307437531662 ) ) ;
#3688 = CARTESIAN_POINT ( 'NONE',  ( 35.48433445138798703, -1.920574954861675065, 5.744586601647555746 ) ) ;
#3689 = ORIENTED_EDGE ( 'NONE', *, *, #36684, .F. ) ;
#3690 = AXIS2_PLACEMENT_3D ( 'NONE', #12089, #6350, #21792 ) ;
#3691 = AXIS2_PLACEMENT_3D ( 'NONE', #39772, #12383, #36683 ) ;
#3692 = CARTESIAN_POINT ( 'NONE',  ( -66.99872204295122913, 28.48507918597134037, -6.999999999999999112 ) ) ;
#3693 = FACE_OUTER_BOUND ( 'NONE', #16574, .T. ) ;
#3694 = CARTESIAN_POINT ( 'NONE',  ( 4.630123336105056886, -27.84462688399876029, 7.730758795053809251 ) ) ;
#3695 = DIRECTION ( 'NONE',  ( 1.000000000000000000, 0.000000000000000000, -0.000000000000000000 ) ) ;
#3696 = CARTESIAN_POINT ( 'NONE',  ( 68.67947939959147163, 58.42312895491860303, 3.988324671431328738 ) ) ;
#3697 = CARTESIAN_POINT ( 'NONE',  ( 36.89747129275986026, -3.002612578834559898, 5.965140782587297075 ) ) ;
#3698 = CIRCLE ( 'NONE', #37186, 0.1000000000000028644 ) ;
#3699 = EDGE_CURVE ( 'NONE', #2951, #9053, #26343, .T. ) ;
#3700 = CARTESIAN_POINT ( 'NONE',  ( 85.17359253740836778, 2.686702876117401662, 1.784494502703901864 ) ) ;
#3701 = VERTEX_POINT ( 'NONE', #23459 ) ;
#3703 = CARTESIAN_POINT ( 'NONE',  ( 25.73532669649552318, 2.638944299754048206, 3.514017186027001305 ) ) ;
#3702 = CARTESIAN_POINT ( 'NONE',  ( 81.23333979799274118, 62.00977392264719157, -2.676159939830913270 ) ) ;
#3704 = CARTESIAN_POINT ( 'NONE',  ( -69.58021497804521971, -46.45211564195850684, 9.908779002578803841 ) ) ;
#3705 = EDGE_LOOP ( 'NONE', ( #21612, #33997, #7666, #28503 ) ) ;
#3706 = FACE_OUTER_BOUND ( 'NONE', #25613, .T. ) ;
#3707 = VERTEX_POINT ( 'NONE', #16652 ) ;
#3708 = CARTESIAN_POINT ( 'NONE',  ( -75.70508440899935465, -5.314284899882218305, 8.787320279435890669 ) ) ;
#3710 = ORIENTED_EDGE ( 'NONE', *, *, #34804, .F. ) ;
#3709 = VERTEX_POINT ( 'NONE', #7805 ) ;
#3711 = CARTESIAN_POINT ( 'NONE',  ( 81.08254763934547782, 61.27217476014467934, -1.284346554836955256 ) ) ;
#3712 = B_SPLINE_CURVE_WITH_KNOTS ( 'NONE', 3,
 ( #24367, #35582, #10632, #38639, #24162, #7352, #21087, #23208, #2159, #5643, #32482, #2371, #36930, #33658, #995, #14889, #1205, #30354, #10828, #35973, #14680, #36721, #40013, #8709, #19909 ),
 .UNSPECIFIED., .F., .F.,
 ( 4, 3, 3, 3, 3, 3, 3, 3, 4 ),
 ( 6.468151674593633721E-05, 9.076621574722126763E-05, 0.0001210204262067980478, 0.0001512763324577447036, 0.0001815301820994257400, 0.0002117781465860766417, 0.0002420274594459822007, 0.0002722905548971199627, 0.0002816827545175661063 ),
 .UNSPECIFIED. ) ;
#3713 = FACE_OUTER_BOUND ( 'NONE', #630, .T. ) ;
#3714 = CARTESIAN_POINT ( 'NONE',  ( 23.51831161216184185, 2.310449087985749106, 4.435690330918023783 ) ) ;
#3715 = VERTEX_POINT ( 'NONE', #20357 ) ;
#3716 = EDGE_CURVE ( 'NONE', #40022, #6547, #39412, .T. ) ;
#3717 = AXIS2_PLACEMENT_3D ( 'NONE', #39855, #20703, #7943 ) ;
#3719 = EDGE_CURVE ( 'NONE', #33808, #40124, #11473, .T. ) ;
#3718 = CARTESIAN_POINT ( 'NONE',  ( 4.723729895314598082, -28.01446086209832842, 6.876076431790004051 ) ) ;
#3721 = CARTESIAN_POINT ( 'NONE',  ( 86.35258271375249706, 1.362405151798338654, 4.807923594896911013 ) ) ;
#3720 = CARTESIAN_POINT ( 'NONE',  ( 4.574815660364650149, -31.38590853778189782, 6.865312560952602894 ) ) ;
#3722 = PLANE ( 'NONE',  #13917 ) ;
#3723 = CARTESIAN_POINT ( 'NONE',  ( 69.62738871241069205, 59.42086865771531023, 3.954846139149833739 ) ) ;
#3724 = CARTESIAN_POINT ( 'NONE',  ( 22.99674145141367987, 3.564721660139269055, -3.751998251592491229 ) ) ;
#3725 = ORIENTED_EDGE ( 'NONE', *, *, #22930, .T. ) ;
#3726 = CIRCLE ( 'NONE', #4358, 2.999999999999998668 ) ;
#3727 = ORIENTED_EDGE ( 'NONE', *, *, #12696, .F. ) ;
#3728 = CARTESIAN_POINT ( 'NONE',  ( 21.85643539959781023, -9.626920734992143736, 7.250399157909895642 ) ) ;
#3729 = CARTESIAN_POINT ( 'NONE',  ( 18.05491602129117013, 13.75800355182912682, 1.937621434239656715 ) ) ;
#3730 = CARTESIAN_POINT ( 'NONE',  ( -54.85217575791900657, 31.46625607997153296, -1.118209565749431533 ) ) ;
#3731 = CARTESIAN_POINT ( 'NONE',  ( 81.34095870999074407, 61.40448684960413317, 1.344573736155039390 ) ) ;
#3732 = CARTESIAN_POINT ( 'NONE',  ( 88.92600529607371129, -1.724176122391732680, 0.2146816905789898644 ) ) ;
#3733 = ORIENTED_EDGE ( 'NONE', *, *, #992, .T. ) ;
#3734 = FACE_OUTER_BOUND ( 'NONE', #27206, .T. ) ;
#3735 = CARTESIAN_POINT ( 'NONE',  ( 33.95122966076780102, -3.129518407428083737, 5.505308520791801996 ) ) ;
#3736 = CARTESIAN_POINT ( 'NONE',  ( 37.03092461603053209, -2.782178920321524807, 5.985969401264504164 ) ) ;
#3737 = CARTESIAN_POINT ( 'NONE',  ( 29.53482198975021333, -3.874005733230891035, 4.296914696760256724 ) ) ;
#3738 = CARTESIAN_POINT ( 'NONE',  ( 31.71901687615503462, -0.5584438621182004070, -5.156917729482751511 ) ) ;
#3739 = DIRECTION ( 'NONE',  ( 0.000000000000000000, 0.000000000000000000, 1.000000000000000000 ) ) ;
#3740 = DIRECTION ( 'NONE',  ( 1.000000000000000000, 0.000000000000000000, 0.000000000000000000 ) ) ;
#3741 = ORIENTED_EDGE ( 'NONE', *, *, #18894, .F. ) ;
#3742 = CARTESIAN_POINT ( 'NONE',  ( -22.24874870218063450, -26.64985754041175525, 6.700000000000000178 ) ) ;
#3743 = CARTESIAN_POINT ( 'NONE',  ( -32.24874870218063450, -25.49307895267003587, 6.700000000000000178 ) ) ;
#3744 = CARTESIAN_POINT ( 'NONE',  ( 32.00563084067037067, -3.049499025779075723, 5.201650770433705162 ) ) ;
#3745 = ORIENTED_EDGE ( 'NONE', *, *, #27944, .T. ) ;
#3746 = ORIENTED_EDGE ( 'NONE', *, *, #21021, .F. ) ;
#3747 = CARTESIAN_POINT ( 'NONE',  ( 36.87053919822349002, -2.087953330798700602, 5.864521777571895633 ) ) ;
#3748 =( BOUNDED_CURVE ( )  B_SPLINE_CURVE ( 3, ( #27503, #40054, #24411, #8747 ),
 .UNSPECIFIED., .F., .T. ) 
 B_SPLINE_CURVE_WITH_KNOTS ( ( 4, 4 ),
 ( 4.708531083176467291, 4.895802057644189631 ),
 .UNSPECIFIED. ) 
 CURVE ( )  GEOMETRIC_REPRESENTATION_ITEM ( )  RATIONAL_B_SPLINE_CURVE ( ( 1.000000000000000000, 0.9970795998553221295, 0.9970795998553221295, 1.000000000000000000 ) ) 
 REPRESENTATION_ITEM ( '' )  );
#3749 = FACE_OUTER_BOUND ( 'NONE', #22002, .T. ) ;
#3750 =( GEOMETRIC_REPRESENTATION_CONTEXT ( 3 ) GLOBAL_UNCERTAINTY_ASSIGNED_CONTEXT ( ( #25460 ) ) GLOBAL_UNIT_ASSIGNED_CONTEXT ( ( #39616, #24183, #17995 ) ) REPRESENTATION_CONTEXT ( 'NONE', 'WORKASPACE' ) );
#3751 = CARTESIAN_POINT ( 'NONE',  ( 66.58940539569050543, 57.77934511969053943, -3.999344142514784650 ) ) ;
#3752 = CARTESIAN_POINT ( 'NONE',  ( 86.88071486596068382, -1.182640904908754731, -5.180176386390026089 ) ) ;
#3753 = AXIS2_PLACEMENT_3D ( 'NONE', #2091, #24084, #14212 ) ;
#3754 = ORIENTED_EDGE ( 'NONE', *, *, #10665, .F. ) ;
#3755 = SHAPE_REPRESENTATION_RELATIONSHIP ( 'NONE' , 'NONE' ,  #131, #15661 ) ;
#3756 = ORIENTED_EDGE ( 'NONE', *, *, #15718, .T. ) ;
#3757 = FACE_BOUND ( 'NONE', #36746, .T. ) ;
#3758 = DIRECTION ( 'NONE',  ( 0.000000000000000000, -1.000000000000000000, 0.000000000000000000 ) ) ;
#3759 = EDGE_LOOP ( 'NONE', ( #4328, #25731, #16849, #10299, #17163, #15560, #868 ) ) ;
#3760 = CARTESIAN_POINT ( 'NONE',  ( 81.46661790917876544, 61.46529165999840671, -1.093381982072927361 ) ) ;
#3762 = EDGE_CURVE ( 'NONE', #27559, #34769, #8591, .T. ) ;
#3761 = CARTESIAN_POINT ( 'NONE',  ( -28.44874870218064444, -25.49307895267003587, 6.700000000000000178 ) ) ;
#3763 = EDGE_LOOP ( 'NONE', ( #7650, #7726, #6876, #28087 ) ) ;
#3764 = CARTESIAN_POINT ( 'NONE',  ( 75.18153624412200031, 63.60369824193131194, -2.950589020697163889 ) ) ;
#3766 = CARTESIAN_POINT ( 'NONE',  ( 0.000000000000000000, 0.000000000000000000, 0.000000000000000000 ) ) ;
#3765 = CARTESIAN_POINT ( 'NONE',  ( -1.697427395360086244, -29.44812577374269580, 7.754798119455333705 ) ) ;
#3767 = CARTESIAN_POINT ( 'NONE',  ( 15.64686839187730349, 11.13536136061385307, -2.614792074122313181 ) ) ;
#3768 = CARTESIAN_POINT ( 'NONE',  ( 79.48860182481722347, 65.82309781974730356, -2.578835243349315576 ) ) ;
#3769 = CARTESIAN_POINT ( 'NONE',  ( 76.28050337382492785, 62.76811984040510595, 3.753756190325763242 ) ) ;
#3770 = ADVANCED_FACE ( 'NONE', ( #29831 ), #33751, .F. ) ;
#3771 = VERTEX_POINT ( 'NONE', #37021 ) ;
#3772 = EDGE_LOOP ( 'NONE', ( #28412, #31133, #9049, #3622 ) ) ;
#3773 = CARTESIAN_POINT ( 'NONE',  ( 4.432911746439800460, -27.54673335294005199, 6.929923840112061306 ) ) ;
#3774 = AXIS2_PLACEMENT_3D ( 'NONE', #6293, #21327, #18218 ) ;
#3775 = DIRECTION ( 'NONE',  ( 0.4999999999999855116, 0.8660254037844470343, 0.000000000000000000 ) ) ;
#3776 = CARTESIAN_POINT ( 'NONE',  ( 0.5371228601270917613, -32.87096174259440318, 7.698786668945009737 ) ) ;
#3777 = CARTESIAN_POINT ( 'NONE',  ( 81.15665777833334005, 65.46403653819207591, 2.541832380858825235 ) ) ;
#3779 = CARTESIAN_POINT ( 'NONE',  ( 16.68329392019911595, 9.858079660169737579, 2.499999999999976463 ) ) ;
#3778 = CARTESIAN_POINT ( 'NONE',  ( -0.9575113486053227208, -31.84711263666175540, 7.686927408461905920 ) ) ;
#3780 = CARTESIAN_POINT ( 'NONE',  ( 27.77988552260176291, -0.3358138158918914651, -6.029166980063449088 ) ) ;
#3781 = VECTOR ( 'NONE', #38443, 1000.000000000000000 ) ;
#3782 = DIRECTION ( 'NONE',  ( 0.000000000000000000, 0.000000000000000000, -1.000000000000000000 ) ) ;
#3783 = DIRECTION ( 'NONE',  ( 0.9848077530122103518, -0.1736481776669172583, -0.000000000000000000 ) ) ;
#3784 = TOROIDAL_SURFACE ( 'NONE', #33365, 114.6618724293813898, 3.000000000000000000 ) ;
#3785 = CARTESIAN_POINT ( 'NONE',  ( 1.681055494462310618, -26.06998307431192075, 7.747520101777647383 ) ) ;
#3786 = CARTESIAN_POINT ( 'NONE',  ( 66.44405367406183416, 57.75571810119279093, 3.999999999999982681 ) ) ;
#3787 = CARTESIAN_POINT ( 'NONE',  ( 4.921324086407802056, -26.64985754041175525, 6.700000000000000178 ) ) ;
#3788 = CARTESIAN_POINT ( 'NONE',  ( 33.43833233143621442, -3.434996429908883098, -5.407889144347614696 ) ) ;
#3789 = CYLINDRICAL_SURFACE ( 'NONE', #31887, 0.9999999999999998890 ) ;
#3790 = CYLINDRICAL_SURFACE ( 'NONE', #39746, 0.09010775117052950700 ) ;
#3791 = CARTESIAN_POINT ( 'NONE',  ( 1.736248384610752149, -32.96974108739077991, 7.691066658568946224 ) ) ;
#3792 = CARTESIAN_POINT ( 'NONE',  ( 1.664466114274210318, -26.17011997221232278, 7.692469944509197965 ) ) ;
#3793 = ADVANCED_FACE ( 'NONE', ( #26947 ), #16442, .T. ) ;
#3794 = PLANE ( 'NONE',  #7689 ) ;
#3795 = LINE ( 'NONE', #19417, #35566 ) ;
#3796 = CARTESIAN_POINT ( 'NONE',  ( 30.44988808354906595, -2.941501225529987718, 4.958839487400774182 ) ) ;
#3797 = VERTEX_POINT ( 'NONE', #399 ) ;
#3798 = CARTESIAN_POINT ( 'NONE',  ( 2.625420455124711339, -26.29080307942845351, 7.505001789837626447 ) ) ;
#3799 = CARTESIAN_POINT ( 'NONE',  ( 67.80923286766689273, 58.07768331974902765, -3.990378031984521012 ) ) ;
#3800 = EDGE_CURVE ( 'NONE', #18519, #31377, #13143, .T. ) ;
#3801 = ORIENTED_EDGE ( 'NONE', *, *, #23984, .F. ) ;
#3802 = B_SPLINE_CURVE_WITH_KNOTS ( 'NONE', 3,
 ( #16565, #29345, #22575, #23168 ),
 .UNSPECIFIED., .F., .F.,
 ( 4, 4 ),
 ( 0.8210829304512126114, 0.9474561098508307300 ),
 .UNSPECIFIED. ) ;
#3803 = CARTESIAN_POINT ( 'NONE',  ( -0.9222807936984492860, -27.27089925875410259, 7.782861076432730840 ) ) ;
#3804 = CARTESIAN_POINT ( 'NONE',  ( -64.08758708074094557, 36.76569972833094369, 3.434863364315535961 ) ) ;
#3805 = CARTESIAN_POINT ( 'NONE',  ( 23.66522075457919172, 3.155031241165582312, 3.754767217157412684 ) ) ;
#3806 = AXIS2_PLACEMENT_3D ( 'NONE', #5241, #24179, #17989 ) ;
#3807 = CARTESIAN_POINT ( 'NONE',  ( 1.074608721727911664, -26.22801491291194864, 7.703977250142849620 ) ) ;
#3808 = VECTOR ( 'NONE', #39803, 1000.000000000000000 ) ;
#3809 = AXIS2_PLACEMENT_3D ( 'NONE', #18051, #21163, #14976 ) ;
#3810 = CARTESIAN_POINT ( 'NONE',  ( 4.404516770028684469, -31.79202354683301834, 7.695279973900954751 ) ) ;
#3811 = VERTEX_POINT ( 'NONE', #34793 ) ;
#3812 = CARTESIAN_POINT ( 'NONE',  ( 22.87842292266282129, 4.333480938141546446, 3.064138866945673723 ) ) ;
#3813 = DIRECTION ( 'NONE',  ( 0.000000000000000000, 0.000000000000000000, 1.000000000000000000 ) ) ;
#3814 = CARTESIAN_POINT ( 'NONE',  ( 79.12779906683435627, 65.83686883797783196, 2.419967184825693174 ) ) ;
#3815 = ORIENTED_EDGE ( 'NONE', *, *, #11270, .F. ) ;
#3817 = EDGE_CURVE ( 'NONE', #2799, #23657, #25223, .T. ) ;
#3816 = CARTESIAN_POINT ( 'NONE',  ( 1.700390093233090871, -29.56993018339339940, 6.800000000000000711 ) ) ;
#3818 = EDGE_CURVE ( 'NONE', #12484, #5958, #32288, .T. ) ;
#3819 = ORIENTED_EDGE ( 'NONE', *, *, #34391, .F. ) ;
#3820 = CARTESIAN_POINT ( 'NONE',  ( 77.95070745440513349, 65.53481705947537250, -1.908681007153592235 ) ) ;
#3822 = CARTESIAN_POINT ( 'NONE',  ( -1.708395779829353645, -28.77608428252948158, 6.976682809038451616 ) ) ;
#3821 = CARTESIAN_POINT ( 'NONE',  ( 21.73434502951461056, 0.2315104026643188539, 9.064982765253589037 ) ) ;
#3823 = CARTESIAN_POINT ( 'NONE',  ( 81.16506502659913735, 61.30232764367859488, -1.065084354002960865 ) ) ;
#3824 = CARTESIAN_POINT ( 'NONE',  ( 79.47890774847340367, 63.12292952392867562, 3.765547211956734586 ) ) ;
#3825 = ORIENTED_EDGE ( 'NONE', *, *, #28655, .F. ) ;
#3826 = CARTESIAN_POINT ( 'NONE',  ( 81.47505553675506462, 61.46950381087522430, 1.024355359505926266 ) ) ;
#3827 = CARTESIAN_POINT ( 'NONE',  ( -70.92837670882107659, -36.87473357531881391, 0.000000000000000000 ) ) ;
#3828 = CARTESIAN_POINT ( 'NONE',  ( -1.261910041069867372, -27.90116479715461750, 7.693875151218753317 ) ) ;
#3829 = CARTESIAN_POINT ( 'NONE',  ( 24.03893326528611141, 2.664202206450044130, -5.290213626918107259 ) ) ;
#3830 = DIRECTION ( 'NONE',  ( 0.000000000000000000, 0.000000000000000000, 1.000000000000000000 ) ) ;
#3831 = CARTESIAN_POINT ( 'NONE',  ( -74.86601972701976138, -2.929674985788335739, 9.238933323493853322 ) ) ;
#3832 = CARTESIAN_POINT ( 'NONE',  ( 24.74313279468194793, 0.5480144272095329727, -4.780879834594610855 ) ) ;
#3833 = VERTEX_POINT ( 'NONE', #9848 ) ;
#3834 = EDGE_CURVE ( 'NONE', #8999, #14282, #15873, .T. ) ;
#3835 = CARTESIAN_POINT ( 'NONE',  ( -20.87867591359218977, -24.55319635012989110, 6.800000000000000711 ) ) ;
#3836 = ORIENTED_EDGE ( 'NONE', *, *, #2506, .T. ) ;
#3837 = CIRCLE ( 'NONE', #2530, 7.999999999999992895 ) ;
#3838 = CARTESIAN_POINT ( 'NONE',  ( -0.9757923178187628555, -31.82346948261344366, 7.762796336881261361 ) ) ;
#3839 = CARTESIAN_POINT ( 'NONE',  ( 29.54642850493534567, -3.606211835941682153, -4.678983485493422023 ) ) ;
#3840 = CARTESIAN_POINT ( 'NONE',  ( 36.49326386636163733, -3.559160538920521866, -5.796799980422059129 ) ) ;
#3841 = CARTESIAN_POINT ( 'NONE',  ( 3.417450607696787657, -32.61980722748252504, 6.887161170156907097 ) ) ;
#3842 = CARTESIAN_POINT ( 'NONE',  ( 16.61276722214797275, 9.469120112283594182, 2.799222124946485035 ) ) ;
#3843 = FACE_OUTER_BOUND ( 'NONE', #13102, .T. ) ;
#3844 = CARTESIAN_POINT ( 'NONE',  ( -0.5612858708501290428, -26.89882064179876409, 7.638132480492516585 ) ) ;
#3845 = ORIENTED_EDGE ( 'NONE', *, *, #21407, .F. ) ;
#3846 = LINE ( 'NONE', #35131, #7227 ) ;
#3847 = AXIS2_PLACEMENT_3D ( 'NONE', #1253, #1447, #39291 ) ;
#3848 = FACE_OUTER_BOUND ( 'NONE', #8797, .T. ) ;
#3849 = CARTESIAN_POINT ( 'NONE',  ( 24.78824275346884676, 1.421632137423702424, -4.544576515312537701 ) ) ;
#3850 = CARTESIAN_POINT ( 'NONE',  ( 33.59320765816826082, -0.3498627648884612418, -5.050355079047641915 ) ) ;
#3851 = FACE_OUTER_BOUND ( 'NONE', #25626, .T. ) ;
#3852 = ORIENTED_EDGE ( 'NONE', *, *, #19159, .T. ) ;
#3853 = EDGE_CURVE ( 'NONE', #13150, #26564, #32591, .T. ) ;
#3855 = EDGE_CURVE ( 'NONE', #25870, #36487, #23079, .T. ) ;
#3854 = CARTESIAN_POINT ( 'NONE',  ( 66.90849722842033032, 57.81418058710544727, 3.996206253853811674 ) ) ;
#3856 = EDGE_CURVE ( 'NONE', #35794, #14683, #12318, .T. ) ;
#3857 = CARTESIAN_POINT ( 'NONE',  ( 87.67674921920735187, -0.7466428619051976856, -5.210926517169286676 ) ) ;
#3858 = CARTESIAN_POINT ( 'NONE',  ( -1.078675913592196167, -26.64985754041175525, 6.700000000000000178 ) ) ;
#3859 = ORIENTED_EDGE ( 'NONE', *, *, #10125, .F. ) ;
#3860 = CARTESIAN_POINT ( 'NONE',  ( -72.89123299691203783, 3.290588968460324448, -10.95732599500614945 ) ) ;
#3861 = CARTESIAN_POINT ( 'NONE',  ( 0.000000000000000000, 0.000000000000000000, 0.000000000000000000 ) ) ;
#3862 = CARTESIAN_POINT ( 'NONE',  ( 2.241180031393448235, -32.92666184063634205, 7.785868773668302545 ) ) ;
#3863 = CARTESIAN_POINT ( 'NONE',  ( -12.44874870218064267, -25.49307895267003587, 6.700000000000000178 ) ) ;
#3864 = ORIENTED_EDGE ( 'NONE', *, *, #36921, .F. ) ;
#3865 = DIRECTION ( 'NONE',  ( -0.000000000000000000, -0.000000000000000000, 1.000000000000000000 ) ) ;
#3866 = VERTEX_POINT ( 'NONE', #40508 ) ;
#3867 = VERTEX_POINT ( 'NONE', #38047 ) ;
#3868 = CARTESIAN_POINT ( 'NONE',  ( 80.72570547868197366, 61.86964107431867177, -2.884918531047269141 ) ) ;
#3869 = CARTESIAN_POINT ( 'NONE',  ( -1.722734353762952475, -28.91418899491404915, 7.785344483711591934 ) ) ;
#3870 = CARTESIAN_POINT ( 'NONE',  ( 79.10075812992909050, 65.22691190166821684, 3.061371641637242735 ) ) ;
#3873 = EDGE_LOOP ( 'NONE', ( #30242, #17507, #25147, #10970, #33925, #12535, #40320 ) ) ;
#3872 = EDGE_LOOP ( 'NONE', ( #3689, #3486, #29987, #31844 ) ) ;
#3871 = CARTESIAN_POINT ( 'NONE',  ( -1.280268548403576290, -31.20570797914146155, 6.874555630061442990 ) ) ;
#3874 = AXIS2_PLACEMENT_3D ( 'NONE', #7544, #7343, #4273 ) ;
#3875 = CARTESIAN_POINT ( 'NONE',  ( -22.44874870218064089, -26.64985754041175525, 6.700000000000000178 ) ) ;
#3876 = CARTESIAN_POINT ( 'NONE',  ( 1.062037487868057184, -33.01122440958558002, 6.894806418505347700 ) ) ;
#3877 = CARTESIAN_POINT ( 'NONE',  ( -1.786480958475062719, -29.49459066941995644, 7.782861076432731728 ) ) ;
#3878 = CARTESIAN_POINT ( 'NONE',  ( 21.85643539959774628, 7.825395393543534972, -11.66269361450695108 ) ) ;
#3879 = CARTESIAN_POINT ( 'NONE',  ( 24.36623814963473222, 3.146137341929644560, -3.353173740419891580 ) ) ;
#3880 = CARTESIAN_POINT ( 'NONE',  ( 5.200206962362909913, -29.53412679592301870, 7.700536657684215136 ) ) ;
#3881 = ORIENTED_EDGE ( 'NONE', *, *, #35632, .F. ) ;
#3882 = EDGE_CURVE ( 'NONE', #12496, #7875, #17142, .T. ) ;
#3883 = CARTESIAN_POINT ( 'NONE',  ( -0.9720661970843325062, -31.83001367219261013, 7.635761828346575797 ) ) ;
#3884 = DIRECTION ( 'NONE',  ( 0.000000000000000000, -1.000000000000000000, 0.000000000000000000 ) ) ;
#3885 = CARTESIAN_POINT ( 'NONE',  ( -75.07486328459704339, -3.143736151799179979, -10.45530216219834330 ) ) ;
#3886 = CIRCLE ( 'NONE', #9103, 8.204531065793066347 ) ;
#3887 = CYLINDRICAL_SURFACE ( 'NONE', #39222, 3.399999999999999911 ) ;
#3888 = DIRECTION ( 'NONE',  ( 0.000000000000000000, 0.000000000000000000, 1.000000000000000000 ) ) ;
#3889 = CARTESIAN_POINT ( 'NONE',  ( 79.24523542244190821, 65.91691524828226534, 2.349509806045092297 ) ) ;
#3890 = CARTESIAN_POINT ( 'NONE',  ( 85.38915795161820199, 1.318023545160245558, -5.584599991349963766 ) ) ;
#3891 = CARTESIAN_POINT ( 'NONE',  ( -0.5744564167362967710, -26.91002633704227875, 7.720710062488898906 ) ) ;
#3892 = CARTESIAN_POINT ( 'NONE',  ( -1.292017994372690159, -27.78295751345079623, 7.785344483711591934 ) ) ;
#3893 = CARTESIAN_POINT ( 'NONE',  ( 21.53507218971822468, 7.396261084522392615, 0.9507677088441091051 ) ) ;
#3894 = CARTESIAN_POINT ( 'NONE',  ( 33.55284483517386462, -1.200833309292756779, 5.443130933784450676 ) ) ;
#3895 = EDGE_CURVE ( 'NONE', #22787, #9079, #34183, .T. ) ;
#3896 = EDGE_LOOP ( 'NONE', ( #15633, #1632, #6291, #8277 ) ) ;
#3897 = CYLINDRICAL_SURFACE ( 'NONE', #13830, 2.500000000000002220 ) ;
#3898 = EDGE_CURVE ( 'NONE', #16025, #29790, #6157, .T. ) ;
#3899 = CARTESIAN_POINT ( 'NONE',  ( -0.3376550272357887184, -26.84845906633096746, 6.895222827070021765 ) ) ;
#3900 = CARTESIAN_POINT ( 'NONE',  ( 4.669725009344072753, -27.91368402659282921, 7.785868773668303433 ) ) ;
#3901 = CARTESIAN_POINT ( 'NONE',  ( 11.65737507970504439, -27.06993018339339940, 6.800000000000000711 ) ) ;
#3902 = CARTESIAN_POINT ( 'NONE',  ( 68.77554901931263487, 58.16923054873410592, 3.957896739784568574 ) ) ;
#3903 = CARTESIAN_POINT ( 'NONE',  ( 36.44751297234375187, -2.353303903281885656, 5.894913904403375149 ) ) ;
#3904 = B_SPLINE_CURVE_WITH_KNOTS ( 'NONE', 3,
 ( #7597, #20149, #32729, #4525, #17046, #1438, #10873, #29819, #13971, #26539 ),
 .UNSPECIFIED., .F., .F.,
 ( 4, 3, 3, 4 ),
 ( 1.022834283856302764E-18, 3.025570593003180098E-05, 6.051145698344018127E-05, 6.468151674593884443E-05 ),
 .UNSPECIFIED. ) ;
#3905 = EDGE_CURVE ( 'NONE', #21757, #36812, #21108, .T. ) ;
#3906 = VECTOR ( 'NONE', #10189, 1000.000000000000000 ) ;
#3907 = CARTESIAN_POINT ( 'NONE',  ( 1.109803157764845061, -33.01974279738480789, 7.750000000000000888 ) ) ;
#3908 = CARTESIAN_POINT ( 'NONE',  ( 88.52897200822518187, -1.082218601420786186, 0.1993289098281435523 ) ) ;
#3909 = ORIENTED_EDGE ( 'NONE', *, *, #9581, .F. ) ;
#3911 = CARTESIAN_POINT ( 'NONE',  ( -0.3996106877581342420, -26.76992922016355436, 6.971170733404096431 ) ) ;
#3910 = CARTESIAN_POINT ( 'NONE',  ( 81.26572199898306792, 62.02204868734987286, -2.661900242191199695 ) ) ;
#3912 = CARTESIAN_POINT ( 'NONE',  ( -1.543298022821887328, -28.25521066738867049, 7.750000000000000888 ) ) ;
#3913 = ORIENTED_EDGE ( 'NONE', *, *, #7068, .F. ) ;
#3914 = FACE_OUTER_BOUND ( 'NONE', #16342, .T. ) ;
#3915 = ORIENTED_EDGE ( 'NONE', *, *, #8014, .T. ) ;
#3916 = CARTESIAN_POINT ( 'NONE',  ( -1.722317759908783996, -28.83844474126830804, 7.750000000000000888 ) ) ;
#3917 = ORIENTED_EDGE ( 'NONE', *, *, #33230, .T. ) ;
#3918 = CIRCLE ( 'NONE', #19672, 6.681288188914807691 ) ;
#3919 = CARTESIAN_POINT ( 'NONE',  ( 81.12024331894986062, 61.43208913379081793, -1.925402693829568745 ) ) ;
#3920 = PLANE ( 'NONE',  #23999 ) ;
#3921 = CARTESIAN_POINT ( 'NONE',  ( 24.50089963235556567, 1.790356837895823006, 4.437133755813296609 ) ) ;
#3923 = EDGE_LOOP ( 'NONE', ( #27975, #36477, #33008, #33198, #7175 ) ) ;
#3922 = ORIENTED_EDGE ( 'NONE', *, *, #30549, .T. ) ;
#3924 = CARTESIAN_POINT ( 'NONE',  ( -0.002090259858060845594, -32.51298313013740682, 7.769368695748488207 ) ) ;
#3926 = CARTESIAN_POINT ( 'NONE',  ( 85.23804977158383167, 2.614301451366713991, 1.665401937347900763 ) ) ;
#3925 = CARTESIAN_POINT ( 'NONE',  ( -58.71358459458718926, 29.03749951736172719, -5.614777500241355135 ) ) ;
#3927 = DIRECTION ( 'NONE',  ( -0.000000000000000000, 1.000000000000000000, -0.000000000000000000 ) ) ;
#3928 = CARTESIAN_POINT ( 'NONE',  ( 70.57032280423491954, 60.39816359117256184, 3.808711916423200616 ) ) ;
#3929 = CARTESIAN_POINT ( 'NONE',  ( 23.64958599753803981, 3.252002366305553060, -3.672120356605920399 ) ) ;
#3930 = ORIENTED_EDGE ( 'NONE', *, *, #18262, .T. ) ;
#3931 = ORIENTED_EDGE ( 'NONE', *, *, #36941, .F. ) ;
#3932 = AXIS2_PLACEMENT_3D ( 'NONE', #8235, #11127, #36264 ) ;
#3933 = CARTESIAN_POINT ( 'NONE',  ( 21.85643539959775694, 2.022457263371903569, 13.81434276849105558 ) ) ;
#3934 = CARTESIAN_POINT ( 'NONE',  ( 21.77466435200733841, 5.668278662190309625, 2.100676170755116701 ) ) ;
#3935 = ORIENTED_EDGE ( 'NONE', *, *, #20944, .T. ) ;
#3936 = DIRECTION ( 'NONE',  ( 1.000000000000000000, 0.000000000000000000, 0.000000000000000000 ) ) ;
#3937 = CARTESIAN_POINT ( 'NONE',  ( 80.42837321982344179, 65.43835520822057106, 2.971291902561977949 ) ) ;
#3938 = CARTESIAN_POINT ( 'NONE',  ( 86.79297523138272652, 0.7501027249346864378, -5.742269118526623473 ) ) ;
#3939 = ORIENTED_EDGE ( 'NONE', *, *, #766, .F. ) ;
#3940 = CARTESIAN_POINT ( 'NONE',  ( 14.64292194440910500, -5.617547757890807958, 2.491780128467261601 ) ) ;
#3941 = CARTESIAN_POINT ( 'NONE',  ( 5.076275776509211468, -29.16566689353966169, 6.895222827070021765 ) ) ;
#3942 = CARTESIAN_POINT ( 'NONE',  ( 37.04602089111122609, -2.800936193217299586, -5.988325540095575938 ) ) ;
#3943 = CARTESIAN_POINT ( 'NONE',  ( 5.011198270955363299, -30.34358980514384285, 7.013842709614101167 ) ) ;
#3944 = CARTESIAN_POINT ( 'NONE',  ( -1.765891609886502511, -30.05458793497804137, 7.751599049952173637 ) ) ;
#3945 = ORIENTED_EDGE ( 'NONE', *, *, #17399, .F. ) ;
#3946 = DIRECTION ( 'NONE',  ( 1.000000000000000000, 0.000000000000000000, 0.000000000000000000 ) ) ;
#3947 = EDGE_CURVE ( 'NONE', #2740, #7424, #22013, .T. ) ;
#3948 = EDGE_CURVE ( 'NONE', #6853, #33723, #19780, .T. ) ;
#3949 = CARTESIAN_POINT ( 'NONE',  ( 5.551251297819359110, -26.64985754041175525, 6.700000000000000178 ) ) ;
#3950 = EDGE_CURVE ( 'NONE', #34664, #4150, #32091, .T. ) ;
#3951 = CARTESIAN_POINT ( 'NONE',  ( 28.84716823796745189, -3.982103006514774002, 4.149921582050339453 ) ) ;
#3952 = ORIENTED_EDGE ( 'NONE', *, *, #38992, .F. ) ;
#3953 = ORIENTED_EDGE ( 'NONE', *, *, #14972, .T. ) ;
#3954 = CARTESIAN_POINT ( 'NONE',  ( 37.10426046727946670, -3.126190214317604799, 5.976248370712866631 ) ) ;
#3955 = CARTESIAN_POINT ( 'NONE',  ( 66.41703863280939402, 57.80493748213750393, -4.000000000000021316 ) ) ;
#3956 = CARTESIAN_POINT ( 'NONE',  ( 87.50351120902806201, -1.998158110427775247, 3.528025977964829085 ) ) ;
#3957 = VECTOR ( 'NONE', #1568, 1000.000000000000000 ) ;
#3958 = ORIENTED_EDGE ( 'NONE', *, *, #11545, .T. ) ;
#3959 = B_SPLINE_CURVE_WITH_KNOTS ( 'NONE', 3,
 ( #34198, #37249, #8629, #33779, #5557, #2496, #33990, #24286 ),
 .UNSPECIFIED., .F., .F.,
 ( 4, 2, 2, 4 ),
 ( 0.000000000000000000, 0.1250305178534004968, 0.2500610357068009937, 0.5001220714135948819 ),
 .UNSPECIFIED. ) ;
#3960 = CARTESIAN_POINT ( 'NONE',  ( 4.954463893073100422, -28.58453498085037836, 7.013842709614101167 ) ) ;
#3961 = CARTESIAN_POINT ( 'NONE',  ( 2.272716057154847924, -26.11704110451741556, 7.695279973900954751 ) ) ;
#3962 = FACE_BOUND ( 'NONE', #16065, .T. ) ;
#3963 = CARTESIAN_POINT ( 'NONE',  ( -71.92837670882106238, -42.87473357531881391, -1.732050807568860318 ) ) ;
#3964 = ORIENTED_EDGE ( 'NONE', *, *, #3660, .F. ) ;
#3965 = CARTESIAN_POINT ( 'NONE',  ( 22.22653128512649090, 5.106210340169274886, 3.172958745359750310 ) ) ;
#3966 = CARTESIAN_POINT ( 'NONE',  ( 81.41819469040422064, 65.60226997055944764, -2.078018481493678404 ) ) ;
#3967 = VECTOR ( 'NONE', #18154, 1000.000000000000000 ) ;
#3968 = EDGE_LOOP ( 'NONE', ( #12840, #27144, #6953, #34302 ) ) ;
#3969 = CARTESIAN_POINT ( 'NONE',  ( 75.80265905884337485, 60.84868533121094458, -3.810661578667723148 ) ) ;
#3971 = CARTESIAN_POINT ( 'NONE',  ( -40.97867591359219119, -24.55319635012989110, 6.700000000000000178 ) ) ;
#3970 = LINE ( 'NONE', #16489, #35145 ) ;
#3972 = CARTESIAN_POINT ( 'NONE',  ( -70.12941285977503014, -0.1676659666690925865, 5.947291465561957757 ) ) ;
#3973 = CARTESIAN_POINT ( 'NONE',  ( 76.74823446354523071, 60.29158698200765798, 3.346357594037719707 ) ) ;
#3974 = DIRECTION ( 'NONE',  ( 0.000000000000000000, 0.000000000000000000, 1.000000000000000000 ) ) ;
#3975 = CARTESIAN_POINT ( 'NONE',  ( 4.588767459758324848E-15, -39.37473357531881391, 6.000000000000000000 ) ) ;
#3976 = DIRECTION ( 'NONE',  ( -0.000000000000000000, -0.000000000000000000, -1.000000000000000000 ) ) ;
#3977 = CARTESIAN_POINT ( 'NONE',  ( 81.77194423968626324, 61.86568514665832907, 1.662695954554601840 ) ) ;
#3978 = CARTESIAN_POINT ( 'NONE',  ( 86.31823139319517679, 1.400990185460310844, -4.784756222713710372 ) ) ;
#3979 = CARTESIAN_POINT ( 'NONE',  ( 27.52542935251784328, 0.09321990139520379415, -5.913109915068038624 ) ) ;
#3980 = CARTESIAN_POINT ( 'NONE',  ( 2.255350295996689347, -26.21552723005750352, 7.703977250142848732 ) ) ;
#3981 = CARTESIAN_POINT ( 'NONE',  ( -69.92837670882109080, -20.91525569503158977, 9.949874371066208312 ) ) ;
#3982 = AXIS2_PLACEMENT_3D ( 'NONE', #28937, #9787, #6910 ) ;
#3983 = CARTESIAN_POINT ( 'NONE',  ( 2.338742698598151204, -26.12863595720122234, 6.894806418505347700 ) ) ;
#3984 = EDGE_LOOP ( 'NONE', ( #38476, #2259, #7737, #10448, #31005, #957 ) ) ;
#3985 = CARTESIAN_POINT ( 'NONE',  ( 0.7364113883766857382, -26.30944669709577610, 6.939395833800442226 ) ) ;
#3986 = CARTESIAN_POINT ( 'NONE',  ( 66.27376694608931018, 57.73522568913554665, 4.000000000000000000 ) ) ;
#3987 = CARTESIAN_POINT ( 'NONE',  ( 25.58354041903514187, 2.439056306859946233, -4.005116038328519146 ) ) ;
#3988 = CARTESIAN_POINT ( 'NONE',  ( 1.144161204942605092, -32.92412392164827395, 7.712764235869103757 ) ) ;
#3989 = CARTESIAN_POINT ( 'NONE',  ( -1.797340250851707344, -29.44390463015740522, 7.750000000000000888 ) ) ;
#3990 =( BOUNDED_SURFACE ( )  B_SPLINE_SURFACE ( 3, 2, ( 
 ( #32094, #788, #9838 ),
 ( #29385, #38035, #22814 ),
 ( #29184, #12926, #10233 ),
 ( #34983, #7350, #7154 ) ),
 .UNSPECIFIED., .F., .F., .T. ) 
 B_SPLINE_SURFACE_WITH_KNOTS ( ( 4, 4 ),
 ( 3, 3 ),
 ( 0.000000000000000000, 0.0006385966863609145649 ),
 ( 0.000000000000000000, 1.000000000000000000 ),
 .UNSPECIFIED. ) 
 GEOMETRIC_REPRESENTATION_ITEM ( )  RATIONAL_B_SPLINE_SURFACE ( (
 ( 1.000000000000000000, 0.5935057080259643625, 1.000000000000000000),
 ( 1.000000000000000000, 0.5840949208454031538, 1.000000000000000000),
 ( 1.000000000000000000, 0.5746205253747198594, 1.000000000000000000),
 ( 1.000000000000000000, 0.5652620711642702966, 1.000000000000000000) ) ) 
 REPRESENTATION_ITEM ( '' )  SURFACE ( )  );
#3991 = PRODUCT_DEFINITION_SHAPE ( 'NONE', 'NONE',  #40731 ) ;
#3992 = CARTESIAN_POINT ( 'NONE',  ( 3.397908533250484364, -32.51584789198624037, 7.769368695748488207 ) ) ;
#3993 = CARTESIAN_POINT ( 'NONE',  ( -1.580282519025539401, -28.36646263432153248, 7.773839561854630986 ) ) ;
#3994 = DIRECTION ( 'NONE',  ( -0.2817767355331954882, 0.9594800004753907263, 0.000000000000000000 ) ) ;
#3995 = DIRECTION ( 'NONE',  ( -0.000000000000000000, -1.000000000000000000, -0.000000000000000000 ) ) ;
#3996 = VECTOR ( 'NONE', #20602, 999.9999999999998863 ) ;
#3997 = EDGE_CURVE ( 'NONE', #4296, #17900, #13329, .T. ) ;
#3998 = CARTESIAN_POINT ( 'NONE',  ( 33.46455515056310759, -3.089188617792877789, 5.429351193206847448 ) ) ;
#3999 = ORIENTED_EDGE ( 'NONE', *, *, #21548, .F. ) ;
#4000 = CARTESIAN_POINT ( 'NONE',  ( -6.248748702180631831, -26.64985754041175525, 6.800000000000000711 ) ) ;
#4001 = CARTESIAN_POINT ( 'NONE',  ( 68.12732179974642577, 58.11841597887141120, -3.982418445723222789 ) ) ;
#4002 = LINE ( 'NONE', #16520, #6221 ) ;
#4003 = ORIENTED_EDGE ( 'NONE', *, *, #28033, .T. ) ;
#4004 = CARTESIAN_POINT ( 'NONE',  ( 1.700390093233090871, -29.56993018339339940, 7.750000000000000888 ) ) ;
#4005 = CARTESIAN_POINT ( 'NONE',  ( 30.48050265367797707, -3.144661348558943192, 4.957493858021535971 ) ) ;
#4006 = CARTESIAN_POINT ( 'NONE',  ( 22.01915847652775327, 4.164052895855497205, 4.067381656372952570 ) ) ;
#4007 = CARTESIAN_POINT ( 'NONE',  ( 5.121324086407808451, -24.55319635012989110, 6.700000000000000178 ) ) ;
#4008 = APPLICATION_CONTEXT ( 'automotive_design' ) ;
#4009 = CARTESIAN_POINT ( 'NONE',  ( 1.228243814321680949, -26.20287178139112072, 7.757178535559533294 ) ) ;
#4010 = CARTESIAN_POINT ( 'NONE',  ( 4.390205000165592786, -31.80932647847912875, 7.635761828346570468 ) ) ;
#4011 = VERTEX_POINT ( 'NONE', #4097 ) ;
#4012 = VECTOR ( 'NONE', #16704, 1000.000000000000227 ) ;
#4013 = LINE ( 'NONE', #26621, #39888 ) ;
#4014 = CARTESIAN_POINT ( 'NONE',  ( 81.08176929032271119, 62.48897713179231772, 3.134554000843276178 ) ) ;
#4015 = DIRECTION ( 'NONE',  ( -1.000000000000000000, 0.000000000000000000, 0.000000000000000000 ) ) ;
#4016 = ORIENTED_EDGE ( 'NONE', *, *, #9483, .T. ) ;
#4017 = CARTESIAN_POINT ( 'NONE',  ( 78.78025785238997969, 63.39248666165328672, -3.791687334209850935 ) ) ;
#4019 = CARTESIAN_POINT ( 'NONE',  ( -0.7969451277773216269, -31.88752197801528965, 7.139196562012274150 ) ) ;
#4018 = CARTESIAN_POINT ( 'NONE',  ( 22.62923931292150570, 0.3004384395878155201, 6.475933053414085983 ) ) ;
#4020 = CARTESIAN_POINT ( 'NONE',  ( 79.73441168749667440, 65.96538777704688528, -2.410848004503907127 ) ) ;
#4021 = EDGE_CURVE ( 'NONE', #14780, #4065, #28124, .T. ) ;
#4022 = CARTESIAN_POINT ( 'NONE',  ( 78.95999731999182814, 64.46943033386045840, 3.516968106976288588 ) ) ;
#4023 = CIRCLE ( 'NONE', #27001, 2.499999999999996891 ) ;
#4024 = CARTESIAN_POINT ( 'NONE',  ( 81.87444285025611634, 65.47866087958064440, 1.319711737399753781 ) ) ;
#4025 = CARTESIAN_POINT ( 'NONE',  ( -63.66774038485660725, 44.17617058018847587, 2.092190587516514100 ) ) ;
#4026 = CARTESIAN_POINT ( 'NONE',  ( 22.31758782591801094, 6.227955964823622459, -0.6941013191108784675 ) ) ;
#4027 = CARTESIAN_POINT ( 'NONE',  ( -64.66796849410253856, 36.23110552202055601, -6.165526157072429569 ) ) ;
#4028 = VERTEX_POINT ( 'NONE', #35194 ) ;
#4029 = CARTESIAN_POINT ( 'NONE',  ( -78.33073954512362036, -5.228239016004201822, 8.428737381316327770 ) ) ;
#4030 = CARTESIAN_POINT ( 'NONE',  ( 26.06851587782132285, 0.7123551559736346350, -4.422872410777025642 ) ) ;
#4031 = ADVANCED_FACE ( 'NONE', ( #32694 ), #19525, .F. ) ;
#4032 = CARTESIAN_POINT ( 'NONE',  ( -1.544665293549569052, -28.25920506871950622, 7.754798119455333705 ) ) ;
#4033 = ORIENTED_EDGE ( 'NONE', *, *, #36814, .F. ) ;
#4034 = CARTESIAN_POINT ( 'NONE',  ( 22.18112716655140204, 5.504259556802007403, 2.539316679596942183 ) ) ;
#4035 = VERTEX_POINT ( 'NONE', #32106 ) ;
#4036 = CARTESIAN_POINT ( 'NONE',  ( 21.73971061288548157, 4.236109109462486977, -2.798397955401881632 ) ) ;
#4037 = LINE ( 'NONE', #20251, #29259 ) ;
#4038 = CARTESIAN_POINT ( 'NONE',  ( 1.700390093233090871, -29.56993018339339940, 7.800000000000000711 ) ) ;
#4039 = CARTESIAN_POINT ( 'NONE',  ( 18.30092389467140634, 7.735072622103469797, 3.062699801917176945 ) ) ;
#4040 = DIRECTION ( 'NONE',  ( -0.6427876096865235978, 0.7660444431189911141, 0.000000000000000000 ) ) ;
#4041 = DIRECTION ( 'NONE',  ( -0.000000000000000000, -0.000000000000000000, 1.000000000000000000 ) ) ;
#4042 = CARTESIAN_POINT ( 'NONE',  ( -63.58520484588292732, 35.72026407271187765, 6.999999999999999112 ) ) ;
#4043 = AXIS2_PLACEMENT_3D ( 'NONE', #30127, #39795, #38619 ) ;
#4044 = CARTESIAN_POINT ( 'NONE',  ( 1.746865321026883189, -25.24062890126829828, 6.954324564059724878 ) ) ;
#4045 = CARTESIAN_POINT ( 'NONE',  ( 35.47974504919754679, -1.182722008973795091, -5.478873071446319187 ) ) ;
#4046 = CARTESIAN_POINT ( 'NONE',  ( -40.97867591359219119, -26.64985754041175525, 6.800000000000000711 ) ) ;
#4047 = EDGE_CURVE ( 'NONE', #32530, #357, #22320, .T. ) ;
#4048 = EDGE_LOOP ( 'NONE', ( #39370, #38765, #30452, #36692, #14431 ) ) ;
#4049 = CARTESIAN_POINT ( 'NONE',  ( 66.89671537544454338, 57.84689108302589489, 3.997688572865332635 ) ) ;
#4050 = CARTESIAN_POINT ( 'NONE',  ( -63.05048152672938500, 38.43432252562566731, 4.010992198732391323 ) ) ;
#4051 = CARTESIAN_POINT ( 'NONE',  ( 88.13894822871212398, -2.422255244508634053, -0.8714879239747004291 ) ) ;
#4052 = AXIS2_PLACEMENT_3D ( 'NONE', #25499, #15615, #27965 ) ;
#4053 = ORIENTED_EDGE ( 'NONE', *, *, #19621, .F. ) ;
#4054 = CARTESIAN_POINT ( 'NONE',  ( -81.73845805635816930, 10.46959273479546049, -1.466899665262664021 ) ) ;
#4055 = SHAPE_DEFINITION_REPRESENTATION ( #35129, #39290 ) ;
#4056 = CARTESIAN_POINT ( 'NONE',  ( 2.903857642304979336, -26.28925757113477957, 7.773839561854631874 ) ) ;
#4057 = CARTESIAN_POINT ( 'NONE',  ( -58.99872204295123623, 28.48507918597136523, -6.834244957304557389 ) ) ;
#4058 = EDGE_CURVE ( 'NONE', #25957, #16025, #11437, .T. ) ;
#4059 = ORIENTED_EDGE ( 'NONE', *, *, #14400, .F. ) ;
#4060 = CARTESIAN_POINT ( 'NONE',  ( 3.992580567114907719, -26.94342455530274449, 7.784725160561908552 ) ) ;
#4061 = ORIENTED_EDGE ( 'NONE', *, *, #23923, .F. ) ;
#4062 = CARTESIAN_POINT ( 'NONE',  ( 80.91727723835752784, 61.27046310099965609, -1.796258654643025476 ) ) ;
#4063 = CARTESIAN_POINT ( 'NONE',  ( 79.59524243168506530, 64.21532580903964060, 3.665158340976913287 ) ) ;
#4065 = VERTEX_POINT ( 'NONE', #17823 ) ;
#4064 = CARTESIAN_POINT ( 'NONE',  ( -1.314124652899413048, -31.14241256655375523, 6.868387053540519815 ) ) ;
#4066 = DIRECTION ( 'NONE',  ( 1.000000000000000000, 7.826543628040252284E-17, -0.000000000000000000 ) ) ;
#4067 = CARTESIAN_POINT ( 'NONE',  ( 1.121324086407811338, -26.64985754041175525, 6.700000000000000178 ) ) ;
#4068 = CARTESIAN_POINT ( 'NONE',  ( 10.50357756723356140, 59.39757829809867928, -1.000000000000000000 ) ) ;
#4069 = EDGE_CURVE ( 'NONE', #4188, #7364, #36876, .T. ) ;
#4070 = EDGE_CURVE ( 'NONE', #9920, #10407, #32597, .T. ) ;
#4071 = CARTESIAN_POINT ( 'NONE',  ( 21.85643539959774273, -9.053501261307662418, 13.64238141129353110 ) ) ;
#4072 = CARTESIAN_POINT ( 'NONE',  ( 23.73916140895965299, 3.555150681598093776, -3.202806708119017021 ) ) ;
#4073 = ORIENTED_EDGE ( 'NONE', *, *, #4447, .F. ) ;
#4074 = CARTESIAN_POINT ( 'NONE',  ( 5.200212981237024579, -29.53471514687662136, 7.710604733652628440 ) ) ;
#4075 = ADVANCED_FACE ( 'NONE', ( #14732 ), #1806, .F. ) ;
#4076 = DIRECTION ( 'NONE',  ( -0.000000000000000000, -0.000000000000000000, 1.000000000000000000 ) ) ;
#4077 = CARTESIAN_POINT ( 'NONE',  ( -0.5575963939758998844, -32.23273358912542363, 7.778495531946298058 ) ) ;
#4078 = AXIS2_PLACEMENT_3D ( 'NONE', #2528, #22476, #35043 ) ;
#4079 = CARTESIAN_POINT ( 'NONE',  ( -73.04755721403003577, -2.452746795641160382, -9.775035012883797947 ) ) ;
#4080 = CARTESIAN_POINT ( 'NONE',  ( 5.143799646208105258, -28.94308837681026247, 7.643192810543818716 ) ) ;
#4081 = DIRECTION ( 'NONE',  ( -0.1736481776669333843, 0.9848077530122075762, 0.000000000000000000 ) ) ;
#4082 = CARTESIAN_POINT ( 'NONE',  ( 80.69089980977662435, 64.07786826041912320, 3.533418250979425412 ) ) ;
#4083 = CARTESIAN_POINT ( 'NONE',  ( 86.89103086197154369, -0.8412156502217053022, -5.497997349500185926 ) ) ;
#4084 = DIRECTION ( 'NONE',  ( 0.000000000000000000, 0.000000000000000000, 1.000000000000000000 ) ) ;
#4085 = PLANE ( 'NONE',  #17432 ) ;
#4086 = B_SPLINE_CURVE_WITH_KNOTS ( 'NONE', 3,
 ( #21493, #36518, #39811, #27852, #36925, #8499, #40404, #17968, #12208, #33458 ),
 .UNSPECIFIED., .F., .F.,
 ( 4, 3, 3, 4 ),
 ( 8.940560153363745023E-19, 3.025570593003112336E-05, 6.051145698344056074E-05, 6.468151674593758404E-05 ),
 .UNSPECIFIED. ) ;
#4087 = CARTESIAN_POINT ( 'NONE',  ( 3.922602026865150471, -26.86590094501167059, 7.700536657684220465 ) ) ;
#4088 = FACE_OUTER_BOUND ( 'NONE', #21208, .T. ) ;
#4089 = CARTESIAN_POINT ( 'NONE',  ( -0.3795852241544983574, -26.88035727981826994, 6.865312560952602894 ) ) ;
#4090 = CARTESIAN_POINT ( 'NONE',  ( 4.700764115346282246, -27.97063167234916392, 7.761597726988848756 ) ) ;
#4091 = CARTESIAN_POINT ( 'NONE',  ( 5.551251297819359110, -25.49307895267003587, 6.700000000000000178 ) ) ;
#4092 = EDGE_CURVE ( 'NONE', #5244, #28284, #2041, .T. ) ;
#4093 = CARTESIAN_POINT ( 'NONE',  ( 36.79828219115022137, -2.555128534534287787, 5.949659924383641219 ) ) ;
#4094 = DIRECTION ( 'NONE',  ( -0.000000000000000000, -1.000000000000000000, -0.000000000000000000 ) ) ;
#4095 = CARTESIAN_POINT ( 'NONE',  ( 85.45255010372768822, 2.373364497502822967, 3.195069691434311743 ) ) ;
#4097 = CARTESIAN_POINT ( 'NONE',  ( -70.92837670882107659, -23.80776546975053165, 6.000000000000005329 ) ) ;
#4096 = CARTESIAN_POINT ( 'NONE',  ( 80.84084779726516956, 63.39242392479005161, -3.526329879082124030 ) ) ;
#4098 = DIRECTION ( 'NONE',  ( -0.3103887796125159859, -0.9506097019758703581, 0.000000000000000000 ) ) ;
#4099 = DIRECTION ( 'NONE',  ( 0.000000000000000000, -0.000000000000000000, -1.000000000000000000 ) ) ;
#4100 = ORIENTED_EDGE ( 'NONE', *, *, #38297, .T. ) ;
#4101 = DIRECTION ( 'NONE',  ( -1.000000000000000000, 0.000000000000000000, 0.000000000000000000 ) ) ;
#4102 = ADVANCED_FACE ( 'NONE', ( #21142 ), #8146, .T. ) ;
#4103 = ORIENTED_EDGE ( 'NONE', *, *, #34680, .T. ) ;
#4104 = CARTESIAN_POINT ( 'NONE',  ( -72.92401200329621247, 7.089954214640987296, 9.800610954731245883 ) ) ;
#4105 = VERTEX_POINT ( 'NONE', #33708 ) ;
#4106 = CARTESIAN_POINT ( 'NONE',  ( 81.03127633846453648, 61.72971393008351981, -2.526545245021137198 ) ) ;
#4107 = DIRECTION ( 'NONE',  ( 0.000000000000000000, 0.000000000000000000, -1.000000000000000000 ) ) ;
#4108 = CARTESIAN_POINT ( 'NONE',  ( 22.53938003481075825, 1.184789744452465321, 6.008811300886961249 ) ) ;
#4111 = ORIENTED_EDGE ( 'NONE', *, *, #40113, .F. ) ;
#4110 = ORIENTED_EDGE ( 'NONE', *, *, #39600, .T. ) ;
#4109 = VECTOR ( 'NONE', #24731, 1000.000000000000000 ) ;
#4112 = EDGE_CURVE ( 'NONE', #1778, #29684, #30098, .T. ) ;
#4113 = DIRECTION ( 'NONE',  ( -0.000000000000000000, -0.000000000000000000, 1.000000000000000000 ) ) ;
#4114 = ADVANCED_FACE ( 'NONE', ( #12678 ), #23820, .F. ) ;
#4115 = DIRECTION ( 'NONE',  ( 0.000000000000000000, 0.000000000000000000, 1.000000000000000000 ) ) ;
#4117 = CARTESIAN_POINT ( 'NONE',  ( 85.76128207622278410, 2.026582092692974069, 3.826057417255781967 ) ) ;
#4116 = CARTESIAN_POINT ( 'NONE',  ( 1.074608721727911442, -26.22801491291194864, 7.695279973900954751 ) ) ;
#4118 = FACE_OUTER_BOUND ( 'NONE', #13101, .T. ) ;
#4119 = CARTESIAN_POINT ( 'NONE',  ( 72.25564410411975302, 59.56945073910184618, 3.929231508797896399 ) ) ;
#4120 = ORIENTED_EDGE ( 'NONE', *, *, #7991, .T. ) ;
#4121 = CARTESIAN_POINT ( 'NONE',  ( 23.23159003004921885, 3.295630425265384300, -3.830492098241911503 ) ) ;
#4122 = VERTEX_POINT ( 'NONE', #28332 ) ;
#4123 = EDGE_CURVE ( 'NONE', #15644, #39711, #6523, .T. ) ;
#4124 = ORIENTED_EDGE ( 'NONE', *, *, #17105, .T. ) ;
#4125 = CARTESIAN_POINT ( 'NONE',  ( 21.85643539959778536, -7.083161344002194326, -10.43125315386002860 ) ) ;
#4126 = CARTESIAN_POINT ( 'NONE',  ( 20.16883043528743968, 11.76570021211175643, 3.257865388789312089 ) ) ;
#4127 = LINE ( 'NONE', #2663, #8332 ) ;
#4128 = CARTESIAN_POINT ( 'NONE',  ( 81.57183863168549465, 63.40013557970607394, 3.079343812564428351 ) ) ;
#4129 = FACE_OUTER_BOUND ( 'NONE', #15584, .T. ) ;
#4130 = VERTEX_POINT ( 'NONE', #6109 ) ;
#4131 = CARTESIAN_POINT ( 'NONE',  ( 19.69441324270408700, -2.725662423435629922, 3.280187516344912346 ) ) ;
#4132 = CARTESIAN_POINT ( 'NONE',  ( 5.068171392735082215, -29.10285614499638740, 6.863904403958576594 ) ) ;
#4133 = CARTESIAN_POINT ( 'NONE',  ( 16.00969967615263556, -3.370281526357195467, -2.705098849150198603 ) ) ;
#4134 = CARTESIAN_POINT ( 'NONE',  ( 32.78094590778558626, -0.9280580154095039447, -5.322657437719364282 ) ) ;
#4135 = DIRECTION ( 'NONE',  ( 1.000000000000000000, 0.000000000000000000, 0.000000000000000000 ) ) ;
#4136 = CARTESIAN_POINT ( 'NONE',  ( -62.92837670882107659, -49.49506129533733656, -6.000000000000000000 ) ) ;
#4137 = CARTESIAN_POINT ( 'NONE',  ( 0.1120526303552441955, -32.69643921324515645, 7.139344958878412584 ) ) ;
#4138 = ORIENTED_EDGE ( 'NONE', *, *, #11281, .F. ) ;
#4139 = CARTESIAN_POINT ( 'NONE',  ( -15.07867591359219439, -24.55319635012989110, 6.700000000000000178 ) ) ;
#4140 = AXIS2_PLACEMENT_3D ( 'NONE', #17782, #34902, #6266 ) ;
#4141 = DIRECTION ( 'NONE',  ( 0.000000000000000000, -0.000000000000000000, -1.000000000000000000 ) ) ;
#4142 = CARTESIAN_POINT ( 'NONE',  ( 28.23003454072220819, -3.405378548512706161, 4.612377654681626638 ) ) ;
#4143 = ORIENTED_EDGE ( 'NONE', *, *, #24636, .T. ) ;
#4144 = VERTEX_POINT ( 'NONE', #18646 ) ;
#4145 = CARTESIAN_POINT ( 'NONE',  ( 36.20113637138914697, -3.651277154294600091, 5.717575700238314518 ) ) ;
#4146 = CARTESIAN_POINT ( 'NONE',  ( 2.186430707228644188, -33.03594076280592162, 7.753200566781576875 ) ) ;
#4147 = CARTESIAN_POINT ( 'NONE',  ( 87.45676830308305227, -1.940095815629343967, 3.699365911462623391 ) ) ;
#4148 = ORIENTED_EDGE ( 'NONE', *, *, #23205, .T. ) ;
#4149 = ADVANCED_FACE ( 'NONE', ( #33648 ), #24150, .F. ) ;
#4150 = VERTEX_POINT ( 'NONE', #40004 ) ;
#4151 = DIRECTION ( 'NONE',  ( 0.000000000000000000, 0.000000000000000000, -1.000000000000000000 ) ) ;
#4152 = ORIENTED_EDGE ( 'NONE', *, *, #32289, .F. ) ;
#4153 = CARTESIAN_POINT ( 'NONE',  ( -4.444218661349752963, -35.94265729135299381, 6.000000000000000000 ) ) ;
#4154 = ORIENTED_EDGE ( 'NONE', *, *, #39587, .F. ) ;
#4155 = EDGE_CURVE ( 'NONE', #10309, #8273, #5221, .T. ) ;
#4156 = CARTESIAN_POINT ( 'NONE',  ( 82.43319509988585025, 63.84109541104518115, -1.838010297257801851 ) ) ;
#4157 = EDGE_CURVE ( 'NONE', #27773, #21932, #29647, .T. ) ;
#4158 = CARTESIAN_POINT ( 'NONE',  ( 1.551251297819356001, -26.64985754041175525, 6.800000000000000711 ) ) ;
#4159 = ORIENTED_EDGE ( 'NONE', *, *, #19877, .F. ) ;
#4160 = CARTESIAN_POINT ( 'NONE',  ( 75.82377327986996818, 62.28299708301697279, -3.825872951952260959 ) ) ;
#4162 = CARTESIAN_POINT ( 'NONE',  ( 4.382959869488853855, -27.33051813421351994, 7.773839561854632763 ) ) ;
#4161 = CARTESIAN_POINT ( 'NONE',  ( 2.394970551016177840, -26.13952796232410591, 6.864368109219935121 ) ) ;
#4163 = CARTESIAN_POINT ( 'NONE',  ( 6.040270069758088667, -32.09115252335679003, 7.635761828346577573 ) ) ;
#4164 = CARTESIAN_POINT ( 'NONE',  ( 78.09760114435867706, 60.38799743245716911, 2.844364419925230258 ) ) ;
#4165 = AXIS2_PLACEMENT_3D ( 'NONE', #661, #38303, #22686 ) ;
#4166 = CARTESIAN_POINT ( 'NONE',  ( 1.700390093233090871, -29.56993018339339940, 7.800000000000000711 ) ) ;
#4167 = EDGE_CURVE ( 'NONE', #14186, #7610, #11775, .T. ) ;
#4168 = CARTESIAN_POINT ( 'NONE',  ( -25.07867591359219617, -24.55319635012989110, 6.700000000000000178 ) ) ;
#4169 = ADVANCED_FACE ( 'NONE', ( #18377 ), #14877, .F. ) ;
#4170 = CARTESIAN_POINT ( 'NONE',  ( 1.869561550574128761, -26.07402100007339740, 7.013842709614101167 ) ) ;
#4171 = CARTESIAN_POINT ( 'NONE',  ( 1.686887486498407140, -26.06995622926011436, 7.635761828346576685 ) ) ;
#4172 = CARTESIAN_POINT ( 'NONE',  ( 79.73837173991839222, 66.20136991484933731, 1.918505602738378446 ) ) ;
#4173 = CARTESIAN_POINT ( 'NONE',  ( -0.9644972916791141326, -31.83894080698376783, 7.651421919295144924 ) ) ;
#4174 = CARTESIAN_POINT ( 'NONE',  ( 26.56638717734885802, 2.990222579127657099, 1.122734419917069237 ) ) ;
#4175 = DIRECTION ( 'NONE',  ( -0.000000000000000000, -0.000000000000000000, 1.000000000000000000 ) ) ;
#4176 = LINE ( 'NONE', #38729, #9050 ) ;
#4177 = CARTESIAN_POINT ( 'NONE',  ( 4.728387659347194294, -31.31879373379047848, 7.767720160662276996 ) ) ;
#4178 = CARTESIAN_POINT ( 'NONE',  ( 0.7337844087288916128, -26.31022567980965121, 6.929923840112065747 ) ) ;
#4179 = VECTOR ( 'NONE', #33858, 1000.000000000000000 ) ;
#4180 = CARTESIAN_POINT ( 'NONE',  ( -32.44874870218063734, -26.64985754041175525, 6.700000000000000178 ) ) ;
#4181 = CARTESIAN_POINT ( 'NONE',  ( 36.68200451011485086, -3.313387469113171946, -5.912010938468631238 ) ) ;
#4182 = CARTESIAN_POINT ( 'NONE',  ( 1.050623329351162871, -32.90726492125749303, 7.785172627573962778 ) ) ;
#4183 = LINE ( 'NONE', #7050, #18704 ) ;
#4184 = CARTESIAN_POINT ( 'NONE',  ( 3.297628331390787260, -32.57140239904362033, 7.759451378593095860 ) ) ;
#4185 = CARTESIAN_POINT ( 'NONE',  ( -63.57019645983813660, 43.64021813969844743, -2.910064772521099741 ) ) ;
#4186 = CARTESIAN_POINT ( 'NONE',  ( -4.890026461918812295, -8.951974136083761024, 6.000000000000000000 ) ) ;
#4187 = LINE ( 'NONE', #14232, #68 ) ;
#4188 = VERTEX_POINT ( 'NONE', #11171 ) ;
#4189 = CARTESIAN_POINT ( 'NONE',  ( 32.91478736177253239, -0.5485403146597650492, 5.320368748126441005 ) ) ;
#4190 = DIRECTION ( 'NONE',  ( -0.7660444431189800119, -0.6427876096865369204, 0.000000000000000000 ) ) ;
#4191 = CARTESIAN_POINT ( 'NONE',  ( 67.15438370417800229, 58.05139456359000150, -3.999036733496184048 ) ) ;
#4192 = CARTESIAN_POINT ( 'NONE',  ( 3.041304459685018724, -26.33696975259048756, 6.880828092187095457 ) ) ;
#4193 = ORIENTED_EDGE ( 'NONE', *, *, #35353, .T. ) ;
#4194 = DIRECTION ( 'NONE',  ( -0.000000000000000000, -0.000000000000000000, 1.000000000000000000 ) ) ;
#4195 = CARTESIAN_POINT ( 'NONE',  ( -1.600607472504411488, -28.40656649520510157, 7.700536657684219577 ) ) ;
#4196 = CARTESIAN_POINT ( 'NONE',  ( 23.89044766034434275, 3.056531940009395765, 3.748979796177386081 ) ) ;
#4197 = CARTESIAN_POINT ( 'NONE',  ( 0.9148132382037100774, -32.87793322582781030, 6.997764925645181933 ) ) ;
#4198 = CARTESIAN_POINT ( 'NONE',  ( 0.3249534634392911014, -32.78834191550933497, 6.945385021654666424 ) ) ;
#4199 = CARTESIAN_POINT ( 'NONE',  ( -0.5626977249550375593, -26.90001753928526540, 7.750000000000002665 ) ) ;
#4200 = ORIENTED_EDGE ( 'NONE', *, *, #10963, .T. ) ;
#4201 = CARTESIAN_POINT ( 'NONE',  ( -71.72837670882105954, -34.30579396504363388, 1.385640646055090519 ) ) ;
#4202 = CARTESIAN_POINT ( 'NONE',  ( 14.75430999618867745, -4.622527584820372404, 2.500000000000000888 ) ) ;
#4204 = AXIS2_PLACEMENT_3D ( 'NONE', #11892, #27756, #18694 ) ;
#4203 = CARTESIAN_POINT ( 'NONE',  ( 81.23507808130547403, 61.62583295638711434, 2.125034277891707291 ) ) ;
#4205 = CARTESIAN_POINT ( 'NONE',  ( -0.03438793071513444183, -32.60975724081566796, 7.640616322432101981 ) ) ;
#4206 = EDGE_LOOP ( 'NONE', ( #22146, #8567, #25360, #23422, #15252 ) ) ;
#4207 = CARTESIAN_POINT ( 'NONE',  ( 80.20105671851041507, 61.18620973470589774, -2.431999527814464379 ) ) ;
#4209 = CARTESIAN_POINT ( 'NONE',  ( -1.713501025485110407, -28.79831591363838683, 6.891695036779140970 ) ) ;
#4208 = CARTESIAN_POINT ( 'NONE',  ( 26.70483259202675086, 0.9606887959971135427, 4.381135443176162880 ) ) ;
#4210 = CARTESIAN_POINT ( 'NONE',  ( 81.59312859631556591, 63.05267747590616523, -3.015199126117770412 ) ) ;
#4211 = CARTESIAN_POINT ( 'NONE',  ( 78.24346468842466606, 65.07400588416957987, 2.889371261047450457 ) ) ;
#4212 = EDGE_CURVE ( 'NONE', #33614, #29368, #1952, .T. ) ;
#4213 = LINE ( 'NONE', #23142, #19482 ) ;
#4214 = EDGE_CURVE ( 'NONE', #35240, #7017, #18171, .T. ) ;
#4215 = CARTESIAN_POINT ( 'NONE',  ( 82.39191784114052552, 64.57324092874044652, 1.480606629405690544 ) ) ;
#4216 =( BOUNDED_CURVE ( )  B_SPLINE_CURVE ( 3, ( #2691, #5342, #24688, #39922 ),
 .UNSPECIFIED., .F., .T. ) 
 B_SPLINE_CURVE_WITH_KNOTS ( ( 4, 4 ),
 ( 1.347909859412855127, 1.534781240595299634 ),
 .UNSPECIFIED. ) 
 CURVE ( )  GEOMETRIC_REPRESENTATION_ITEM ( )  RATIONAL_B_SPLINE_CURVE ( ( 1.000000000000000000, 0.9970920404276226723, 0.9970920404276226723, 1.000000000000000000 ) ) 
 REPRESENTATION_ITEM ( '' )  );
#4217 = CARTESIAN_POINT ( 'NONE',  ( -64.08758708074093136, 43.28886537931755640, 1.984762278319444961 ) ) ;
#4218 = CARTESIAN_POINT ( 'NONE',  ( 24.55145103709714505, -1.086933616027371263, 6.883468691731016165 ) ) ;
#4219 = CARTESIAN_POINT ( 'NONE',  ( -64.14095127866889356, 35.19432717188715287, -4.537732464557278966 ) ) ;
#4220 = EDGE_LOOP ( 'NONE', ( #29010, #34951, #25458, #26842 ) ) ;
#4221 = CARTESIAN_POINT ( 'NONE',  ( -76.32424250352048034, -4.240740262105982872, 8.445734442623528793 ) ) ;
#4222 = LINE ( 'NONE', #1144, #18011 ) ;
#4223 = CARTESIAN_POINT ( 'NONE',  ( -0.09336860625537750369, -32.55799552926065843, 7.785593909369614707 ) ) ;
#4224 = DIRECTION ( 'NONE',  ( -0.000000000000000000, -1.000000000000000000, -0.000000000000000000 ) ) ;
#4225 = CARTESIAN_POINT ( 'NONE',  ( 20.91978843656600517, 4.581251045227689112, -2.652517874115063012 ) ) ;
#4226 = CARTESIAN_POINT ( 'NONE',  ( -1.337427566997555717, -27.83163680677632001, 7.635761828346574021 ) ) ;
#4227 = CARTESIAN_POINT ( 'NONE',  ( 5.127407220394881726, -30.28097170179577091, 6.864216812889599062 ) ) ;
#4228 = CARTESIAN_POINT ( 'NONE',  ( 5.198146613259219784, -29.69565482044479410, 6.867199677474200570 ) ) ;
#4229 = PRODUCT ( 'Triangular punching die', 'Triangular punching die', '', ( #32256 ) ) ;
#4230 = CARTESIAN_POINT ( 'NONE',  ( -0.6172017013887949322, -27.07259496238298269, 7.139196562012275038 ) ) ;
#4231 = FACE_OUTER_BOUND ( 'NONE', #31859, .T. ) ;
#4232 = AXIS2_PLACEMENT_3D ( 'NONE', #23405, #35581, #23014 ) ;
#4233 = PLANE ( 'NONE',  #15168 ) ;
#4234 = AXIS2_PLACEMENT_3D ( 'NONE', #39315, #38712, #39111 ) ;
#4235 = CARTESIAN_POINT ( 'NONE',  ( 5.200390093233090205, -29.56993018339339940, 6.929570838012950595 ) ) ;
#4236 = ORIENTED_EDGE ( 'NONE', *, *, #11636, .T. ) ;
#4237 = CARTESIAN_POINT ( 'NONE',  ( 66.56396446968585678, 57.85070090013417854, 3.999903336036485069 ) ) ;
#4238 = CIRCLE ( 'NONE', #26562, 12.73502530973474300 ) ;
#4239 = CARTESIAN_POINT ( 'NONE',  ( -64.08758708074093136, 38.76906266698302517, 3.999999999999998668 ) ) ;
#4240 = CARTESIAN_POINT ( 'NONE',  ( 84.10013685850573495, 3.017793503712738357, 0.3246723698904760980 ) ) ;
#4241 = AXIS2_PLACEMENT_3D ( 'NONE', #40332, #15841, #31299 ) ;
#4242 = LINE ( 'NONE', #16766, #24136 ) ;
#4243 = ORIENTED_EDGE ( 'NONE', *, *, #22801, .T. ) ;
#4244 = CARTESIAN_POINT ( 'NONE',  ( 26.60765709881297880, 1.631430624340022506, 4.332177513178613104 ) ) ;
#4245 = PRODUCT_CONTEXT ( 'NONE', #14482, 'mechanical' ) ;
#4246 = CARTESIAN_POINT ( 'NONE',  ( 2.896878217289016622, -26.28424773566757722, 7.767720160662274331 ) ) ;
#4247 = CARTESIAN_POINT ( 'NONE',  ( 1.153797596015393667, -26.12793346271676498, 7.785593909369613819 ) ) ;
#4248 = ORIENTED_EDGE ( 'NONE', *, *, #11834, .F. ) ;
#4249 = CARTESIAN_POINT ( 'NONE',  ( -1.750280548689878701, -28.98434346021053543, 7.646866513072558824 ) ) ;
#4250 = ADVANCED_FACE ( 'NONE', ( #5837 ), #36314, .T. ) ;
#4251 = VERTEX_POINT ( 'NONE', #20651 ) ;
#4252 = ORIENTED_EDGE ( 'NONE', *, *, #35132, .F. ) ;
#4253 = CARTESIAN_POINT ( 'NONE',  ( 78.52976371562807856, 65.87711177338782420, -1.796258654643035912 ) ) ;
#4254 = CARTESIAN_POINT ( 'NONE',  ( 4.983308922979784228, -28.35648716565642857, 7.750000000000000000 ) ) ;
#4255 = CARTESIAN_POINT ( 'NONE',  ( 80.71678001510488798, 62.11300466482759219, 3.061371641637220087 ) ) ;
#4256 = CARTESIAN_POINT ( 'NONE',  ( -1.269366464186706844, -31.22539145627230184, 6.892063359921934307 ) ) ;
#4257 = CARTESIAN_POINT ( 'NONE',  ( 1.121324086407811338, -26.64985754041175525, 6.700000000000000178 ) ) ;
#4258 = ADVANCED_FACE ( 'NONE', ( #11984 ), #15087, .F. ) ;
#4259 = DIRECTION ( 'NONE',  ( 0.000000000000000000, 0.000000000000000000, -1.000000000000000000 ) ) ;
#4260 = CARTESIAN_POINT ( 'NONE',  ( 5.986119168300054305, -26.95491573082899706, 7.754798119455333705 ) ) ;
#4261 = CARTESIAN_POINT ( 'NONE',  ( 33.54884098819741212, -4.040961204078771019, -4.876534918468718338 ) ) ;
#4262 = CARTESIAN_POINT ( 'NONE',  ( 4.163022776446456241, -25.19622345277205966, 7.695279973900954751 ) ) ;
#4263 = CARTESIAN_POINT ( 'NONE',  ( 21.98979295893775543, 5.607672701399281756, -3.095502674479804206 ) ) ;
#4264 = CARTESIAN_POINT ( 'NONE',  ( 77.97558924392689050, 65.55221975275186708, -1.909876039719648588 ) ) ;
#4265 = VERTEX_POINT ( 'NONE', #37115 ) ;
#4266 = AXIS2_PLACEMENT_3D ( 'NONE', #6609, #16263, #22463 ) ;
#4267 = CARTESIAN_POINT ( 'NONE',  ( -1.773217931840104900, -29.99897723786583015, 6.998987538705435441 ) ) ;
#4268 = CARTESIAN_POINT ( 'NONE',  ( 4.281704324602110923, -27.35705493990426262, 7.692469944509198854 ) ) ;
#4269 = CARTESIAN_POINT ( 'NONE',  ( -75.59970171100725622, -3.666675714033016842, -8.878492054693071012 ) ) ;
#4270 = CARTESIAN_POINT ( 'NONE',  ( 4.720365337249898374, -27.80081420075986287, 7.743886751744251562 ) ) ;
#4271 = LINE ( 'NONE', #39016, #18168 ) ;
#4272 = CARTESIAN_POINT ( 'NONE',  ( 81.03825699591070020, 63.48946937969523674, 3.448515284080272192 ) ) ;
#4273 = DIRECTION ( 'NONE',  ( 0.000000000000000000, 0.000000000000000000, 1.000000000000000000 ) ) ;
#4274 = CARTESIAN_POINT ( 'NONE',  ( 3.881713901294285396, -26.96188585715140107, 7.763628509615284834 ) ) ;
#4275 = CARTESIAN_POINT ( 'NONE',  ( -1.576116513076069259, -30.80058222959184633, 7.700536657684210695 ) ) ;
#4276 = DIRECTION ( 'NONE',  ( 1.000000000000000000, -0.000000000000000000, 0.000000000000000000 ) ) ;
#4277 = CARTESIAN_POINT ( 'NONE',  ( 33.93654037581948302, -1.338830054478469478, 5.503015902613915600 ) ) ;
#4278 = DIRECTION ( 'NONE',  ( -0.000000000000000000, -0.000000000000000000, -1.000000000000000000 ) ) ;
#4279 = CARTESIAN_POINT ( 'NONE',  ( 15.84347261764352766, 10.40642223222415907, -2.679155096453247786 ) ) ;
#4280 = CARTESIAN_POINT ( 'NONE',  ( 1.700390093233090871, -29.56993018339339940, 7.750000000000000888 ) ) ;
#4281 = FACE_OUTER_BOUND ( 'NONE', #22061, .T. ) ;
#4282 = B_SPLINE_CURVE_WITH_KNOTS ( 'NONE', 3,
 ( #23041, #34812, #617, #35607, #35010, #9868, #4311, #16832, #25721, #10261, #10059, #10657, #29417, #3925, #1231, #26332, #13764, #38866, #19135, #22442, #6784, #31908, #14753, #33320, #13957, #10855 ),
 .UNSPECIFIED., .F., .F.,
 ( 4, 2, 2, 2, 2, 2, 2, 2, 2, 2, 2, 2, 4 ),
 ( 0.000000000000000000, 0.0001695542964127800731, 0.0003391085928255601462, 0.0005086628892383401922, 0.0006782171856511202924, 0.001017325778476677999, 0.001356434371302235814, 0.002034651556953352095, 0.002712868742604468593, 0.003391085928255584223, 0.004069303113906699854, 0.004747520299557816785, 0.005425737485208931982 ),
 .UNSPECIFIED. ) ;
#4283 = CARTESIAN_POINT ( 'NONE',  ( 69.23715119732055712, 58.71109548446294468, 3.988427515945585089 ) ) ;
#4284 = CARTESIAN_POINT ( 'NONE',  ( 29.10196052430525171, 0.3604245502769343190, 4.748462792029568114 ) ) ;
#4285 = ADVANCED_FACE ( 'NONE', ( #2359 ), #8084, .T. ) ;
#4286 = FACE_OUTER_BOUND ( 'NONE', #22251, .T. ) ;
#4287 = AXIS2_PLACEMENT_3D ( 'NONE', #2046, #29624, #29430 ) ;
#4288 = CARTESIAN_POINT ( 'NONE',  ( 86.29974207331044056, 1.340767688666749446, -5.501321414410665689 ) ) ;
#4290 = CARTESIAN_POINT ( 'NONE',  ( -0.4761956913552217729, -26.82902173683139679, 6.863805608295729499 ) ) ;
#4289 = CARTESIAN_POINT ( 'NONE',  ( 79.39927235112092774, 65.46614203786572261, -2.932725070486261743 ) ) ;
#4291 = CARTESIAN_POINT ( 'NONE',  ( -1.381852710791847461, -31.22270215869128762, 7.766640943994346458 ) ) ;
#4292 = AXIS2_PLACEMENT_3D ( 'NONE', #31777, #493, #19413 ) ;
#4293 = EDGE_CURVE ( 'NONE', #40685, #23776, #35087, .T. ) ;
#4294 = LINE ( 'NONE', #23612, #3781 ) ;
#4295 = CARTESIAN_POINT ( 'NONE',  ( -59.65099889957326695, 26.74201272916463878, 6.661192808835134649 ) ) ;
#4296 = VERTEX_POINT ( 'NONE', #36513 ) ;
#4297 = FACE_OUTER_BOUND ( 'NONE', #36494, .T. ) ;
#4298 = DIRECTION ( 'NONE',  ( 0.000000000000000000, 0.000000000000000000, 1.000000000000000000 ) ) ;
#4299 = VECTOR ( 'NONE', #29453, 1000.000000000000000 ) ;
#4300 = ORIENTED_EDGE ( 'NONE', *, *, #28965, .T. ) ;
#4301 = EDGE_CURVE ( 'NONE', #6453, #2951, #8287, .T. ) ;
#4302 = ORIENTED_EDGE ( 'NONE', *, *, #10002, .F. ) ;
#4303 = VERTEX_POINT ( 'NONE', #33453 ) ;
#4304 = CARTESIAN_POINT ( 'NONE',  ( 80.80704226153129355, 62.39036624599364700, -3.220356845322062789 ) ) ;
#4305 = CARTESIAN_POINT ( 'NONE',  ( -10.24874870218063450, -26.64985754041175525, 6.800000000000000711 ) ) ;
#4306 = CARTESIAN_POINT ( 'NONE',  ( 81.09335400879911049, 61.74513338965306275, 2.494286432550478771 ) ) ;
#4307 = CARTESIAN_POINT ( 'NONE',  ( 25.21589077596340189, 0.9012383917972676128, 4.613794564236588513 ) ) ;
#4308 = EDGE_LOOP ( 'NONE', ( #6577, #29939, #38675, #39208 ) ) ;
#4309 = CARTESIAN_POINT ( 'NONE',  ( -0.06885977712395061068, -32.47334897749556859, 7.782034975670476307 ) ) ;
#4310 = EDGE_CURVE ( 'NONE', #19528, #21404, #30343, .T. ) ;
#4312 = CARTESIAN_POINT ( 'NONE',  ( -6.978675913592191193, -26.64985754041175525, 6.800000000000000711 ) ) ;
#4311 = CARTESIAN_POINT ( 'NONE',  ( -58.97292984558871609, 28.26388549929947303, -6.370425507473826521 ) ) ;
#4313 = DIRECTION ( 'NONE',  ( -0.000000000000000000, -0.000000000000000000, 1.000000000000000000 ) ) ;
#4314 = CARTESIAN_POINT ( 'NONE',  ( -64.08758708074196875, 43.90637424960519297, -1.960639441496169200 ) ) ;
#4315 = CARTESIAN_POINT ( 'NONE',  ( 71.19973236181560594, 58.84349373463830091, 3.887826097256417590 ) ) ;
#4316 = CARTESIAN_POINT ( 'NONE',  ( 22.11632824126515828, 4.958352940722863700, -3.426487884367986236 ) ) ;
#4317 = EDGE_LOOP ( 'NONE', ( #4193, #15572, #8359, #39908, #36854 ) ) ;
#4318 = CYLINDRICAL_SURFACE ( 'NONE', #39498, 7.744449365083023729 ) ;
#4319 = VERTEX_POINT ( 'NONE', #39804 ) ;
#4320 = AXIS2_PLACEMENT_3D ( 'NONE', #3092, #18276, #15609 ) ;
#4321 = CARTESIAN_POINT ( 'NONE',  ( 21.85643539959778892, -9.157157878381195104, -8.039778668638760450 ) ) ;
#4322 = AXIS2_PLACEMENT_3D ( 'NONE', #14388, #15006, #21195 ) ;
#4323 = CARTESIAN_POINT ( 'NONE',  ( 21.86904452675153365, 4.504091705278521651, 2.554698571754111767E-12 ) ) ;
#4324 = DIRECTION ( 'NONE',  ( 1.000000000000000000, 0.000000000000000000, 0.000000000000000000 ) ) ;
#4325 = CARTESIAN_POINT ( 'NONE',  ( 80.93493477626120125, 64.98323193449216717, 3.125232205748817549 ) ) ;
#4326 = CARTESIAN_POINT ( 'NONE',  ( 86.85482141032015591, 0.6757441427909987031, 5.750446197363288547 ) ) ;
#4327 = CARTESIAN_POINT ( 'NONE',  ( -17.27251170661583402, 3.729367930467589076, -2.500000000000000444 ) ) ;
#4328 = ORIENTED_EDGE ( 'NONE', *, *, #26787, .F. ) ;
#4329 = VECTOR ( 'NONE', #5012, 1000.000000000000000 ) ;
#4330 = CARTESIAN_POINT ( 'NONE',  ( -78.72866883428119422, -5.350567248293963019, 8.033035618889639906 ) ) ;
#4331 = ADVANCED_FACE ( 'NONE', ( #11574 ), #22513, .F. ) ;
#4332 = CARTESIAN_POINT ( 'NONE',  ( 14.76950060579820345, -5.972576308483009910, 2.511535789893701409 ) ) ;
#4333 = CARTESIAN_POINT ( 'NONE',  ( 5.078111950526700724, -29.18133977915486099, 6.920489980334476599 ) ) ;
#4334 = CARTESIAN_POINT ( 'NONE',  ( 33.12369938294775551, -3.163197387429788510, -5.376152407042375181 ) ) ;
#4335 = CARTESIAN_POINT ( 'NONE',  ( 30.51439263097747556, -0.1427504069471233206, -4.968906982075368184 ) ) ;
#4336 = CARTESIAN_POINT ( 'NONE',  ( 5.090329724959301139, -29.91149280961422008, 7.505001789837621118 ) ) ;
#4337 = CARTESIAN_POINT ( 'NONE',  ( 84.10579224183346980, 3.010952253929020550, -0.2616020758091565646 ) ) ;
#4338 = CARTESIAN_POINT ( 'NONE',  ( -0.5096406291778409203, -26.98618015562372108, 7.721096864323899744 ) ) ;
#4339 = CARTESIAN_POINT ( 'NONE',  ( -36.97867591359219119, -26.64985754041175525, 6.700000000000000178 ) ) ;
#4340 = CARTESIAN_POINT ( 'NONE',  ( 5.018694563533798281, -28.47163790933613825, 7.771081512783701406 ) ) ;
#4341 = VERTEX_POINT ( 'NONE', #25585 ) ;
#4342 = VERTEX_POINT ( 'NONE', #22312 ) ;
#4343 = CARTESIAN_POINT ( 'NONE',  ( 35.83251579909378393, -3.729987874846103058, 5.623171243541962738 ) ) ;
#4344 = CARTESIAN_POINT ( 'NONE',  ( 14.77222811005485603, -4.461988841550141416, 2.511961482897715481 ) ) ;
#4345 = ADVANCED_FACE ( 'NONE', ( #37517 ), #750, .T. ) ;
#4346 = EDGE_CURVE ( 'NONE', #13345, #28759, #33084, .T. ) ;
#4347 = CARTESIAN_POINT ( 'NONE',  ( 66.27376694609004915, 57.73522568913436004, -4.000000000000000000 ) ) ;
#4348 = CARTESIAN_POINT ( 'NONE',  ( 87.92068663493991210, -2.504771375202706540, 0.3618066692888307623 ) ) ;
#4349 = EDGE_CURVE ( 'NONE', #9974, #30067, #24388, .T. ) ;
#4350 = ORIENTED_EDGE ( 'NONE', *, *, #15951, .T. ) ;
#4351 = VECTOR ( 'NONE', #19120, 1000.000000000000000 ) ;
#4352 = CARTESIAN_POINT ( 'NONE',  ( -1.799609906766908685, -29.56993018339339940, 7.800000000000000711 ) ) ;
#4353 = ORIENTED_EDGE ( 'NONE', *, *, #507, .T. ) ;
#4354 = CARTESIAN_POINT ( 'NONE',  ( -57.68674048389793541, 29.08812126441105406, -4.503248736989433176 ) ) ;
#4355 = CARTESIAN_POINT ( 'NONE',  ( 3.799575776136275174, -32.37054073623617256, 6.951256099901591767 ) ) ;
#4356 = ORIENTED_EDGE ( 'NONE', *, *, #3856, .T. ) ;
#4357 = CARTESIAN_POINT ( 'NONE',  ( 22.08043625007045563, 5.168148467668603807, 3.316046242248380960 ) ) ;
#4358 = AXIS2_PLACEMENT_3D ( 'NONE', #9720, #18776, #27634 ) ;
#4359 = CARTESIAN_POINT ( 'NONE',  ( 82.39984057372335258, 63.46184634947035619, -2.021051955677194201 ) ) ;
#4360 = DIRECTION ( 'NONE',  ( 1.000000000000000000, 0.000000000000000000, 0.000000000000000000 ) ) ;
#4361 = CARTESIAN_POINT ( 'NONE',  ( 3.852146645688039328, -32.33035474113215457, 7.750000000000000888 ) ) ;
#4362 = ORIENTED_EDGE ( 'NONE', *, *, #2791, .T. ) ;
#4363 = CARTESIAN_POINT ( 'NONE',  ( 74.67253486855700828, 63.25418332940030552, -3.074209570828856819 ) ) ;
#4365 = DIRECTION ( 'NONE',  ( 1.000000000000000000, 0.000000000000000000, 0.000000000000000000 ) ) ;
#4364 = CARTESIAN_POINT ( 'NONE',  ( 2.477266370399229256, -26.15723709312290524, 7.010186378901970272 ) ) ;
#4366 = PLANE ( 'NONE',  #9959 ) ;
#4367 = CARTESIAN_POINT ( 'NONE',  ( 76.06955384389382857, 61.76325957217472506, 3.887901781368110488 ) ) ;
#4368 = CARTESIAN_POINT ( 'NONE',  ( 23.59090747053171100, 2.763374893270500010, -4.088477763750560712 ) ) ;
#4369 = FACE_OUTER_BOUND ( 'NONE', #18702, .T. ) ;
#4370 = PLANE ( 'NONE',  #14875 ) ;
#4371 = CARTESIAN_POINT ( 'NONE',  ( -2.697268050091675118E-17, 3.729367930467589076, 2.500000000000000000 ) ) ;
#4372 = DIRECTION ( 'NONE',  ( -0.000000000000000000, -1.000000000000000000, -0.000000000000000000 ) ) ;
#4373 = CARTESIAN_POINT ( 'NONE',  ( 80.71833143474502492, 65.93084270547805659, 2.217414436011085677 ) ) ;
#4374 = CARTESIAN_POINT ( 'NONE',  ( -0.08235064813525205807, -32.58188673079869346, 6.887161170156905321 ) ) ;
#4375 = CARTESIAN_POINT ( 'NONE',  ( 27.87477497239535396, 2.606304449749688779, 1.085873857364543671 ) ) ;
#4376 = CARTESIAN_POINT ( 'NONE',  ( 2.285449761772891719, -26.22063563864136171, 7.763628509615287498 ) ) ;
#4377 = CARTESIAN_POINT ( 'NONE',  ( 21.85643539959777115, -15.24623503193425123, 0.9260495571226281530 ) ) ;
#4378 = CARTESIAN_POINT ( 'NONE',  ( -78.24659595803589696, -5.198025430032019223, -8.506940804273437351 ) ) ;
#4379 = CARTESIAN_POINT ( 'NONE',  ( -4.248748702180636272, -26.64985754041175525, 6.700000000000000178 ) ) ;
#4380 = ADVANCED_BREP_SHAPE_REPRESENTATION ( '', ( #26229, #30744 ), #8364 ) ;
#4381 = CARTESIAN_POINT ( 'NONE',  ( 74.75340671132555315, 59.31352934624568718, 3.344778443633103837 ) ) ;
#4382 = DIRECTION ( 'NONE',  ( -0.7541618601367555685, 0.000000000000000000, -0.6566885781822833223 ) ) ;
#4383 = CARTESIAN_POINT ( 'NONE',  ( 37.12953470293586378, -2.935607199016813329, -5.998835710568205748 ) ) ;
#4384 = CARTESIAN_POINT ( 'NONE',  ( 1.004186251462368507, -32.89789583248860794, 7.768425012602594215 ) ) ;
#4385 = CARTESIAN_POINT ( 'NONE',  ( 4.698894047304983168, -31.37521543190015905, 6.870737987065013819 ) ) ;
#4386 = CARTESIAN_POINT ( 'NONE',  ( -1.799548180193444757, -29.59071677051289839, 7.745317755893211142 ) ) ;
#4387 = AXIS2_PLACEMENT_3D ( 'NONE', #27264, #33883, #12014 ) ;
#4388 = CARTESIAN_POINT ( 'NONE',  ( -1.548293269840338660, -28.28698065990691646, 7.776484688137388801 ) ) ;
#4389 = EDGE_CURVE ( 'NONE', #11923, #23464, #34943, .T. ) ;
#4390 = CIRCLE ( 'NONE', #10298, 0.1000000000000028644 ) ;
#4391 = CARTESIAN_POINT ( 'NONE',  ( -4.978675913592189417, -24.55319635012989110, 6.700000000000000178 ) ) ;
#4392 = ADVANCED_FACE ( 'NONE', ( #9117 ), #40399, .F. ) ;
#4393 = EDGE_LOOP ( 'NONE', ( #6668, #17644, #20082, #37851 ) ) ;
#4394 = CARTESIAN_POINT ( 'NONE',  ( 23.23260104507673418, 3.379988935392680638, 3.619754408035347204 ) ) ;
#4395 = CARTESIAN_POINT ( 'NONE',  ( -69.92837670882107659, -0.6719362264620037939, 5.928123921495636495 ) ) ;
#4396 = CARTESIAN_POINT ( 'NONE',  ( 67.43143073044585378, 58.20127550988744503, -3.998123450764769604 ) ) ;
#4397 = ADVANCED_FACE ( 'NONE', ( #18575 ), #34270, .T. ) ;
#4398 = CARTESIAN_POINT ( 'NONE',  ( -65.15514661499977933, 34.97220226750606997, -6.888442104241536690 ) ) ;
#4399 = ORIENTED_EDGE ( 'NONE', *, *, #14362, .F. ) ;
#4400 = DIRECTION ( 'NONE',  ( -0.000000000000000000, -0.000000000000000000, 1.000000000000000000 ) ) ;
#4401 = CARTESIAN_POINT ( 'NONE',  ( -10.87867591359219155, -24.55319635012989110, 6.800000000000000711 ) ) ;
#4402 = CARTESIAN_POINT ( 'NONE',  ( 85.56005740296494366, 1.042223677629517287, -5.769124288340541362 ) ) ;
#4403 = CARTESIAN_POINT ( 'NONE',  ( 0.9110305502213149609, -32.87703034998288842, 6.988553391373221402 ) ) ;
#4404 = CARTESIAN_POINT ( 'NONE',  ( 0.3731043410590647036, -32.80849661502264780, 6.872971584836694348 ) ) ;
#4405 = FACE_OUTER_BOUND ( 'NONE', #21105, .T. ) ;
#4406 = VERTEX_POINT ( 'NONE', #21890 ) ;
#4407 = CARTESIAN_POINT ( 'NONE',  ( 23.14042469615008812, 4.038978393511998277, 3.095302447830163839 ) ) ;
#4408 = CARTESIAN_POINT ( 'NONE',  ( -1.741823553407790603, -30.20331317155271478, 7.737115613922535218 ) ) ;
#4409 = CARTESIAN_POINT ( 'NONE',  ( 80.98905497205693393, 62.76708948751929995, 3.312281065658538193 ) ) ;
#4410 = CARTESIAN_POINT ( 'NONE',  ( -0.03609309492223993637, -32.60878366570602083, 7.638132480492516585 ) ) ;
#4411 = EDGE_LOOP ( 'NONE', ( #7261, #14166, #16448, #34763 ) ) ;
#4412 = CARTESIAN_POINT ( 'NONE',  ( 78.68856915541800845, 64.27844437337117256, -3.554489553981586170 ) ) ;
#4414 = CARTESIAN_POINT ( 'NONE',  ( -1.712708766155947249, -28.79484523504865479, 7.012192614029402193 ) ) ;
#4413 = CARTESIAN_POINT ( 'NONE',  ( 25.39883144959904726, 0.6937492590089258115, 4.599813248329277293 ) ) ;
#4415 = AXIS2_PLACEMENT_3D ( 'NONE', #37432, #16225, #25098 ) ;
#4416 = CARTESIAN_POINT ( 'NONE',  ( 80.04208101465897585, 65.56312698749695755, -2.920975158733597699 ) ) ;
#4417 = CARTESIAN_POINT ( 'NONE',  ( 79.09261123048416664, 64.22416776617161815, 3.612066323963887715 ) ) ;
#4418 = AXIS2_PLACEMENT_3D ( 'NONE', #26393, #38923, #23294 ) ;
#4419 = CIRCLE ( 'NONE', #38595, 3.000000000000002665 ) ;
#4420 = CARTESIAN_POINT ( 'NONE',  ( -0.7622425899803056959, -33.94363691401473915, 7.695279973900954751 ) ) ;
#4421 = CARTESIAN_POINT ( 'NONE',  ( 78.99593020234610208, 66.21156118037409044, 1.070820504726896605 ) ) ;
#4422 = FACE_OUTER_BOUND ( 'NONE', #1071, .T. ) ;
#4423 = CARTESIAN_POINT ( 'NONE',  ( 26.56634348862415251, 2.991955253353971500, -0.5426703667890996341 ) ) ;
#4424 = CARTESIAN_POINT ( 'NONE',  ( -64.46937875527684980, 36.54399046018806985, -5.728582434991689176 ) ) ;
#4425 = VERTEX_POINT ( 'NONE', #2979 ) ;
#4426 = CARTESIAN_POINT ( 'NONE',  ( -73.66256240681488521, -1.125518199222426130, 9.676865719492857565 ) ) ;
#4427 = CARTESIAN_POINT ( 'NONE',  ( 25.40152483165711672, 0.6871398706826929992, -4.599596795371007296 ) ) ;
#4428 = DIRECTION ( 'NONE',  ( -0.000000000000000000, -0.000000000000000000, -1.000000000000000000 ) ) ;
#4429 = CARTESIAN_POINT ( 'NONE',  ( 21.58862418887968460, 7.202556094215188054, 2.923978954502209682 ) ) ;
#4430 = EDGE_LOOP ( 'NONE', ( #38174, #23858, #21182, #37088, #18242 ) ) ;
#4431 = CARTESIAN_POINT ( 'NONE',  ( 33.68489815951246413, -3.839215430596429002, -5.138831521973123984 ) ) ;
#4432 = CARTESIAN_POINT ( 'NONE',  ( 30.63322649116577523, -3.239464216780934436, -4.965866477755658259 ) ) ;
#4433 = CARTESIAN_POINT ( 'NONE',  ( -20.44874870218064444, -26.64985754041175525, 6.800000000000000711 ) ) ;
#4434 = CARTESIAN_POINT ( 'NONE',  ( -1.100220459609689394, -31.66911586629656838, 6.951256099901595320 ) ) ;
#4435 = DIRECTION ( 'NONE',  ( -0.000000000000000000, -0.000000000000000000, 1.000000000000000000 ) ) ;
#4436 = DIRECTION ( 'NONE',  ( -0.7660444431189813441, 0.6427876096865353661, -0.000000000000000000 ) ) ;
#4437 = CARTESIAN_POINT ( 'NONE',  ( -2.726063116431162392, -27.94446379774605660, 7.635761828346577573 ) ) ;
#4438 = CIRCLE ( 'NONE', #3774, 12.73502530973474300 ) ;
#4439 = CARTESIAN_POINT ( 'NONE',  ( 1.869561550574128761, -26.07402100007339740, 7.013842709614101167 ) ) ;
#4440 = CARTESIAN_POINT ( 'NONE',  ( 22.53894523562045293, 1.168954165206360862, -6.023172632562342699 ) ) ;
#4441 = ORIENTED_EDGE ( 'NONE', *, *, #2167, .F. ) ;
#4442 = ORIENTED_EDGE ( 'NONE', *, *, #21963, .F. ) ;
#4443 = CARTESIAN_POINT ( 'NONE',  ( 66.82596693864583415, 58.04328079001189877, 3.997688572870336188 ) ) ;
#4444 = AXIS2_PLACEMENT_3D ( 'NONE', #38323, #10122, #34878 ) ;
#4445 = CARTESIAN_POINT ( 'NONE',  ( 73.06729433089581960, 60.84378783247667144, -3.914122288852232678 ) ) ;
#4446 = AXIS2_PLACEMENT_3D ( 'NONE', #36574, #2429, #8353 ) ;
#4447 = EDGE_CURVE ( 'NONE', #6564, #40623, #30994, .T. ) ;
#4448 = EDGE_CURVE ( 'NONE', #18960, #24982, #40606, .T. ) ;
#4449 = CARTESIAN_POINT ( 'NONE',  ( 85.74309555164268204, 1.026708856660649705, -5.825338620068188256 ) ) ;
#4450 = EDGE_CURVE ( 'NONE', #21747, #35504, #7053, .T. ) ;
#4451 = CARTESIAN_POINT ( 'NONE',  ( -74.69100398025469190, 7.583772050443990942, -10.58965610702078841 ) ) ;
#4452 = APPLICATION_PROTOCOL_DEFINITION ( 'draft international standard', 'automotive_design', 1998, #1895 ) ;
#4453 = CARTESIAN_POINT ( 'NONE',  ( 2.992014398447776724, -26.32199281776421884, 7.771081512783698741 ) ) ;
#4454 = CARTESIAN_POINT ( 'NONE',  ( 1.102287257230225581, -26.12705058514163525, 7.773839561854632763 ) ) ;
#4455 = VERTEX_POINT ( 'NONE', #16310 ) ;
#4456 = CARTESIAN_POINT ( 'NONE',  ( 5.054787681455045423, -30.12492281798062521, 7.692469944509195301 ) ) ;
#4457 = B_SPLINE_CURVE_WITH_KNOTS ( 'NONE', 3,
 ( #18767, #461, #25155, #15885, #28857, #9290, #18984, #35056, #28444, #37902 ),
 .UNSPECIFIED., .F., .F.,
 ( 4, 3, 3, 4 ),
 ( 0.0005050348086185383559, 0.0005143352185143338934, 0.0005445898203825257468, 0.0005634294782181790886 ),
 .UNSPECIFIED. ) ;
#4458 = ORIENTED_EDGE ( 'NONE', *, *, #7264, .T. ) ;
#4459 = CARTESIAN_POINT ( 'NONE',  ( 79.88928440695104882, 63.65969051258252165, -3.720735635808768205 ) ) ;
#4460 =( BOUNDED_SURFACE ( )  B_SPLINE_SURFACE ( 3, 2, ( 
 ( #19448, #16345, #19652 ),
 ( #7088, #32223, #28918 ),
 ( #32418, #20047, #1139 ),
 ( #28714, #926, #25828 ),
 ( #6892, #19243, #4025 ),
 ( #4217, #38775, #16151 ),
 ( #9769, #13061, #16543 ),
 ( #1336, #29123, #29524 ),
 ( #526, #25423, #25623 ),
 ( #35114, #13262, #16736 ),
 ( #3626, #6695, #9971 ),
 ( #13460, #26035, #38365 ),
 ( #22352, #32021, #31811 ),
 ( #7488, #38167, #38569 ) ),
 .UNSPECIFIED., .F., .F., .T. ) 
 B_SPLINE_SURFACE_WITH_KNOTS ( ( 4, 2, 2, 2, 2, 2, 4 ),
 ( 3, 3 ),
 ( 0.000000000000000000, 0.0004485899915298040600, 0.0008971799830596081200, 0.001345769974589412126, 0.001794359966119216240, 0.002691539949178824252, 0.003588719932238432480 ),
 ( 0.000000000000000000, 1.000000000000000000 ),
 .UNSPECIFIED. ) 
 GEOMETRIC_REPRESENTATION_ITEM ( )  RATIONAL_B_SPLINE_SURFACE ( (
 ( 1.000000000000000000, 0.9000259740535757613, 1.000000000000000000),
 ( 1.000000000000000000, 0.9000175163599423156, 1.000000000000000000),
 ( 1.000000000000000000, 0.8985936556292808408, 1.000000000000000000),
 ( 1.000000000000000000, 0.8930319130234418701, 1.000000000000000000),
 ( 1.000000000000000000, 0.8888779410518012902, 1.000000000000000000),
 ( 1.000000000000000000, 0.8784198174355972721, 1.000000000000000000),
 ( 1.000000000000000000, 0.8719969190870759945, 1.000000000000000000),
 ( 1.000000000000000000, 0.8575109182637734584, 1.000000000000000000),
 ( 1.000000000000000000, 0.8493613801775528049, 1.000000000000000000),
 ( 1.000000000000000000, 0.8227151417012925627, 1.000000000000000000),
 ( 1.000000000000000000, 0.8025165990303427810, 1.000000000000000000),
 ( 1.000000000000000000, 0.7574223494978716831, 1.000000000000000000),
 ( 1.000000000000000000, 0.7332909362864591385, 1.000000000000000000),
 ( 1.000000000000000000, 0.7071067811865473507, 1.000000000000000000) ) ) 
 REPRESENTATION_ITEM ( '' )  SURFACE ( )  );
#4461 = CARTESIAN_POINT ( 'NONE',  ( 36.21386368451217663, -1.588474078234619169, 5.668731034284322234 ) ) ;
#4462 = CARTESIAN_POINT ( 'NONE',  ( 80.93996669421811418, 61.38942684853007847, 2.064111563736219956 ) ) ;
#4464 = ORIENTED_EDGE ( 'NONE', *, *, #21922, .F. ) ;
#4463 = CYLINDRICAL_SURFACE ( 'NONE', #36166, 12.38600677260393113 ) ;
#4465 = CARTESIAN_POINT ( 'NONE',  ( 27.43879754216082389, 0.9604377377020558715, 4.488885984917203587 ) ) ;
#4466 = CARTESIAN_POINT ( 'NONE',  ( 3.964423987650910419, -27.03334556693910429, 6.864651958020303368 ) ) ;
#4467 = DIRECTION ( 'NONE',  ( -0.5000000000000036637, 0.8660254037844367092, 0.000000000000000000 ) ) ;
#4468 =( GEOMETRIC_REPRESENTATION_CONTEXT ( 3 ) GLOBAL_UNCERTAINTY_ASSIGNED_CONTEXT ( ( #21763 ) ) GLOBAL_UNIT_ASSIGNED_CONTEXT ( ( #10403, #33047, #16769 ) ) REPRESENTATION_CONTEXT ( 'NONE', 'WORKASPACE' ) );
#4469 = CARTESIAN_POINT ( 'NONE',  ( 33.79079129742034127, -4.868640718861981576, -3.414904310288808365 ) ) ;
#4470 = CARTESIAN_POINT ( 'NONE',  ( 78.60787044352795760, 65.99999220767536201, -1.312857279933637766 ) ) ;
#4471 = AXIS2_PLACEMENT_3D ( 'NONE', #14092, #26274, #10602 ) ;
#4472 = LINE ( 'NONE', #25479, #11600 ) ;
#4473 = CARTESIAN_POINT ( 'NONE',  ( -72.95661835997130140, 1.053701266592789398, -9.852289288704627168 ) ) ;
#4474 = CARTESIAN_POINT ( 'NONE',  ( -32.97867591359219119, -26.64985754041175525, 6.700000000000000178 ) ) ;
#4475 = LINE ( 'NONE', #19508, #26068 ) ;
#4476 = CARTESIAN_POINT ( 'NONE',  ( 81.23287006775859709, 61.35999619221078660, 1.467306180864043075 ) ) ;
#4477 = CARTESIAN_POINT ( 'NONE',  ( -1.501549270632406063, -30.71346805803427316, 7.779495906702013741 ) ) ;
#4478 = DIRECTION ( 'NONE',  ( -0.8660254037844415942, 0.4999999999999950040, -0.000000000000000000 ) ) ;
#4479 = CARTESIAN_POINT ( 'NONE',  ( -1.576062547484236243, -30.80072589882973944, 7.697032948437506406 ) ) ;
#4480 = DIRECTION ( 'NONE',  ( 0.000000000000000000, 0.000000000000000000, -1.000000000000000000 ) ) ;
#4481 = CARTESIAN_POINT ( 'NONE',  ( 3.972279103913426201, -32.23235770788113541, 7.730015791551950954 ) ) ;
#4482 = CARTESIAN_POINT ( 'NONE',  ( -11.07867591359219794, -24.55319635012989110, 6.700000000000000178 ) ) ;
#4483 = CARTESIAN_POINT ( 'NONE',  ( 0.000000000000000000, -34.30579396504363388, 0.000000000000000000 ) ) ;
#4484 = CARTESIAN_POINT ( 'NONE',  ( 5.030284764849001000, -28.49206123220129783, 7.750000000000000888 ) ) ;
#4485 = VECTOR ( 'NONE', #38614, 1000.000000000000000 ) ;
#4486 = CARTESIAN_POINT ( 'NONE',  ( 2.704822964097302052, -32.92983929193388093, 7.387053503561887169 ) ) ;
#4487 = CARTESIAN_POINT ( 'NONE',  ( 69.15563817390996348, 58.92225492517195562, 3.988427515945577095 ) ) ;
#4488 = CARTESIAN_POINT ( 'NONE',  ( 36.19474364399976452, -2.230523885484240854, 5.855463137465835466 ) ) ;
#4489 = AXIS2_PLACEMENT_3D ( 'NONE', #14466, #8081, #5217 ) ;
#4490 = CARTESIAN_POINT ( 'NONE',  ( -22.87867591359218977, -26.64985754041175525, 6.700000000000000178 ) ) ;
#4491 = CARTESIAN_POINT ( 'NONE',  ( 88.39837738899358044, -0.9355285267052176890, 2.786041992172542336 ) ) ;
#4492 = EDGE_CURVE ( 'NONE', #20522, #9487, #10929, .T. ) ;
#4494 = CARTESIAN_POINT ( 'NONE',  ( 1.096693473209699121, -26.22395493079927320, 7.635761828346577573 ) ) ;
#4493 = CARTESIAN_POINT ( 'NONE',  ( 80.41878079785792011, 63.93588341273047604, -3.625945587094182354 ) ) ;
#4495 = CARTESIAN_POINT ( 'NONE',  ( -1.240463007521606764, -27.67219833340346113, 7.009310105710485850 ) ) ;
#4496 = CARTESIAN_POINT ( 'NONE',  ( -58.97877168559173100, 27.59157091290065367, 6.753965997777578778 ) ) ;
#4497 = ORIENTED_EDGE ( 'NONE', *, *, #31027, .T. ) ;
#4498 = CARTESIAN_POINT ( 'NONE',  ( -78.35024558020644747, 11.32744874732892804, -6.714849854229168358 ) ) ;
#4499 = CARTESIAN_POINT ( 'NONE',  ( 21.73879351235361668, 6.093659825503084271, 3.276088519256564524 ) ) ;
#4500 = VERTEX_POINT ( 'NONE', #23508 ) ;
#4501 = CARTESIAN_POINT ( 'NONE',  ( -71.90933819610624766, -21.00662979218648374, 3.919381273429904056 ) ) ;
#4502 = EDGE_LOOP ( 'NONE', ( #16669, #5606, #37962, #29719 ) ) ;
#4503 = CARTESIAN_POINT ( 'NONE',  ( 79.79930721375663438, 64.34646279424465831, -3.632888195267881315 ) ) ;
#4504 = DIRECTION ( 'NONE',  ( 1.000000000000000000, 0.000000000000000000, 0.000000000000000000 ) ) ;
#4505 = CARTESIAN_POINT ( 'NONE',  ( 80.88543547514460386, 62.41573260227067976, 3.197674131580384493 ) ) ;
#4506 = CARTESIAN_POINT ( 'NONE',  ( 24.90057636419620124, 1.281227854881117789, 4.570978506677809250 ) ) ;
#4507 = ORIENTED_EDGE ( 'NONE', *, *, #11914, .T. ) ;
#4508 = CARTESIAN_POINT ( 'NONE',  ( 5.026513843668968917, -30.27484297658092061, 6.864216812889196717 ) ) ;
#4509 = VECTOR ( 'NONE', #17851, 1000.000000000000000 ) ;
#4511 = CARTESIAN_POINT ( 'NONE',  ( 18.51265066377991531, 11.53724448280501313, 2.500000000000000000 ) ) ;
#4510 = CARTESIAN_POINT ( 'NONE',  ( 0.08557765857971742773, 0.5999999999999995337, -3.903564864120421696 ) ) ;
#4512 = CARTESIAN_POINT ( 'NONE',  ( -70.92837670882107659, -23.80776546975053165, -10.00000000000000888 ) ) ;
#4513 = CARTESIAN_POINT ( 'NONE',  ( 4.662690227536056220, -31.23869556963216709, 7.693875151218752428 ) ) ;
#4514 = EDGE_CURVE ( 'NONE', #36371, #25629, #23732, .T. ) ;
#4515 = CARTESIAN_POINT ( 'NONE',  ( 23.97627728469320019, 3.287926408277590085, -3.421875469786679336 ) ) ;
#4516 = ORIENTED_EDGE ( 'NONE', *, *, #16317, .T. ) ;
#4517 = DIRECTION ( 'NONE',  ( 0.000000000000000000, 1.000000000000000000, 0.000000000000000000 ) ) ;
#4518 = CARTESIAN_POINT ( 'NONE',  ( 22.46150523612397976, 0.3089437977474873143, 9.145744397224946809 ) ) ;
#4519 = CARTESIAN_POINT ( 'NONE',  ( 17.12093179650374708, 14.48834468576525758, -3.790908043361014279 ) ) ;
#4520 = CARTESIAN_POINT ( 'NONE',  ( -64.36865852185155745, 34.97220226750606997, 7.506047544094573531 ) ) ;
#4521 = ORIENTED_EDGE ( 'NONE', *, *, #15019, .F. ) ;
#4522 = CARTESIAN_POINT ( 'NONE',  ( 0.4771275691783791184, -32.74226228095595559, 6.880147297696982633 ) ) ;
#4523 = CARTESIAN_POINT ( 'NONE',  ( 78.83984420990493902, 66.12288285737184879, 1.382728580145343278 ) ) ;
#4524 = CARTESIAN_POINT ( 'NONE',  ( 86.43196921298398649, 0.8512835087624049946, 5.909244108978848331 ) ) ;
#4525 = CARTESIAN_POINT ( 'NONE',  ( -0.5075199548166184904, -26.98436772626320490, 7.661510568013095046 ) ) ;
#4526 = ORIENTED_EDGE ( 'NONE', *, *, #12031, .F. ) ;
#4527 = CARTESIAN_POINT ( 'NONE',  ( -1.639146693691649892, -28.93157757802832819, 6.894806418505346812 ) ) ;
#4528 = EDGE_CURVE ( 'NONE', #4832, #6790, #17102, .T. ) ;
#4529 = CARTESIAN_POINT ( 'NONE',  ( 22.43255271695741371, 5.122918363847896117, -2.447134636434162847 ) ) ;
#4530 = CARTESIAN_POINT ( 'NONE',  ( 14.75024544199591503, -5.969387982752670574, -2.508530555894281200 ) ) ;
#4531 = CARTESIAN_POINT ( 'NONE',  ( 36.99218678239946456, -2.719487527304628394, -5.979923425448357754 ) ) ;
#4532 = CARTESIAN_POINT ( 'NONE',  ( 5.098207581826219581, -29.69173459304409946, 7.754798119455333705 ) ) ;
#4533 = DIRECTION ( 'NONE',  ( 0.7660444431189771253, 0.6427876096865405842, -0.000000000000000000 ) ) ;
#4534 = CARTESIAN_POINT ( 'NONE',  ( 29.68218759030339271, -3.793136067405761924, -4.440320134392340634 ) ) ;
#4535 = CARTESIAN_POINT ( 'NONE',  ( 3.870387127636869540, -26.95245864641162825, 7.643333865083954848 ) ) ;
#4536 = DIRECTION ( 'NONE',  ( 0.000000000000000000, 0.000000000000000000, 1.000000000000000000 ) ) ;
#4537 = CARTESIAN_POINT ( 'NONE',  ( -1.153862800135780464, -27.72243446737795125, 6.882085323592686876 ) ) ;
#4538 = AXIS2_PLACEMENT_3D ( 'NONE', #3971, #16292, #23092 ) ;
#4539 = EDGE_CURVE ( 'NONE', #32235, #8986, #22906, .T. ) ;
#4540 = VERTEX_POINT ( 'NONE', #29675 ) ;
#4541 = VERTEX_POINT ( 'NONE', #1487 ) ;
#4542 = CARTESIAN_POINT ( 'NONE',  ( 35.22074791301828611, -1.047776788863644226, 5.411314349319545691 ) ) ;
#4543 = LINE ( 'NONE', #17667, #14581 ) ;
#4544 = CARTESIAN_POINT ( 'NONE',  ( -75.45330471031414277, 33.71485196875532608, 9.800414904976365804 ) ) ;
#4545 = FACE_OUTER_BOUND ( 'NONE', #28914, .T. ) ;
#4546 = ORIENTED_EDGE ( 'NONE', *, *, #33575, .F. ) ;
#4547 = DIRECTION ( 'NONE',  ( -0.000000000000000000, -0.000000000000000000, -1.000000000000000000 ) ) ;
#4548 = CARTESIAN_POINT ( 'NONE',  ( -55.16208421294561504, 31.22611435454061990, -1.446432346866528995 ) ) ;
#4550 = CARTESIAN_POINT ( 'NONE',  ( 21.90912465241696694, 3.662607847362923774, -2.128491611114075699 ) ) ;
#4549 = CARTESIAN_POINT ( 'NONE',  ( 4.772714607425114330, -27.89337953414514359, 6.865554069792297653 ) ) ;
#4551 = ORIENTED_EDGE ( 'NONE', *, *, #18980, .T. ) ;
#4552 = CARTESIAN_POINT ( 'NONE',  ( 23.96426883893546389, 3.278871655312407984, 3.444941816143999969 ) ) ;
#4553 = CARTESIAN_POINT ( 'NONE',  ( 82.13040900219759521, 64.82864533757665981, -1.905332024691357429 ) ) ;
#4554 = EDGE_CURVE ( 'NONE', #16283, #19590, #26400, .T. ) ;
#4555 = CARTESIAN_POINT ( 'NONE',  ( -1.226243465414398548, -31.30048392015029890, 7.680992449362119778 ) ) ;
#4556 = ORIENTED_EDGE ( 'NONE', *, *, #12160, .F. ) ;
#4558 = CARTESIAN_POINT ( 'NONE',  ( 4.386463650923984048, -27.33967598338160343, 7.778495531946297170 ) ) ;
#4557 = CARTESIAN_POINT ( 'NONE',  ( 2.497040581740529674, -26.16180034221845219, 6.955226052476382925 ) ) ;
#4559 = CARTESIAN_POINT ( 'NONE',  ( -18.24874870218063450, -26.64985754041175525, 6.700000000000000178 ) ) ;
#4560 = CARTESIAN_POINT ( 'NONE',  ( 76.30453859000765249, 59.72919098693703432, 3.074209570828593918 ) ) ;
#4561 = ORIENTED_EDGE ( 'NONE', *, *, #39880, .T. ) ;
#4562 = CARTESIAN_POINT ( 'NONE',  ( 23.43636678123177219, 2.538610166689087677, -4.312835133894656003 ) ) ;
#4563 = DIRECTION ( 'NONE',  ( 1.000000000000000000, 0.000000000000000000, 0.000000000000000000 ) ) ;
#4564 = CARTESIAN_POINT ( 'NONE',  ( 16.14043970921329674, 15.25505324876322888, -0.6630684997063907016 ) ) ;
#4565 = DIRECTION ( 'NONE',  ( -0.000000000000000000, -0.000000000000000000, -1.000000000000000000 ) ) ;
#4566 = CARTESIAN_POINT ( 'NONE',  ( -70.92837670882107659, -60.53509472482660669, 7.538952224936807056 ) ) ;
#4567 = CARTESIAN_POINT ( 'NONE',  ( -16.97867591359219475, -24.55319635012989110, 6.700000000000000178 ) ) ;
#4568 = CARTESIAN_POINT ( 'NONE',  ( 81.16843721835843439, 61.30356250071481128, 1.032522165606394315 ) ) ;
#4569 = CARTESIAN_POINT ( 'NONE',  ( 85.17359253740836778, 2.686702876117401662, 1.784494502703901864 ) ) ;
#4570 = CARTESIAN_POINT ( 'NONE',  ( 33.61282307965942806, -4.196488527906213406, -4.700131347630155609 ) ) ;
#4571 = ADVANCED_FACE ( 'NONE', ( #23304 ), #4697, .T. ) ;
#4572 = EDGE_CURVE ( 'NONE', #28407, #3811, #25791, .T. ) ;
#4573 = CARTESIAN_POINT ( 'NONE',  ( 4.639185200793720654, -27.65646266981928036, 7.139344958878412584 ) ) ;
#4574 = CARTESIAN_POINT ( 'NONE',  ( -72.42837670882107659, -47.11702805680359063, 9.886859966642603581 ) ) ;
#4575 = ADVANCED_FACE ( 'NONE', ( #35474 ), #16905, .F. ) ;
#4576 = DIRECTION ( 'NONE',  ( -1.000000000000000000, 0.000000000000000000, 0.000000000000000000 ) ) ;
#4577 = CARTESIAN_POINT ( 'NONE',  ( 35.94200923520244828, 151.3264224549853907, 1.000000000000000000 ) ) ;
#4578 = CARTESIAN_POINT ( 'NONE',  ( 0.1132627511917800867, -26.45046942404118440, 6.989977667959447416 ) ) ;
#4579 = CARTESIAN_POINT ( 'NONE',  ( 35.33513638873442630, -3.237442486773212558, -5.721300635602096563 ) ) ;
#4580 = CARTESIAN_POINT ( 'NONE',  ( 0.9946364188725682620, -32.89587624457358572, 7.759451378593097637 ) ) ;
#4581 = CARTESIAN_POINT ( 'NONE',  ( 1.700390093233090871, -29.56993018339339940, 7.750000000000000888 ) ) ;
#4582 = CARTESIAN_POINT ( 'NONE',  ( -63.68920958294118151, 44.29446941693485229, -1.843112653903773657 ) ) ;
#4583 = CARTESIAN_POINT ( 'NONE',  ( 5.751251297819365504, -25.49307895267003587, 6.700000000000000178 ) ) ;
#4584 = EDGE_CURVE ( 'NONE', #2595, #24834, #1171, .T. ) ;
#4585 = VERTEX_POINT ( 'NONE', #33182 ) ;
#4586 = CARTESIAN_POINT ( 'NONE',  ( 36.29298905792148133, -2.016294748008292892, 5.862889200204672413 ) ) ;
#4587 = CARTESIAN_POINT ( 'NONE',  ( 1.700390093233090871, -29.56993018339339940, 7.800000000000000711 ) ) ;
#4588 = CARTESIAN_POINT ( 'NONE',  ( 67.14253272251396254, 58.08395421452478757, -3.998868826385352460 ) ) ;
#4589 = CARTESIAN_POINT ( 'NONE',  ( 3.070482080713194950, -26.34923958263044597, 6.921725064902947366 ) ) ;
#4590 = ORIENTED_EDGE ( 'NONE', *, *, #24841, .T. ) ;
#4591 = CARTESIAN_POINT ( 'NONE',  ( -15.07867591359219439, -26.64985754041175525, 6.700000000000000178 ) ) ;
#4592 = DIRECTION ( 'NONE',  ( 0.000000000000000000, 1.000000000000000000, 0.000000000000000000 ) ) ;
#4593 = CARTESIAN_POINT ( 'NONE',  ( 85.65758405518126040, 0.8774719100965696628, -5.855775047906961461 ) ) ;
#4594 = CARTESIAN_POINT ( 'NONE',  ( 2.310642412388812961, -32.91472262586214015, 7.643333865083956624 ) ) ;
#4595 = PLANE ( 'NONE',  #39140 ) ;
#4596 = CARTESIAN_POINT ( 'NONE',  ( 35.94200923520244828, 151.3264224549853907, 1.000000000000000000 ) ) ;
#4597 = EDGE_LOOP ( 'NONE', ( #20473, #17904, #34990, #38022, #18712 ) ) ;
#4598 = CARTESIAN_POINT ( 'NONE',  ( 24.40258831255338734, 3.162078629162225152, 3.277950946408194621 ) ) ;
#4599 = CARTESIAN_POINT ( 'NONE',  ( 0.6783104270758654186, -48.60743831809499227, -2.500000000000000000 ) ) ;
#4600 = EDGE_CURVE ( 'NONE', #19379, #38217, #10595, .T. ) ;
#4601 = CARTESIAN_POINT ( 'NONE',  ( 80.95271419388603817, 62.75148163162413795, 3.324099845469156378 ) ) ;
#4602 = CARTESIAN_POINT ( 'NONE',  ( -0.2487487021806331078, -26.64985754041175525, 6.800000000000000711 ) ) ;
#4603 = ORIENTED_EDGE ( 'NONE', *, *, #28455, .F. ) ;
#4604 = CARTESIAN_POINT ( 'NONE',  ( 79.34756916856697728, 63.37933396398980079, -3.765547211956733697 ) ) ;
#4606 = CARTESIAN_POINT ( 'NONE',  ( 14.69558838330761930, -4.461995682952461628, -2.500000000000009770 ) ) ;
#4605 = CARTESIAN_POINT ( 'NONE',  ( 21.73501309383516045, 0.2561466533226999243, 9.001404038369074101 ) ) ;
#4607 = CARTESIAN_POINT ( 'NONE',  ( 81.34875679480646227, 63.64560584541077759, -3.283621700554755218 ) ) ;
#4608 = CARTESIAN_POINT ( 'NONE',  ( 78.45565513354563336, 64.70068626995113448, 3.258123098320686140 ) ) ;
#4609 = EDGE_CURVE ( 'NONE', #18695, #20708, #17913, .T. ) ;
#4610 = AXIS2_PLACEMENT_3D ( 'NONE', #5051, #32862, #39212 ) ;
#4611 = CARTESIAN_POINT ( 'NONE',  ( -1.629504578382812818, -30.64779913458552230, 7.750000000000000888 ) ) ;
#4612 = ADVANCED_FACE ( 'NONE', ( #33599 ), #23695, .F. ) ;
#4613 = CARTESIAN_POINT ( 'NONE',  ( 81.16957891225079891, 61.30398062001319914, 1.002944004955704127 ) ) ;
#4614 = CARTESIAN_POINT ( 'NONE',  ( 59.69572451838116933, -0.8894979772356270686, 5.999999999999999112 ) ) ;
#4615 = CARTESIAN_POINT ( 'NONE',  ( 30.13572739226143327, -4.670734905539763560, 0.4584422186006349986 ) ) ;
#4616 = CARTESIAN_POINT ( 'NONE',  ( -64.78745217040265914, 34.77601383833022197, -6.355070236020407215 ) ) ;
#4617 = EDGE_LOOP ( 'NONE', ( #34756, #10277, #8001, #23565 ) ) ;
#4618 = CARTESIAN_POINT ( 'NONE',  ( -74.01468305983279095, -3.815910838439570352, 9.516541306992865046 ) ) ;
#4619 = CARTESIAN_POINT ( 'NONE',  ( 21.98018615774344653, 0.2297809094950876430, -7.706785321375619446 ) ) ;
#4620 = ADVANCED_FACE ( 'NONE', ( #8851 ), #23886, .F. ) ;
#4621 = LINE ( 'NONE', #17344, #27432 ) ;
#4622 = ORIENTED_EDGE ( 'NONE', *, *, #14827, .T. ) ;
#4623 = CARTESIAN_POINT ( 'NONE',  ( -14.97867591359219119, -26.64985754041175525, 6.700000000000000178 ) ) ;
#4624 = CIRCLE ( 'NONE', #20378, 6.138794830819693793 ) ;
#4625 = ORIENTED_EDGE ( 'NONE', *, *, #37239, .F. ) ;
#4626 = CARTESIAN_POINT ( 'NONE',  ( 21.73769930489046232, 4.234352968378803261, -2.806692186376322340 ) ) ;
#4627 = LINE ( 'NONE', #39183, #2992 ) ;
#4628 = LINE ( 'NONE', #20452, #28830 ) ;
#4629 = CARTESIAN_POINT ( 'NONE',  ( 5.112556415631599904, -30.34910987273946148, 7.006908160621412307 ) ) ;
#4630 = CARTESIAN_POINT ( 'NONE',  ( -72.12732577070732987, -48.03925814481806356, 5.880655408758564739 ) ) ;
#4631 = CARTESIAN_POINT ( 'NONE',  ( 2.679230591341950962, -32.82598166935948569, 6.903372536218455480 ) ) ;
#4632 = DIRECTION ( 'NONE',  ( 0.000000000000000000, 0.000000000000000000, 1.000000000000000000 ) ) ;
#4633 = CARTESIAN_POINT ( 'NONE',  ( 4.668948836787977896, -27.91232378075620701, 6.894806418505348589 ) ) ;
#4634 = ORIENTED_EDGE ( 'NONE', *, *, #38564, .T. ) ;
#4635 = CARTESIAN_POINT ( 'NONE',  ( 66.43088956075774831, 57.76580747938982796, 4.000000000000006217 ) ) ;
#4636 = CARTESIAN_POINT ( 'NONE',  ( 72.54144496250529528, 58.88102433069186503, -3.699617110138616383 ) ) ;
#4637 = ORIENTED_EDGE ( 'NONE', *, *, #8585, .T. ) ;
#4638 = CARTESIAN_POINT ( 'NONE',  ( 87.11462257552980759, -1.147413441766115039, -5.140310012396687611 ) ) ;
#4639 = CARTESIAN_POINT ( 'NONE',  ( 0.1824275742476695050, -26.52759723137196701, 6.929923840112064859 ) ) ;
#4640 = CARTESIAN_POINT ( 'NONE',  ( 2.876659513533784018, -26.27350604724992067, 7.743886751744251562 ) ) ;
#4641 = PRODUCT_CONTEXT ( 'NONE', #11045, 'mechanical' ) ;
#4642 = CARTESIAN_POINT ( 'NONE',  ( 2.287972448046889706, -32.91877281575333569, 7.769368695748486431 ) ) ;
#4643 = CARTESIAN_POINT ( 'NONE',  ( -2.772340841568255776, -28.07161080258395103, 7.754798119455333705 ) ) ;
#4644 = CARTESIAN_POINT ( 'NONE',  ( 5.141684319425215755, -30.20828278875847062, 6.894806418505347700 ) ) ;
#4645 = ADVANCED_FACE ( 'NONE', ( #8234 ), #38801, .T. ) ;
#4646 = VECTOR ( 'NONE', #21031, 1000.000000000000000 ) ;
#4647 = EDGE_LOOP ( 'NONE', ( #28907, #11112, #23141, #1339, #24209 ) ) ;
#4648 = CARTESIAN_POINT ( 'NONE',  ( 78.51047153333161077, 65.93088068117907596, -1.448968528258141486 ) ) ;
#4649 = CARTESIAN_POINT ( 'NONE',  ( 12.97258467943525062, 9.268118853444669014, -3.480631448259292604 ) ) ;
#4650 = CARTESIAN_POINT ( 'NONE',  ( 78.83205648568262802, 65.58035453618819588, 2.615973384260660950 ) ) ;
#4651 = FACE_OUTER_BOUND ( 'NONE', #11592, .T. ) ;
#4652 = CYLINDRICAL_SURFACE ( 'NONE', #37650, 3.399999999999999911 ) ;
#4653 = CYLINDRICAL_SURFACE ( 'NONE', #12459, 1.000000000000003997 ) ;
#4654 = DIRECTION ( 'NONE',  ( 1.000000000000000000, 0.000000000000000000, 0.000000000000000000 ) ) ;
#4655 = CARTESIAN_POINT ( 'NONE',  ( 21.85643539959776049, -12.91308397612913161, -3.835380774090566103 ) ) ;
#4656 = CARTESIAN_POINT ( 'NONE',  ( 78.31607304441834572, 65.79307132853784879, -1.652946521066924745 ) ) ;
#4657 = VECTOR ( 'NONE', #6665, 1000.000000000000114 ) ;
#4658 = ADVANCED_FACE ( 'NONE', ( #29432 ), #26351, .F. ) ;
#4659 = CARTESIAN_POINT ( 'NONE',  ( 14.72840846699002526, -4.935183498936103419, 2.501324498462070167 ) ) ;
#4660 = EDGE_CURVE ( 'NONE', #5702, #13186, #26402, .T. ) ;
#4661 = CARTESIAN_POINT ( 'NONE',  ( -74.32433723247588375, -2.242446129776642927, -10.69717072308378469 ) ) ;
#4662 = CARTESIAN_POINT ( 'NONE',  ( 1.490503839106549266, -32.96344572930279071, 6.959317978105165281 ) ) ;
#4663 = CARTESIAN_POINT ( 'NONE',  ( 2.493137266801881413, -26.26364043220722877, 6.929923840112065747 ) ) ;
#4664 = CARTESIAN_POINT ( 'NONE',  ( 80.10206815703588745, 64.89240018571257451, 3.380792992375215356 ) ) ;
#4665 = CARTESIAN_POINT ( 'NONE',  ( -1.529814622690701009, -30.63098279475522290, 7.768425012602592439 ) ) ;
#4666 = CARTESIAN_POINT ( 'NONE',  ( 3.946934465176325624, -27.01784786054519216, 7.782034975670478083 ) ) ;
#4667 = CARTESIAN_POINT ( 'NONE',  ( 1.700390093233090871, -29.56993018339339940, 7.750000000000000888 ) ) ;
#4668 = DIRECTION ( 'NONE',  ( -0.000000000000000000, -1.000000000000000000, -0.000000000000000000 ) ) ;
#4669 = CARTESIAN_POINT ( 'NONE',  ( 0.6026438237153681765, -26.24651957209255926, 6.863784140767622333 ) ) ;
#4670 = CARTESIAN_POINT ( 'NONE',  ( 4.483263867588910934, -27.44727572642202063, 6.887547729233693516 ) ) ;
#4671 = AXIS2_PLACEMENT_3D ( 'NONE', #17550, #39380, #21487 ) ;
#4672 = CARTESIAN_POINT ( 'NONE',  ( 1.123053586962270423, -33.02198501472603454, 7.665454363767879364 ) ) ;
#4673 = CARTESIAN_POINT ( 'NONE',  ( 4.271731398765316712, -31.79438740411119468, 6.892063359921928978 ) ) ;
#4674 = CARTESIAN_POINT ( 'NONE',  ( -1.583399485992929234, -33.56764205940365997, 7.695279973900954751 ) ) ;
#4675 = CARTESIAN_POINT ( 'NONE',  ( 67.94738262351316394, 58.59965392607728063, 3.985705108533788010 ) ) ;
#4676 = CARTESIAN_POINT ( 'NONE',  ( 33.62922731160094969, -1.227221384262835890, 5.455052266548129580 ) ) ;
#4677 = EDGE_LOOP ( 'NONE', ( #22942, #38986, #34738, #33814 ) ) ;
#4678 = CARTESIAN_POINT ( 'NONE',  ( -64.08758708074093136, 41.04287353446839859, -3.000000000000000000 ) ) ;
#4679 = CARTESIAN_POINT ( 'NONE',  ( 86.01579553793663990, 1.740700492558412193, -4.743980989581940477 ) ) ;
#4681 = DIRECTION ( 'NONE',  ( 0.8888117386314196011, 0.4582725098355703852, 0.000000000000000000 ) ) ;
#4680 = CARTESIAN_POINT ( 'NONE',  ( 81.20006484400859392, 61.61449114502521951, -2.147349935851008862 ) ) ;
#4682 = CARTESIAN_POINT ( 'NONE',  ( -1.255528973988210284, -27.69575237218189301, 6.875780273367530171 ) ) ;
#4683 = CARTESIAN_POINT ( 'NONE',  ( 2.415520790285624386, -26.14641386366805520, 7.766640943994648438 ) ) ;
#4684 = VERTEX_POINT ( 'NONE', #836 ) ;
#4685 = DIRECTION ( 'NONE',  ( 0.000000000000000000, 1.000000000000000000, 0.000000000000000000 ) ) ;
#4686 = CARTESIAN_POINT ( 'NONE',  ( -10.44874870218064089, -26.64985754041175525, 6.700000000000000178 ) ) ;
#4687 = ORIENTED_EDGE ( 'NONE', *, *, #5684, .T. ) ;
#4688 = CARTESIAN_POINT ( 'NONE',  ( -71.64402667994158946, -21.49031309831630665, 5.969620261456463517 ) ) ;
#4689 = ORIENTED_EDGE ( 'NONE', *, *, #21764, .F. ) ;
#4690 = ORIENTED_EDGE ( 'NONE', *, *, #30724, .T. ) ;
#4691 = CARTESIAN_POINT ( 'NONE',  ( 80.69932603693776230, 62.65430898200600751, -3.392181771880276919 ) ) ;
#4692 = CARTESIAN_POINT ( 'NONE',  ( -44.23414840393349579, -23.60493063168010153, 6.800000000000000711 ) ) ;
#4693 = PRODUCT_RELATED_PRODUCT_CATEGORY ( 'part', '', ( #101 ) ) ;
#4694 = CARTESIAN_POINT ( 'NONE',  ( 80.50045704793726031, 63.23530725187647050, 3.614403801066808697 ) ) ;
#4695 = CARTESIAN_POINT ( 'NONE',  ( 26.03758185223221489, 1.465628984450591643, 4.326634389998879726 ) ) ;
#4696 = CARTESIAN_POINT ( 'NONE',  ( 4.771399860080459909, -27.90595840320830234, 7.776484688137385248 ) ) ;
#4697 = TOROIDAL_SURFACE ( 'NONE', #22468, 98.38357402481355507, 3.000000000000000000 ) ;
#4698 = CARTESIAN_POINT ( 'NONE',  ( 0.02581832829155081277, -32.52895329133826863, 7.730758795053807475 ) ) ;
#4700 = DIRECTION ( 'NONE',  ( -1.000000000000000000, 0.000000000000000000, 0.000000000000000000 ) ) ;
#4699 = CARTESIAN_POINT ( 'NONE',  ( 0.1326080060424829343, 0.5999999999999995337, -3.927320754166761851 ) ) ;
#4701 = CARTESIAN_POINT ( 'NONE',  ( -1.242662853510920540, -27.86744983030224176, 7.769368695748485543 ) ) ;
#4702 = CARTESIAN_POINT ( 'NONE',  ( -81.07947155388369254, 30.81399289130168384, -46.17089178453873188 ) ) ;
#4703 = CARTESIAN_POINT ( 'NONE',  ( 22.95716255745577428, 3.903089801653534696, -3.484934174897956094 ) ) ;
#4704 = ORIENTED_EDGE ( 'NONE', *, *, #20307, .T. ) ;
#4705 = CARTESIAN_POINT ( 'NONE',  ( 5.121754656661359206, -30.23353345891325006, 7.785593909369613819 ) ) ;
#4706 = EDGE_LOOP ( 'NONE', ( #30056, #10455, #15653, #11096, #39480 ) ) ;
#4707 = ADVANCED_FACE ( 'NONE', ( #25942 ), #1246, .F. ) ;
#4708 = CARTESIAN_POINT ( 'NONE',  ( 23.92272977471906614, 4.146422156947720872, -1.204255912843045229 ) ) ;
#4709 = EDGE_CURVE ( 'NONE', #37682, #713, #11903, .T. ) ;
#4710 = VERTEX_POINT ( 'NONE', #4527 ) ;
#4711 = CARTESIAN_POINT ( 'NONE',  ( 1.128064129311358244, -33.02281926226938680, 7.701614758090453705 ) ) ;
#4712 = CARTESIAN_POINT ( 'NONE',  ( 81.42106526723539162, 61.53660244640637700, 1.679744683813965578 ) ) ;
#4713 = CARTESIAN_POINT ( 'NONE',  ( 85.61248512101352048, 1.464218027013357570, -5.526712519226341769 ) ) ;
#4714 = CARTESIAN_POINT ( 'NONE',  ( 4.487153213455422396, -27.45239593059636363, 7.013842709614101167 ) ) ;
#4715 = ORIENTED_EDGE ( 'NONE', *, *, #3010, .T. ) ;
#4716 = FACE_OUTER_BOUND ( 'NONE', #4647, .T. ) ;
#4717 = LINE ( 'NONE', #32928, #20366 ) ;
#4718 = CARTESIAN_POINT ( 'NONE',  ( 33.12062221538703000, -3.232445517116538714, -5.375672140621767348 ) ) ;
#4719 = CARTESIAN_POINT ( 'NONE',  ( 29.09977985558236924, 0.3540121042850735145, -4.748122445935673674 ) ) ;
#4720 = DIRECTION ( 'NONE',  ( 0.9880385148181951571, 0.000000000000000000, -0.1542073060391599970 ) ) ;
#4721 = CARTESIAN_POINT ( 'NONE',  ( 84.57639812724936235, 2.428913470196615521, -3.745062422066182339 ) ) ;
#4722 = CARTESIAN_POINT ( 'NONE',  ( 30.45118816949839768, -3.644433509500874635, -4.694111347297837078 ) ) ;
#4723 = VERTEX_POINT ( 'NONE', #1441 ) ;
#4724 = FACE_OUTER_BOUND ( 'NONE', #13639, .T. ) ;
#4725 = CARTESIAN_POINT ( 'NONE',  ( 3.425778817581328628, -32.49961169336884126, 7.661510568013098599 ) ) ;
#4726 = AXIS2_PLACEMENT_3D ( 'NONE', #2234, #14755, #7975 ) ;
#4727 = CARTESIAN_POINT ( 'NONE',  ( -1.206564353649571819, -27.80649297760044902, 6.874555630061442102 ) ) ;
#4728 = ORIENTED_EDGE ( 'NONE', *, *, #1875, .F. ) ;
#4729 = ORIENTED_EDGE ( 'NONE', *, *, #29201, .T. ) ;
#4730 = CARTESIAN_POINT ( 'NONE',  ( 33.68516129456243391, -3.840378280999563465, 5.137618048204199539 ) ) ;
#4731 = CARTESIAN_POINT ( 'NONE',  ( -1.609939828903696135, -30.70650248539039850, 6.870737987065014707 ) ) ;
#4732 = EDGE_CURVE ( 'NONE', #39711, #34290, #29151, .T. ) ;
#4733 = CARTESIAN_POINT ( 'NONE',  ( -16.24874870218063450, -26.64985754041175525, 6.800000000000000711 ) ) ;
#4734 = CARTESIAN_POINT ( 'NONE',  ( 87.82094399217496061, -2.385319725885814535, 1.832678672200965364 ) ) ;
#4735 = ORIENTED_EDGE ( 'NONE', *, *, #20307, .F. ) ;
#4736 = EDGE_LOOP ( 'NONE', ( #13583, #10954, #32616, #28436 ) ) ;
#4737 = CARTESIAN_POINT ( 'NONE',  ( 4.922922413687589760, -28.48582435662824963, 6.870716933885665512 ) ) ;
#4738 = ORIENTED_EDGE ( 'NONE', *, *, #14908, .F. ) ;
#4739 = CARTESIAN_POINT ( 'NONE',  ( -57.16504416091206053, 33.41445838748276742, -3.999999999999999112 ) ) ;
#4740 = FILL_AREA_STYLE ('',( #20371 ) ) ;
#4741 = ORIENTED_EDGE ( 'NONE', *, *, #37378, .T. ) ;
#4742 = CARTESIAN_POINT ( 'NONE',  ( 22.27435398669647881, 4.892900451708169562, 3.295348648465727948 ) ) ;
#4743 = CARTESIAN_POINT ( 'NONE',  ( 81.16905975791091521, 61.30379048835199995, -1.022614849746412924 ) ) ;
#4744 = EDGE_CURVE ( 'NONE', #21196, #22883, #2756, .T. ) ;
#4745 = CARTESIAN_POINT ( 'NONE',  ( -1.225953191357326499, -31.30097466021442187, 7.693875151218753317 ) ) ;
#4746 = ORIENTED_EDGE ( 'NONE', *, *, #11028, .T. ) ;
#4748 = DIRECTION ( 'NONE',  ( 0.000000000000000000, 0.000000000000000000, -1.000000000000000000 ) ) ;
#4747 = CARTESIAN_POINT ( 'NONE',  ( 0.01878240296280925953, -0.5999999999999994227, -3.829296454260694205 ) ) ;
#4749 = CARTESIAN_POINT ( 'NONE',  ( -66.45851120290885206, -60.53509472482660669, -7.806255641895631925E-15 ) ) ;
#4750 = CARTESIAN_POINT ( 'NONE',  ( 74.93610893867889899, 61.23939191379614755, 3.912919437578919357 ) ) ;
#4751 = CARTESIAN_POINT ( 'NONE',  ( 22.47393122894036210, 2.796275671460458412, -4.701534300632203234 ) ) ;
#4752 = CARTESIAN_POINT ( 'NONE',  ( -64.08758708074093136, 37.05642372032221488, 4.717683440829013364 ) ) ;
#4753 = DIRECTION ( 'NONE',  ( 1.000000000000000000, 0.000000000000000000, 0.000000000000000000 ) ) ;
#4755 = EDGE_CURVE ( 'NONE', #19731, #33546, #12962, .T. ) ;
#4754 = FACE_OUTER_BOUND ( 'NONE', #38298, .T. ) ;
#4756 = CARTESIAN_POINT ( 'NONE',  ( 0.1825688514436868137, -0.5999999999999994227, -3.931742364907163001 ) ) ;
#4757 = CARTESIAN_POINT ( 'NONE',  ( 1.664433243520564654, -26.07011488755866679, 7.685194954629195330 ) ) ;
#4758 = CARTESIAN_POINT ( 'NONE',  ( 81.07711124303949646, 65.42186869171266039, 2.645340681430091490 ) ) ;
#4759 = CARTESIAN_POINT ( 'NONE',  ( 87.55151927672237377, 0.01570269930849589254, 4.249584817138070569 ) ) ;
#4760 = CARTESIAN_POINT ( 'NONE',  ( 29.34248944929254677, 1.775380825033272991, -3.063368523016994249 ) ) ;
#4761 = CARTESIAN_POINT ( 'NONE',  ( -22.44874870218064089, -26.64985754041175525, 6.700000000000000178 ) ) ;
#4762 = CARTESIAN_POINT ( 'NONE',  ( 3.449177982490851502, -26.65415568621681075, 6.887041543973315250 ) ) ;
#4763 = AXIS2_PLACEMENT_3D ( 'NONE', #31582, #10540, #3599 ) ;
#4764 = CARTESIAN_POINT ( 'NONE',  ( 4.672854012516526545, -31.41284476466181630, 7.766640943994350010 ) ) ;
#4765 = CARTESIAN_POINT ( 'NONE',  ( 23.84965713394175424, -3.142048526390663010, 3.808973460114609466 ) ) ;
#4766 = CARTESIAN_POINT ( 'NONE',  ( -7.078675913592194391, -26.64985754041175525, 6.700000000000000178 ) ) ;
#4767 = CARTESIAN_POINT ( 'NONE',  ( 33.67567688289796024, -3.265297112828876802, -5.462301845497175457 ) ) ;
#4768 = FACE_OUTER_BOUND ( 'NONE', #14978, .T. ) ;
#4769 = CARTESIAN_POINT ( 'NONE',  ( -63.99293516169446150, 35.89893413629672381, 12.49999999999999645 ) ) ;
#4770 = DIRECTION ( 'NONE',  ( 0.000000000000000000, 0.000000000000000000, 1.000000000000000000 ) ) ;
#4771 = LINE ( 'NONE', #36081, #4012 ) ;
#4772 = CARTESIAN_POINT ( 'NONE',  ( 4.313182060182604083, -31.74555727507705072, 7.756377446753161209 ) ) ;
#4773 = EDGE_LOOP ( 'NONE', ( #10996, #15436, #30781, #20986 ) ) ;
#4774 = CARTESIAN_POINT ( 'NONE',  ( 33.82075086788260876, -0.7236657158041540638, 5.383591898491746797 ) ) ;
#4775 = CARTESIAN_POINT ( 'NONE',  ( -70.14355411941724583, -0.1632709328201389365, 5.960493810635122180 ) ) ;
#4776 = EDGE_CURVE ( 'NONE', #12173, #26219, #17717, .T. ) ;
#4777 = CARTESIAN_POINT ( 'NONE',  ( 67.48690106321139126, 58.04989387035797677, -3.996173465816880377 ) ) ;
#4778 = AXIS2_PLACEMENT_3D ( 'NONE', #16988, #35159, #32068 ) ;
#4779 = CARTESIAN_POINT ( 'NONE',  ( 3.076514354118595751, -26.35181238915100010, 6.961115707816235343 ) ) ;
#4780 = VERTEX_POINT ( 'NONE', #9078 ) ;
#4781 = DIRECTION ( 'NONE',  ( -0.000000000000000000, 0.000000000000000000, 1.000000000000000000 ) ) ;
#4782 = DIRECTION ( 'NONE',  ( -0.000000000000000000, -0.000000000000000000, -1.000000000000000000 ) ) ;
#4783 = CARTESIAN_POINT ( 'NONE',  ( 78.60788762842503274, 66.00000440856842943, 1.312824883943342513 ) ) ;
#4784 = CARTESIAN_POINT ( 'NONE',  ( 0.9102967148584886203, -32.87685623351212882, 6.920489980334477487 ) ) ;
#4785 = CARTESIAN_POINT ( 'NONE',  ( -1.453630635037690411, -28.30022421521090337, 6.864276522220859711 ) ) ;
#4786 = EDGE_CURVE ( 'NONE', #20345, #33155, #18498, .T. ) ;
#4787 = CARTESIAN_POINT ( 'NONE',  ( 0.3915459956710288236, -32.81601029087934052, 6.865706122441729065 ) ) ;
#4788 = AXIS2_PLACEMENT_3D ( 'NONE', #10745, #7672, #20226 ) ;
#4789 = DIRECTION ( 'NONE',  ( -1.000000000000000000, 0.000000000000000000, 0.000000000000000000 ) ) ;
#4790 = EDGE_LOOP ( 'NONE', ( #8217, #38242, #16637, #40483 ) ) ;
#4791 = ADVANCED_FACE ( 'NONE', ( #21239 ), #33811, .F. ) ;
#4792 = CARTESIAN_POINT ( 'NONE',  ( 23.14123425308138593, 4.046733741470082357, 3.080193756421565787 ) ) ;
#4793 = EDGE_CURVE ( 'NONE', #34797, #22022, #12931, .T. ) ;
#4794 = CARTESIAN_POINT ( 'NONE',  ( 81.06670574969137988, 62.21556664890213284, 2.940771700540082634 ) ) ;
#4795 = CARTESIAN_POINT ( 'NONE',  ( -0.03280221984780769956, -32.61066108333789515, 7.643192810543824933 ) ) ;
#4796 = ORIENTED_EDGE ( 'NONE', *, *, #32659, .F. ) ;
#4797 = CARTESIAN_POINT ( 'NONE',  ( 79.06939945841564565, 62.09164075111537073, -3.616565173810662337 ) ) ;
#4798 =( BOUNDED_CURVE ( )  B_SPLINE_CURVE ( 3, ( #12143, #18525, #8648, #33794 ),
 .UNSPECIFIED., .F., .T. ) 
 B_SPLINE_CURVE_WITH_KNOTS ( ( 4, 4 ),
 ( 4.564251139902668619, 4.712388980384691450 ),
 .UNSPECIFIED. ) 
 CURVE ( )  GEOMETRIC_REPRESENTATION_ITEM ( )  RATIONAL_B_SPLINE_CURVE ( ( 1.000000000000000000, 0.9981721009331390171, 0.9981721009331390171, 1.000000000000000000 ) ) 
 REPRESENTATION_ITEM ( '' )  );
#4800 = CARTESIAN_POINT ( 'NONE',  ( 14.75683830447593614, -5.152850317976760408, -2.499999999999999556 ) ) ;
#4799 = CARTESIAN_POINT ( 'NONE',  ( 21.77915618962539313, 0.2033484107530734719, 8.424735242863125251 ) ) ;
#4801 = CARTESIAN_POINT ( 'NONE',  ( 81.16101395366625582, 61.30084446962304412, -1.089225060638851161 ) ) ;
#4802 = CARTESIAN_POINT ( 'NONE',  ( 78.34436985318809832, 64.89959302631085336, 3.091829831932942252 ) ) ;
#4803 = ORIENTED_EDGE ( 'NONE', *, *, #36733, .F. ) ;
#4804 = B_SPLINE_CURVE_WITH_KNOTS ( 'NONE', 3,
 ( #11778, #5840, #36316, #5020, #14672, #36713, #8496, #6456, #34681, #3394 ),
 .UNSPECIFIED., .F., .F.,
 ( 4, 2, 2, 2, 4 ),
 ( 0.5001220714136037637, 0.6250915535602028505, 0.7500610357068019374, 0.8750305178534010242, 1.000000000000000000 ),
 .UNSPECIFIED. ) ;
#4805 = DIRECTION ( 'NONE',  ( -0.000000000000000000, -0.000000000000000000, 1.000000000000000000 ) ) ;
#4806 = EDGE_CURVE ( 'NONE', #13346, #38041, #12569, .T. ) ;
#4807 = CARTESIAN_POINT ( 'NONE',  ( 82.43454424851958606, 64.20405324974034045, 1.755995906647955795 ) ) ;
#4809 = VERTEX_POINT ( 'NONE', #25758 ) ;
#4808 = CARTESIAN_POINT ( 'NONE',  ( -34.44874870218064444, -25.49307895267003587, 6.700000000000000178 ) ) ;
#4810 = CARTESIAN_POINT ( 'NONE',  ( 28.22557690513166762, 1.384627073958520249, -4.541740331631825001 ) ) ;
#4811 = CARTESIAN_POINT ( 'NONE',  ( -62.78278205347345420, 35.70412497698336551, -5.569918731383365795 ) ) ;
#4812 = ORIENTED_EDGE ( 'NONE', *, *, #38697, .F. ) ;
#4813 = CIRCLE ( 'NONE', #4778, 3.000000000000002665 ) ;
#4814 = CARTESIAN_POINT ( 'NONE',  ( -81.82461451913749784, -5.600584684740513630, -0.2075332267605694003 ) ) ;
#4815 = CARTESIAN_POINT ( 'NONE',  ( 23.06578088975079410, 0.3556780097724844825, -5.946217273123633795 ) ) ;
#4816 = CARTESIAN_POINT ( 'NONE',  ( 5.153606329123710417, -28.99954047225407905, 6.887161170156904433 ) ) ;
#4817 = EDGE_LOOP ( 'NONE', ( #10398, #36335, #26717, #36229 ) ) ;
#4818 = CARTESIAN_POINT ( 'NONE',  ( 37.10903179270489716, -2.404814453197160695, -5.951927498713348363 ) ) ;
#4819 = CARTESIAN_POINT ( 'NONE',  ( -35.07867591359219972, -26.64985754041175525, 6.700000000000000178 ) ) ;
#4820 = DIRECTION ( 'NONE',  ( 0.7660444431189740166, 0.6427876096865440259, 0.000000000000000000 ) ) ;
#4821 = CARTESIAN_POINT ( 'NONE',  ( -66.99872204295122913, 28.48507918597134037, 12.49999999999999645 ) ) ;
#4822 = DIRECTION ( 'NONE',  ( 1.000000000000000000, 0.000000000000000000, 0.000000000000000000 ) ) ;
#4823 = FACE_OUTER_BOUND ( 'NONE', #17882, .T. ) ;
#4824 = CARTESIAN_POINT ( 'NONE',  ( 2.458815852472819419, -32.89148182386498576, 7.139196562012271485 ) ) ;
#4825 = VECTOR ( 'NONE', #18143, 1000.000000000000000 ) ;
#4826 = EDGE_CURVE ( 'NONE', #32259, #30233, #5513, .T. ) ;
#4827 = CARTESIAN_POINT ( 'NONE',  ( 1.784616897348816789, -26.07094378080929431, 6.865554069792297653 ) ) ;
#4828 = ORIENTED_EDGE ( 'NONE', *, *, #30544, .F. ) ;
#4829 = CARTESIAN_POINT ( 'NONE',  ( 66.27376694608996388, 57.73522568913447373, 4.000000000000000000 ) ) ;
#4830 = CARTESIAN_POINT ( 'NONE',  ( 73.59222858082205221, 59.63291812028631966, -3.785151435545463183 ) ) ;
#4831 = CIRCLE ( 'NONE', #14654, 0.1000000000000028644 ) ;
#4832 = VERTEX_POINT ( 'NONE', #1456 ) ;
#4833 = CARTESIAN_POINT ( 'NONE',  ( 87.02687067233559048, -1.029203037998749570, 5.291918051785640564 ) ) ;
#4834 = CARTESIAN_POINT ( 'NONE',  ( -0.9894248136993964993, -27.33053388830764874, 7.635761828346571356 ) ) ;
#4835 = ADVANCED_FACE ( 'NONE', ( #4545 ), #39098, .F. ) ;
#4836 = CARTESIAN_POINT ( 'NONE',  ( -0.8549290955373274326, -27.17820325474436771, 6.931070083220554068 ) ) ;
#4837 = APPLICATION_PROTOCOL_DEFINITION ( 'draft international standard', 'automotive_design', 1998, #11045 ) ;
#4838 = LINE ( 'NONE', #29947, #35065 ) ;
#4839 = EDGE_CURVE ( 'NONE', #33506, #35057, #11091, .T. ) ;
#4840 = CARTESIAN_POINT ( 'NONE',  ( 24.78141585081923992, 3.030236314331866687, 3.301436159119843339 ) ) ;
#4841 = CARTESIAN_POINT ( 'NONE',  ( 5.054793046568992310, -30.12489038615697012, 7.695279973900954751 ) ) ;
#4842 = ORIENTED_EDGE ( 'NONE', *, *, #35132, .T. ) ;
#4843 = CARTESIAN_POINT ( 'NONE',  ( 79.84618440311783161, 63.29375160576378079, -3.738478073092017517 ) ) ;
#4844 = CARTESIAN_POINT ( 'NONE',  ( 33.87044765521353185, -5.290189018693288503, 1.967003440103135548 ) ) ;
#4845 = CARTESIAN_POINT ( 'NONE',  ( 78.72519613238203817, 65.48187369539458302, 2.679976076788566530 ) ) ;
#4846 = CARTESIAN_POINT ( 'NONE',  ( 0.5254594208927613197, -26.37938586935893071, 7.756377446753165650 ) ) ;
#4847 = FACE_OUTER_BOUND ( 'NONE', #37542, .T. ) ;
#4848 = CARTESIAN_POINT ( 'NONE',  ( 15.06093162081344694, 12.12817333299150135, -2.535899686230826067 ) ) ;
#4849 = DIRECTION ( 'NONE',  ( 1.000000000000000000, 0.000000000000000000, 0.000000000000000000 ) ) ;
#4850 = CARTESIAN_POINT ( 'NONE',  ( 21.85643539959776760, 8.340603020592608274, -8.602649199348869402 ) ) ;
#4851 = VERTEX_POINT ( 'NONE', #2266 ) ;
#4852 = CARTESIAN_POINT ( 'NONE',  ( -77.10977740483862419, 9.586436412528746231, 7.873194102962211005 ) ) ;
#4853 = CARTESIAN_POINT ( 'NONE',  ( 14.73544869152550696, -5.109937501475094734, 2.500000000000000444 ) ) ;
#4854 = VECTOR ( 'NONE', #8552, 1000.000000000000000 ) ;
#4855 = CIRCLE ( 'NONE', #34485, 64.42751648247021024 ) ;
#4856 = CARTESIAN_POINT ( 'NONE',  ( -75.61667019430753101, 8.531147133863177245, -10.24029099541588650 ) ) ;
#4857 = CARTESIAN_POINT ( 'NONE',  ( 37.21266877546892005, -2.743693451709001252, -6.000906079407704929 ) ) ;
#4858 = CARTESIAN_POINT ( 'NONE',  ( 79.20700709577714349, 65.89182355360533450, 2.372413575842139188 ) ) ;
#4859 = DIRECTION ( 'NONE',  ( 0.000000000000000000, 0.000000000000000000, 1.000000000000000000 ) ) ;
#4860 = CARTESIAN_POINT ( 'NONE',  ( 3.859195309938889817, -26.94322764099525003, 7.712764235869101093 ) ) ;
#4861 = LINE ( 'NONE', #26495, #12202 ) ;
#4862 = CARTESIAN_POINT ( 'NONE',  ( 0.6856660200322349796, -26.22025332505815598, 6.951256099901589991 ) ) ;
#4863 = VECTOR ( 'NONE', #5598, 1000.000000000000000 ) ;
#4864 = CARTESIAN_POINT ( 'NONE',  ( -64.85784325972055342, 34.81586596186931359, 6.466735817496056526 ) ) ;
#4865 = CARTESIAN_POINT ( 'NONE',  ( 1.108594127457504630, -33.01953560066821325, 7.638991368224661294 ) ) ;
#4866 = VECTOR ( 'NONE', #2283, 1000.000000000000000 ) ;
#4867 = CARTESIAN_POINT ( 'NONE',  ( 67.85873555399604129, 57.94375731920307260, 3.976226663256418714 ) ) ;
#4868 = CARTESIAN_POINT ( 'NONE',  ( 36.79866761904986561, -2.554542194025152035, 5.949720079728989752 ) ) ;
#4869 = EDGE_CURVE ( 'NONE', #25288, #31282, #24273, .T. ) ;
#4870 = FACE_OUTER_BOUND ( 'NONE', #12919, .T. ) ;
#4872 = ADVANCED_FACE ( 'NONE', ( #11899 ), #2069, .F. ) ;
#4871 = CARTESIAN_POINT ( 'NONE',  ( 85.42332570945818304, 2.406190724219733568, -3.391956346677281076 ) ) ;
#4874 = CARTESIAN_POINT ( 'NONE',  ( 29.58360395842353796, 0.1927886596133820130, -4.823634898514195690 ) ) ;
#4873 = CARTESIAN_POINT ( 'NONE',  ( 80.68504733838216225, 63.31860838049917106, -3.572022490087447988 ) ) ;
#4875 = CARTESIAN_POINT ( 'NONE',  ( -1.626196100676897238, -28.86720385366933428, 6.864276522220859711 ) ) ;
#4876 = CARTESIAN_POINT ( 'NONE',  ( -59.64698295252581772, 26.74637988513383391, 7.056669117542213598 ) ) ;
#4877 = ORIENTED_EDGE ( 'NONE', *, *, #28030, .T. ) ;
#4878 = CARTESIAN_POINT ( 'NONE',  ( -69.92837670882107659, -20.78299143688747819, 5.916079783099617906 ) ) ;
#4879 = EDGE_CURVE ( 'NONE', #38151, #1666, #7971, .T. ) ;
#4880 = ORIENTED_EDGE ( 'NONE', *, *, #35633, .F. ) ;
#4881 = AXIS2_PLACEMENT_3D ( 'NONE', #5832, #8280, #14872 ) ;
#4882 = ADVANCED_FACE ( 'NONE', ( #24472 ), #21193, .F. ) ;
#4883 = ORIENTED_EDGE ( 'NONE', *, *, #31531, .F. ) ;
#4884 = ORIENTED_EDGE ( 'NONE', *, *, #25933, .F. ) ;
#4885 = CARTESIAN_POINT ( 'NONE',  ( 81.06091538032714539, 61.57736434115989965, -2.238287240292677449 ) ) ;
#4886 = CARTESIAN_POINT ( 'NONE',  ( -1.518811278079208238, -28.19634271586866703, 6.974994249511789590 ) ) ;
#4887 = CARTESIAN_POINT ( 'NONE',  ( 78.85680892556288768, 65.81502797165208563, 2.238287240292551772 ) ) ;
#4888 = CARTESIAN_POINT ( 'NONE',  ( 24.43811349724861515, 1.135655287698857929, 4.744166224008156796 ) ) ;
#4890 = ORIENTED_EDGE ( 'NONE', *, *, #80, .F. ) ;
#4889 = CARTESIAN_POINT ( 'NONE',  ( -0.7646741769630207575, -27.22825162539180610, 6.969307238440508812 ) ) ;
#4891 = CIRCLE ( 'NONE', #6231, 2.500000000000002220 ) ;
#4892 = PLANE ( 'NONE',  #31853 ) ;
#4894 = CARTESIAN_POINT ( 'NONE',  ( -1.337427566997555717, -27.83163680677632001, 7.635761828346574021 ) ) ;
#4893 = CARTESIAN_POINT ( 'NONE',  ( -36.24874870218063450, -26.64985754041175525, 6.700000000000000178 ) ) ;
#4895 = CARTESIAN_POINT ( 'NONE',  ( -63.84790524989457339, 35.84013490037983729, -7.344445564913361757 ) ) ;
#4896 = CYLINDRICAL_SURFACE ( 'NONE', #7430, 3.399999999999999911 ) ;
#4897 = CARTESIAN_POINT ( 'NONE',  ( 22.71523255480387604, 4.231905031421672625, -3.372270972680762036 ) ) ;
#4898 = ORIENTED_EDGE ( 'NONE', *, *, #21253, .F. ) ;
#4899 = CARTESIAN_POINT ( 'NONE',  ( 5.146918245836023864, -30.17145770867207588, 7.762796336881260473 ) ) ;
#4900 = ORIENTED_EDGE ( 'NONE', *, *, #17343, .F. ) ;
#4901 = CARTESIAN_POINT ( 'NONE',  ( 22.53076953550388950, -1.409035359855524749, -9.122014670555362414 ) ) ;
#4902 = DIRECTION ( 'NONE',  ( 1.000000000000000000, 0.000000000000000000, -0.000000000000000000 ) ) ;
#4903 = LINE ( 'NONE', #17435, #13645 ) ;
#4904 = CARTESIAN_POINT ( 'NONE',  ( 80.61314501154876666, 64.81116531652718038, 3.343039074470575578 ) ) ;
#4905 = CARTESIAN_POINT ( 'NONE',  ( 84.58609069645564205, 2.764543530557054041, -2.886136738505205912 ) ) ;
#4906 = DIRECTION ( 'NONE',  ( 0.000000000000000000, 0.000000000000000000, -1.000000000000000000 ) ) ;
#4907 = ORIENTED_EDGE ( 'NONE', *, *, #28416, .T. ) ;
#4908 = CARTESIAN_POINT ( 'NONE',  ( -1.512235554918550662, -28.43529712411073263, 7.257242401810563237 ) ) ;
#4909 = CARTESIAN_POINT ( 'NONE',  ( -79.55031281509177177, -5.535808051698485777, 7.055139847234975115 ) ) ;
#4910 = AXIS2_PLACEMENT_3D ( 'NONE', #5636, #18175, #30767 ) ;
#4911 = AXIS2_PLACEMENT_3D ( 'NONE', #20494, #14318, #26888 ) ;
#4912 = CARTESIAN_POINT ( 'NONE',  ( 25.01091298175105848, 3.329590532566609529, -1.936828115965013142 ) ) ;
#4913 = CARTESIAN_POINT ( 'NONE',  ( 23.83302048315688992, -3.061032822375338025, -3.850069817691858187 ) ) ;
#4914 = CARTESIAN_POINT ( 'NONE',  ( 35.45326567125915318, -1.915512047056902256, -5.739737567107160210 ) ) ;
#4915 = FACE_OUTER_BOUND ( 'NONE', #7970, .T. ) ;
#4916 = VECTOR ( 'NONE', #15508, 1000.000000000000000 ) ;
#4917 = CARTESIAN_POINT ( 'NONE',  ( 21.73976651585488895, 0.3939909484403775197, -8.664878499868692074 ) ) ;
#4918 = CARTESIAN_POINT ( 'NONE',  ( -0.4994316697168441066, -26.97748265041383320, 7.748216051605117727 ) ) ;
#4919 = ORIENTED_EDGE ( 'NONE', *, *, #30978, .T. ) ;
#4920 = CARTESIAN_POINT ( 'NONE',  ( 37.04303371899823816, -2.892454996259951727, 5.987859319642387490 ) ) ;
#4921 = DIRECTION ( 'NONE',  ( -1.000000000000000000, 0.000000000000000000, 0.000000000000000000 ) ) ;
#4922 = CARTESIAN_POINT ( 'NONE',  ( 31.83096507438640188, -2.965444956201115811, -5.174389953294182831 ) ) ;
#4923 = VERTEX_POINT ( 'NONE', #39919 ) ;
#4924 = ORIENTED_EDGE ( 'NONE', *, *, #25531, .F. ) ;
#4925 = CARTESIAN_POINT ( 'NONE',  ( 20.91979337306159081, 4.581248967235889147, 2.652518752413522307 ) ) ;
#4926 = CARTESIAN_POINT ( 'NONE',  ( -1.647480198169903431, -30.59059884262676121, 6.921725064902949143 ) ) ;
#4927 = LINE ( 'NONE', #10693, #37919 ) ;
#4928 = DIRECTION ( 'NONE',  ( 1.000000000000000000, 0.000000000000000000, 0.000000000000000000 ) ) ;
#4929 = ADVANCED_FACE ( 'NONE', ( #37029 ), #28050, .F. ) ;
#4930 = VERTEX_POINT ( 'NONE', #23850 ) ;
#4931 = CARTESIAN_POINT ( 'NONE',  ( -1.744066689084928345, -30.19099175420856440, 7.635761828346576685 ) ) ;
#4932 = ADVANCED_FACE ( 'NONE', ( #33975 ), #15004, .T. ) ;
#4933 = ORIENTED_EDGE ( 'NONE', *, *, #14864, .T. ) ;
#4934 = EDGE_CURVE ( 'NONE', #863, #14484, #14790, .T. ) ;
#4935 = VERTEX_POINT ( 'NONE', #39501 ) ;
#4936 = CARTESIAN_POINT ( 'NONE',  ( 5.056857618328627346, -29.02759656560906976, 6.894806418505346812 ) ) ;
#4937 =( LENGTH_UNIT ( ) NAMED_UNIT ( * ) SI_UNIT ( .MILLI., .METRE. ) );
#4938 = ORIENTED_EDGE ( 'NONE', *, *, #21078, .F. ) ;
#4939 = CARTESIAN_POINT ( 'NONE',  ( -56.64002613362055882, 29.83241628681515323, -1.779850828381725814 ) ) ;
#4940 = ORIENTED_EDGE ( 'NONE', *, *, #31498, .F. ) ;
#4942 = CARTESIAN_POINT ( 'NONE',  ( 4.312106210101242176, -27.39300398378253476, 7.775108481317161591 ) ) ;
#4941 = CARTESIAN_POINT ( 'NONE',  ( 4.792398414354069658, -27.92993265294842331, 6.867199677474202346 ) ) ;
#4943 = ORIENTED_EDGE ( 'NONE', *, *, #18735, .F. ) ;
#4944 = CARTESIAN_POINT ( 'NONE',  ( 21.98915976803599293, 4.682270550536856923, 3.756922458215664395 ) ) ;
#4945 = CARTESIAN_POINT ( 'NONE',  ( 79.28422506984790630, 66.27750502035057423, -1.322881339814841573 ) ) ;
#4946 = VECTOR ( 'NONE', #29631, 1000.000000000000000 ) ;
#4947 = CIRCLE ( 'NONE', #10868, 8.080217238368755162 ) ;
#4948 = DIRECTION ( 'NONE',  ( -0.000000000000000000, -0.000000000000000000, 1.000000000000000000 ) ) ;
#4949 = ORIENTED_EDGE ( 'NONE', *, *, #39881, .T. ) ;
#4951 = CARTESIAN_POINT ( 'NONE',  ( 1.084781629859024710, -26.22612389321864512, 7.652160403243385645 ) ) ;
#4950 = CARTESIAN_POINT ( 'NONE',  ( 0.09453809279883360062, -26.57304938770676728, 7.768425012602595991 ) ) ;
#4952 = CARTESIAN_POINT ( 'NONE',  ( -1.794705841495275900, -29.38469240096594604, 6.989977667959445640 ) ) ;
#4953 = CARTESIAN_POINT ( 'NONE',  ( 73.75428705932469597, 62.33035115498114465, 3.485789274173696661 ) ) ;
#4954 = EDGE_LOOP ( 'NONE', ( #17719, #25856, #28013, #19643, #9029 ) ) ;
#4955 = CARTESIAN_POINT ( 'NONE',  ( 22.04665046261544248, 2.511317956134706986, -5.313134278748806061 ) ) ;
#4956 = CARTESIAN_POINT ( 'NONE',  ( -64.08758708074093136, 36.76354445449373998, 3.435823087746894267 ) ) ;
#4957 = VECTOR ( 'NONE', #11637, 1000.000000000000000 ) ;
#4958 = DIRECTION ( 'NONE',  ( 0.9637806624122927657, -0.2666961468790326473, 1.731454049777543614E-15 ) ) ;
#4959 = DIRECTION ( 'NONE',  ( 1.000000000000000000, 0.000000000000000000, 0.000000000000000000 ) ) ;
#4960 = CARTESIAN_POINT ( 'NONE',  ( 0.8807958757747544887, -0.5999999999999994227, -3.993526596136941720 ) ) ;
#4961 = DIRECTION ( 'NONE',  ( 1.000000000000000000, 0.000000000000000000, -0.000000000000000000 ) ) ;
#4962 = CARTESIAN_POINT ( 'NONE',  ( 80.71114116412925910, 65.59088185864123943, 2.713791510777070037 ) ) ;
#4963 = CARTESIAN_POINT ( 'NONE',  ( 85.36681891225420316, 2.469661840813765608, 2.484336716295309166 ) ) ;
#4964 = CARTESIAN_POINT ( 'NONE',  ( 27.93970670347097851, 2.313158937601060838, 2.612756796560576689 ) ) ;
#4965 = CARTESIAN_POINT ( 'NONE',  ( -1.788417373966595170, -29.89300939100614940, 7.566278858797844897 ) ) ;
#4966 = B_SPLINE_CURVE_WITH_KNOTS ( 'NONE', 3,
 ( #28927, #3632, #35327, #38175, #10168, #25430, #10578, #29329, #1146, #28722, #4223, #34721, #6501, #25836, #933, #35522, #25630, #9978, #19855 ),
 .UNSPECIFIED., .F., .F.,
 ( 4, 3, 3, 3, 3, 3, 4 ),
 ( 2.176562864887236392E-18, 2.546128104244634667E-05, 5.711050680483281499E-05, 8.113074941675401297E-05, 0.0001053129305727108458, 0.0001360598016347140465, 0.0001612931755702068262 ),
 .UNSPECIFIED. ) ;
#4967 = FACE_OUTER_BOUND ( 'NONE', #29900, .T. ) ;
#4968 = DIRECTION ( 'NONE',  ( -0.9396926207859058744, -0.3420201433256757628, -0.000000000000000000 ) ) ;
#4969 = CARTESIAN_POINT ( 'NONE',  ( 17.15960986616130057, -3.267607912849484375, 2.851956029205625409 ) ) ;
#4970 = CARTESIAN_POINT ( 'NONE',  ( 0.07757799509440113650, -26.46888505406446512, 6.875780273367532835 ) ) ;
#4971 = CARTESIAN_POINT ( 'NONE',  ( 36.14547465321244601, -3.195512951925109757, -5.847773519878426640 ) ) ;
#4972 = LINE ( 'NONE', #33602, #28616 ) ;
#4973 = LINE ( 'NONE', #17709, #10149 ) ;
#4974 = CARTESIAN_POINT ( 'NONE',  ( -1.032223829037264728, -34.03013334986905392, 7.013842709614101167 ) ) ;
#4975 = CARTESIAN_POINT ( 'NONE',  ( 4.323060980164646239, -31.86896110803267490, 7.782861076432731728 ) ) ;
#4976 = AXIS2_PLACEMENT_3D ( 'NONE', #25692, #19517, #29388 ) ;
#4977 = DIRECTION ( 'NONE',  ( 0.000000000000000000, 0.000000000000000000, 1.000000000000000000 ) ) ;
#4978 = CIRCLE ( 'NONE', #27982, 0.1000000000000028644 ) ;
#4979 = ORIENTED_EDGE ( 'NONE', *, *, #30612, .T. ) ;
#4980 = CARTESIAN_POINT ( 'NONE',  ( 36.02627438905632573, -1.730095084077468481, 5.776804761617037265 ) ) ;
#4981 = DIRECTION ( 'NONE',  ( -0.5751513419797895654, -0.4826092789263638494, -0.6605219282605402364 ) ) ;
#4982 = CARTESIAN_POINT ( 'NONE',  ( 67.39181666045010388, 58.30934502646129403, -3.993945454764282310 ) ) ;
#4983 = AXIS2_PLACEMENT_3D ( 'NONE', #269, #6035, #31360 ) ;
#4984 = CYLINDRICAL_SURFACE ( 'NONE', #7589, 0.1000000000000028644 ) ;
#4985 = ORIENTED_EDGE ( 'NONE', *, *, #40046, .F. ) ;
#4986 = FACE_OUTER_BOUND ( 'NONE', #4597, .T. ) ;
#4988 = EDGE_CURVE ( 'NONE', #9291, #14078, #36465, .T. ) ;
#4987 = CARTESIAN_POINT ( 'NONE',  ( -25.07867591359219617, -26.64985754041175525, 6.700000000000000178 ) ) ;
#4989 = LINE ( 'NONE', #32804, #14108 ) ;
#4990 = CARTESIAN_POINT ( 'NONE',  ( -78.09790289012752851, 11.26711229117069735, 6.983148571841773844 ) ) ;
#4991 = CARTESIAN_POINT ( 'NONE',  ( 0.4563090418891334044, -32.84136142028145144, 6.878641987404678027 ) ) ;
#4992 = DIRECTION ( 'NONE',  ( 1.000000000000000000, 0.000000000000000000, 0.000000000000000000 ) ) ;
#4993 = VERTEX_POINT ( 'NONE', #27564 ) ;
#4994 = CARTESIAN_POINT ( 'NONE',  ( 21.99104032157442390, 5.601135775457250610, 3.099302606858675535 ) ) ;
#4995 = CARTESIAN_POINT ( 'NONE',  ( 81.74417899799368570, 61.69322615925144504, -1.090531591958677327 ) ) ;
#4996 = CARTESIAN_POINT ( 'NONE',  ( 79.75420125634298074, 65.05222905597021565, 3.324099845469147052 ) ) ;
#4997 = CARTESIAN_POINT ( 'NONE',  ( -0.02383034049480821370, -32.61575874214327087, 7.660770905198784675 ) ) ;
#4998 = ORIENTED_EDGE ( 'NONE', *, *, #2009, .F. ) ;
#4999 = CARTESIAN_POINT ( 'NONE',  ( 78.65108613080990096, 60.71083206350689210, -2.889099817377091650 ) ) ;
#5000 = B_SPLINE_CURVE_WITH_KNOTS ( 'NONE', 3,
 ( #18688, #25090, #24461, #6563, #37619, #5737, #31272, #37830, #9014, #19109, #9634, #40717, #22217, #9418, #24885 ),
 .UNSPECIFIED., .F., .F.,
 ( 4, 2, 2, 1, 1, 1, 1, 1, 2, 4 ),
 ( 0.4819642147472752991, 0.4909821073736378994, 0.4954910536868194493, 0.4977455268434102242, 0.4988727634217053897, 0.4994363817108530279, 0.4997181908554266805, 0.4998590954277135068, 0.4999295477138567256, 0.5000000000000000000 ),
 .UNSPECIFIED. ) ;
#5002 = CARTESIAN_POINT ( 'NONE',  ( 14.74846712742400001, -5.105618172135831578, -2.500089296388391613 ) ) ;
#5001 = CARTESIAN_POINT ( 'NONE',  ( 26.06852323663950344, 0.7122034496989984032, 4.422876470770067847 ) ) ;
#5003 = CARTESIAN_POINT ( 'NONE',  ( 81.29424054903955721, 63.61798189665201875, -3.316380171282754308 ) ) ;
#5004 = CARTESIAN_POINT ( 'NONE',  ( 77.75442706423145012, 65.27774734742538953, 2.313798345564205494 ) ) ;
#5005 = ORIENTED_EDGE ( 'NONE', *, *, #9333, .F. ) ;
#5006 = CARTESIAN_POINT ( 'NONE',  ( -63.08379346057677139, 18.80112958435941906, 12.49999999999999645 ) ) ;
#5007 = CARTESIAN_POINT ( 'NONE',  ( 81.92984576605168456, 61.94483778347748881, 1.306649493516907290 ) ) ;
#5009 = CARTESIAN_POINT ( 'NONE',  ( 36.10284116201629701, 0.9159659085930716982, -6.000000000000000000 ) ) ;
#5008 = CARTESIAN_POINT ( 'NONE',  ( 0.000000000000000000, 0.000000000000000000, 0.000000000000000000 ) ) ;
#5010 = CARTESIAN_POINT ( 'NONE',  ( 29.52748857962093965, -2.713093490715668743, -5.368793458836177201 ) ) ;
#5011 = EDGE_CURVE ( 'NONE', #36027, #10700, #34327, .T. ) ;
#5012 = DIRECTION ( 'NONE',  ( -0.000000000000000000, -0.000000000000000000, 1.000000000000000000 ) ) ;
#5013 = ORIENTED_EDGE ( 'NONE', *, *, #9148, .F. ) ;
#5014 = CARTESIAN_POINT ( 'NONE',  ( 1.626267501107426350, -33.06915981226823931, 6.867280401193707640 ) ) ;
#5015 = CARTESIAN_POINT ( 'NONE',  ( 22.29087474900200050, 0.2567279992677524159, -7.116332770368763327 ) ) ;
#5016 = AXIS2_PLACEMENT_3D ( 'NONE', #35112, #28916, #32018 ) ;
#5017 = LINE ( 'NONE', #20054, #3808 ) ;
#5018 = CARTESIAN_POINT ( 'NONE',  ( 5.001438667734867671, -30.73314912614656436, 7.697032948437507294 ) ) ;
#5019 = CARTESIAN_POINT ( 'NONE',  ( -1.699609906766909040, -29.50756078821139639, 7.152329793038292749 ) ) ;
#5020 = CARTESIAN_POINT ( 'NONE',  ( -71.43157283993535600, 0.09103159405784894131, 3.980077070333584821 ) ) ;
#5021 = CARTESIAN_POINT ( 'NONE',  ( 37.00929082827390459, -2.250120747072028138, -5.913434965054697123 ) ) ;
#5022 = CARTESIAN_POINT ( 'NONE',  ( 3.430329942220429640, -32.60247582573452263, 7.778495531946297170 ) ) ;
#5023 = DIRECTION ( 'NONE',  ( 0.000000000000000000, 0.000000000000000000, 1.000000000000000000 ) ) ;
#5024 = CARTESIAN_POINT ( 'NONE',  ( 5.121025113131824291, -30.31110547187388349, 6.870724624169667116 ) ) ;
#5025 = CARTESIAN_POINT ( 'NONE',  ( 5.001438667734867671, -30.73314912614656436, 7.686927408461905920 ) ) ;
#5026 = CARTESIAN_POINT ( 'NONE',  ( 2.663812202415797969, -32.83057702712517312, 6.959317978105163505 ) ) ;
#5027 = CARTESIAN_POINT ( 'NONE',  ( 5.093942500299159626, -29.77923753713957922, 6.939395833800446667 ) ) ;
#5028 = ADVANCED_FACE ( 'NONE', ( #40120 ), #2687, .F. ) ;
#5029 = CARTESIAN_POINT ( 'NONE',  ( 1.890031703046834100, -26.07506968295128758, 6.931070083220556732 ) ) ;
#5030 = CARTESIAN_POINT ( 'NONE',  ( 2.147225889248687736, -33.04129679599670055, 6.887547729233689964 ) ) ;
#5031 = ORIENTED_EDGE ( 'NONE', *, *, #11598, .F. ) ;
#5032 = ORIENTED_EDGE ( 'NONE', *, *, #16086, .T. ) ;
#5033 = CARTESIAN_POINT ( 'NONE',  ( 66.42990020876143831, 57.76860247958609307, 4.000000000000007105 ) ) ;
#5034 = CARTESIAN_POINT ( 'NONE',  ( 72.61754431144450450, 61.86111285056382059, -3.476886323448412419 ) ) ;
#5035 = VERTEX_POINT ( 'NONE', #24685 ) ;
#5036 = CARTESIAN_POINT ( 'NONE',  ( 87.26468549332315661, -1.699173523771937644, 4.325011594718342067 ) ) ;
#5038 = EDGE_CURVE ( 'NONE', #4541, #2378, #8198, .T. ) ;
#5037 = CARTESIAN_POINT ( 'NONE',  ( 0.1522824367581332439, -26.54282551325666617, 6.882085323592685988 ) ) ;
#5039 = CARTESIAN_POINT ( 'NONE',  ( 3.048699747109260283, -26.44869756457103094, 6.911401339314957148 ) ) ;
#5040 =( BOUNDED_CURVE ( )  B_SPLINE_CURVE ( 3, ( #22178, #8976, #6114, #31842 ),
 .UNSPECIFIED., .F., .T. ) 
 B_SPLINE_CURVE_WITH_KNOTS ( ( 4, 4 ),
 ( 1.381924640371168467, 1.574767692156077148 ),
 .UNSPECIFIED. ) 
 CURVE ( )  GEOMETRIC_REPRESENTATION_ITEM ( )  RATIONAL_B_SPLINE_CURVE ( ( 1.000000000000000000, 0.9969033633783032089, 0.9969033633783032089, 1.000000000000000000 ) ) 
 REPRESENTATION_ITEM ( '' )  );
#5041 = VECTOR ( 'NONE', #37740, 1000.000000000000000 ) ;
#5042 = CARTESIAN_POINT ( 'NONE',  ( -0.8539220219492742459, -27.17712883508125898, 6.971170733404098208 ) ) ;
#5043 = CIRCLE ( 'NONE', #28055, 2.500000000000000000 ) ;
#5044 = DIRECTION ( 'NONE',  ( 1.000000000000000000, 0.000000000000000000, 0.000000000000000000 ) ) ;
#5045 = FACE_OUTER_BOUND ( 'NONE', #26119, .T. ) ;
#5046 = CARTESIAN_POINT ( 'NONE',  ( -20.97867591359219475, -26.64985754041175525, 6.800000000000000711 ) ) ;
#5047 = ORIENTED_EDGE ( 'NONE', *, *, #11462, .T. ) ;
#5048 = CARTESIAN_POINT ( 'NONE',  ( 80.48656635915796187, 62.05344631111049836, -3.128253119413326289 ) ) ;
#5049 = CARTESIAN_POINT ( 'NONE',  ( 16.68329415696692664, 9.858079400870805031, -2.499999999999912959 ) ) ;
#5050 = CARTESIAN_POINT ( 'NONE',  ( 79.98443850338786376, 63.35773072451035404, 3.725738571856552106 ) ) ;
#5051 = CARTESIAN_POINT ( 'NONE',  ( -8.978675913592192970, -26.64985754041175525, 6.700000000000000178 ) ) ;
#5052 = EDGE_CURVE ( 'NONE', #5880, #33546, #23899, .T. ) ;
#5053 = CARTESIAN_POINT ( 'NONE',  ( 4.425213896693725779, -27.53636676661391647, 7.006423389747786779 ) ) ;
#5054 = CARTESIAN_POINT ( 'NONE',  ( 3.956488544215869485, -27.02628791689333099, 6.866852738645442322 ) ) ;
#5055 = DIRECTION ( 'NONE',  ( -0.000000000000000000, -0.000000000000000000, 1.000000000000000000 ) ) ;
#5056 = CARTESIAN_POINT ( 'NONE',  ( 21.85643539959774273, -7.955861821551272861, 12.12136874776577322 ) ) ;
#5057 = ORIENTED_EDGE ( 'NONE', *, *, #635, .F. ) ;
#5058 = CARTESIAN_POINT ( 'NONE',  ( -80.77358443228958151, 10.51022734914309531, 4.964753886184787746 ) ) ;
#5059 = CARTESIAN_POINT ( 'NONE',  ( 14.78321307761975234, -5.165297048227083465, 2.500001704151146420 ) ) ;
#5060 = AXIS2_PLACEMENT_3D ( 'NONE', #18013, #26884, #8543 ) ;
#5061 = CARTESIAN_POINT ( 'NONE',  ( -77.38302135847544605, 11.04206681912608978, -7.647767078175882638 ) ) ;
#5062 = CARTESIAN_POINT ( 'NONE',  ( 1.512295318426525759, -32.96472816114737725, 6.895222827070022653 ) ) ;
#5063 = CARTESIAN_POINT ( 'NONE',  ( 2.423740107909631902, -26.24775251191726611, 6.865312560952602894 ) ) ;
#5064 = CARTESIAN_POINT ( 'NONE',  ( 78.77361741396555317, 66.07891176884449180, 1.467306180864091703 ) ) ;
#5065 = CARTESIAN_POINT ( 'NONE',  ( -1.527091137229058981, -30.63925276425332811, 7.774064877406527074 ) ) ;
#5066 = DIRECTION ( 'NONE',  ( 0.000000000000000000, 0.000000000000000000, 1.000000000000000000 ) ) ;
#5067 = CARTESIAN_POINT ( 'NONE',  ( -75.45330471031414277, 33.71485196875532608, 21.52833696633422988 ) ) ;
#5068 = CARTESIAN_POINT ( 'NONE',  ( 0.6846915864468829938, -26.22054737195424323, 6.971170733404100872 ) ) ;
#5069 = ADVANCED_FACE ( 'NONE', ( #36626 ), #27968, .F. ) ;
#5070 = EDGE_CURVE ( 'NONE', #18492, #141, #6684, .T. ) ;
#5071 = AXIS2_PLACEMENT_3D ( 'NONE', #2172, #39827, #4098 ) ;
#5072 = AXIS2_PLACEMENT_3D ( 'NONE', #7054, #35681, #29089 ) ;
#5073 = EDGE_CURVE ( 'NONE', #37085, #9686, #6771, .T. ) ;
#5074 = CARTESIAN_POINT ( 'NONE',  ( 4.501000646075883793, -27.47074450049024463, 6.951256099901593544 ) ) ;
#5075 = CARTESIAN_POINT ( 'NONE',  ( 87.90580911867260738, -0.3822524667802704168, 3.357330413655388757 ) ) ;
#5076 = DIRECTION ( 'NONE',  ( 0.000000000000000000, 0.000000000000000000, 1.000000000000000000 ) ) ;
#5077 = ORIENTED_EDGE ( 'NONE', *, *, #19547, .F. ) ;
#5078 = CARTESIAN_POINT ( 'NONE',  ( 67.36017643331848603, 58.39563743223260417, 3.987264345885670025 ) ) ;
#5079 = CARTESIAN_POINT ( 'NONE',  ( 36.21770968404204183, -2.179824564146979338, 5.859047543450206952 ) ) ;
#5080 = CARTESIAN_POINT ( 'NONE',  ( 2.231683959652603022, -33.01691039817721673, 7.782861076432731728 ) ) ;
#5081 = CARTESIAN_POINT ( 'NONE',  ( 88.21591849536395102, -0.7305820373589052563, 3.481732356799086769 ) ) ;
#5083 = CARTESIAN_POINT ( 'NONE',  ( 31.23875116262452778, -0.3865744936300196111, -5.081960649616163117 ) ) ;
#5082 = CARTESIAN_POINT ( 'NONE',  ( 31.38399832331403161, -1.255798082282080008, 5.972680360385385079 ) ) ;
#5084 = LINE ( 'NONE', #39446, #34046 ) ;
#5085 = CARTESIAN_POINT ( 'NONE',  ( -58.33732831438487665, 31.01206039140789983, 4.738023936417821602 ) ) ;
#5086 = CARTESIAN_POINT ( 'NONE',  ( -0.5913600112788022223, -32.21528109744426160, 6.875671892026064214 ) ) ;
#5087 = ORIENTED_EDGE ( 'NONE', *, *, #16076, .F. ) ;
#5088 = CARTESIAN_POINT ( 'NONE',  ( -71.83651116356016075, -21.21610000639230975, 3.930990725878106495 ) ) ;
#5089 = VERTEX_POINT ( 'NONE', #28382 ) ;
#5090 = ORIENTED_EDGE ( 'NONE', *, *, #27168, .T. ) ;
#5091 = CARTESIAN_POINT ( 'NONE',  ( 78.61081429290072720, 65.94468767047428059, -1.703597047176659940 ) ) ;
#5092 = CARTESIAN_POINT ( 'NONE',  ( -1.625555967947097225, -28.86417650903285548, 7.759451378593097637 ) ) ;
#5093 = AXIS2_PLACEMENT_3D ( 'NONE', #27238, #4428, #16953 ) ;
#5094 = CARTESIAN_POINT ( 'NONE',  ( 79.09343976728347059, 65.54176476638913584, 2.787474064117257733 ) ) ;
#5095 = CARTESIAN_POINT ( 'NONE',  ( 24.04774667349223094, 0.8530566696381411962, 5.040905544005979344 ) ) ;
#5097 = EDGE_LOOP ( 'NONE', ( #16309, #40363, #13808, #17192 ) ) ;
#5096 = DIRECTION ( 'NONE',  ( -0.1736481776669340227, 0.9848077530122074652, -0.000000000000000000 ) ) ;
#5098 = VECTOR ( 'NONE', #39151, 1000.000000000000000 ) ;
#5099 = EDGE_CURVE ( 'NONE', #8271, #20794, #7484, .T. ) ;
#5100 = CARTESIAN_POINT ( 'NONE',  ( 74.30211141138923381, 59.57442121254392475, -3.624554307378899054 ) ) ;
#5101 = DIRECTION ( 'NONE',  ( -0.000000000000000000, -0.000000000000000000, 1.000000000000000000 ) ) ;
#5103 = DIRECTION ( 'NONE',  ( 0.000000000000000000, 1.000000000000000000, 0.000000000000000000 ) ) ;
#5102 = CARTESIAN_POINT ( 'NONE',  ( 14.69558838330753936, -3.003688195628454238, -6.000000000000000888 ) ) ;
#5104 = CARTESIAN_POINT ( 'NONE',  ( 4.749297472835600331, -31.28869828601962766, 7.695279973900954751 ) ) ;
#5105 = CARTESIAN_POINT ( 'NONE',  ( -26.87867591359219333, -26.64985754041175525, 6.800000000000000711 ) ) ;
#5106 = CARTESIAN_POINT ( 'NONE',  ( 23.95987346625971171, 3.275624734069571442, -3.453389381892394638 ) ) ;
#5107 = ORIENTED_EDGE ( 'NONE', *, *, #23300, .T. ) ;
#5108 = CARTESIAN_POINT ( 'NONE',  ( 2.430498945370407782, -26.14692813174583108, 7.751599049952198506 ) ) ;
#5109 = EDGE_CURVE ( 'NONE', #28333, #18637, #38050, .T. ) ;
#5110 = CARTESIAN_POINT ( 'NONE',  ( 21.85643539959775339, 5.487231995601864476, 10.01193108169250578 ) ) ;
#5111 = ADVANCED_FACE ( 'NONE', ( #34185 ), #2889, .F. ) ;
#5112 = CARTESIAN_POINT ( 'NONE',  ( 4.976842733950423536, -28.33913446795707358, 7.695279973900954751 ) ) ;
#5113 = CARTESIAN_POINT ( 'NONE',  ( 78.68416471612012231, 66.05417514313617744, 1.083735637653860495 ) ) ;
#5114 = CARTESIAN_POINT ( 'NONE',  ( 87.67674921920735187, -0.7466428619051976856, -5.210926517169286676 ) ) ;
#5115 = CARTESIAN_POINT ( 'NONE',  ( -75.45330471031414277, 33.71485196875532608, -9.800414904976365804 ) ) ;
#5116 = ORIENTED_EDGE ( 'NONE', *, *, #12561, .F. ) ;
#5117 = AXIS2_PLACEMENT_3D ( 'NONE', #13719, #32667, #10011 ) ;
#5118 = DIRECTION ( 'NONE',  ( 1.000000000000000000, 0.000000000000000000, 0.000000000000000000 ) ) ;
#5119 = B_SPLINE_CURVE_WITH_KNOTS ( 'NONE', 3,
 ( #12436, #103, #34089, #28491, #9337, #18600, #31793, #5865, #3006, #27672, #27873, #9546, #21916, #12225, #37344, #40227, #12636, #24804, #18813, #9139, #21713, #34492, #3211, #25207, #37737 ),
 .UNSPECIFIED., .F., .F.,
 ( 4, 3, 3, 3, 3, 3, 3, 3, 4 ),
 ( 6.468151674593740786E-05, 9.076621574721993949E-05, 0.0001210204262067974786, 0.0001512763324577440531, 0.0001815301820994204274, 0.0002117781465860696215, 0.0002420274594459737711, 0.0002722905548971171980, 0.0002816827545175588422 ),
 .UNSPECIFIED. ) ;
#5120 = EDGE_CURVE ( 'NONE', #16194, #22132, #16226, .T. ) ;
#5121 = CARTESIAN_POINT ( 'NONE',  ( 5.057666307568779551, -29.03261825887476988, 6.889465824494256374 ) ) ;
#5122 = CARTESIAN_POINT ( 'NONE',  ( 33.12654886128940035, -3.652994402058499013, -5.215079931666823043 ) ) ;
#5123 = CARTESIAN_POINT ( 'NONE',  ( 22.91837443496737237, 2.645784632913941170, -3.783364632193285004 ) ) ;
#5124 = FACE_OUTER_BOUND ( 'NONE', #26549, .T. ) ;
#5125 = CARTESIAN_POINT ( 'NONE',  ( 26.78359742506201968, 1.531162930580288073, -4.367563350258214960 ) ) ;
#5126 = PLANE ( 'NONE',  #21569 ) ;
#5127 = EDGE_LOOP ( 'NONE', ( #26350, #8424, #39154, #29092 ) ) ;
#5128 = CARTESIAN_POINT ( 'NONE',  ( 34.33118553565899589, -1.490639677210669145, 5.564609824335974508 ) ) ;
#5129 = AXIS2_PLACEMENT_3D ( 'NONE', #36415, #8187, #26945 ) ;
#5130 = CARTESIAN_POINT ( 'NONE',  ( -1.158355754856540631, -27.72937577116574204, 6.876076431790005827 ) ) ;
#5131 = ORIENTED_EDGE ( 'NONE', *, *, #28017, .T. ) ;
#5132 = ORIENTED_EDGE ( 'NONE', *, *, #16450, .T. ) ;
#5133 = CARTESIAN_POINT ( 'NONE',  ( 35.22190015492834902, -1.045615856747100780, 5.409212822378231422 ) ) ;
#5134 = CARTESIAN_POINT ( 'NONE',  ( -24.24874870218063450, -26.64985754041175525, 6.800000000000000711 ) ) ;
#5135 = CARTESIAN_POINT ( 'NONE',  ( 14.66504043345076447, 12.84305297963188863, -2.500000000000000000 ) ) ;
#5136 = DIRECTION ( 'NONE',  ( 0.000000000000000000, 0.000000000000000000, -1.000000000000000000 ) ) ;
#5137 = ORIENTED_EDGE ( 'NONE', *, *, #13992, .F. ) ;
#5138 = FACE_OUTER_BOUND ( 'NONE', #3265, .T. ) ;
#5139 = ORIENTED_EDGE ( 'NONE', *, *, #23602, .F. ) ;
#5140 = VERTEX_POINT ( 'NONE', #12322 ) ;
#5141 = LINE ( 'NONE', #22179, #335 ) ;
#5142 = CARTESIAN_POINT ( 'NONE',  ( 81.14259283377289478, 61.75830469257449806, -2.468641556981999496 ) ) ;
#5143 = AXIS2_PLACEMENT_3D ( 'NONE', #2556, #21270, #37108 ) ;
#5144 = CARTESIAN_POINT ( 'NONE',  ( 14.72857438083221027, -4.937295716523431466, 2.501304222021813128 ) ) ;
#5146 = DIRECTION ( 'NONE',  ( 1.000000000000000000, 0.000000000000000000, 0.000000000000000000 ) ) ;
#5145 = CARTESIAN_POINT ( 'NONE',  ( -60.75950795826495465, 23.17721540975219696, 15.50000000000000000 ) ) ;
#5147 = EDGE_LOOP ( 'NONE', ( #39421, #20925, #29885, #31121 ) ) ;
#5148 = CARTESIAN_POINT ( 'NONE',  ( 23.17090746384732824, 3.812297950970844784, 3.383282008515589911 ) ) ;
#5149 = CARTESIAN_POINT ( 'NONE',  ( 79.53094818655489462, 66.25005786596102553, -1.601045042264588325 ) ) ;
#5150 = CARTESIAN_POINT ( 'NONE',  ( 1.700390093233090871, -29.56993018339339940, 7.800000000000000711 ) ) ;
#5151 = ORIENTED_EDGE ( 'NONE', *, *, #14720, .F. ) ;
#5152 = B_SPLINE_CURVE_WITH_KNOTS ( 'NONE', 3,
 ( #37722, #35090, #28888, #696, #31374, #22522, #13428, #12623, #35288, #6864, #15717, #497, #34890, #22114, #9939, #31781, #3596, #3201, #7056, #34479, #16121, #28269, #91 ),
 .UNSPECIFIED., .F., .F.,
 ( 4, 1, 1, 1, 1, 1, 1, 2, 2, 1, 1, 1, 1, 1, 2, 2, 4 ),
 ( 0.000000000000000000, 0.1249999999999883982, 0.1874999999999822364, 0.2187499999999795997, 0.2343749999999782674, 0.2421874999999781286, 0.2460937499999785449, 0.2480468749999787670, 0.2499999999999789613, 0.3749999999999901745, 0.4374999999999960032, 0.4687499999999989453, 0.4843750000000004996, 0.4921875000000016653, 0.4960937500000021649, 0.5000000000000026645, 1.000000000000000000 ),
 .UNSPECIFIED. ) ;
#5154 = CARTESIAN_POINT ( 'NONE',  ( 30.19238557334687911, -2.952639005720375742, -4.918649992961978690 ) ) ;
#5153 = CARTESIAN_POINT ( 'NONE',  ( -0.02954803322811855662, -26.64293167151592456, 7.712764235869101093 ) ) ;
#5155 = DIRECTION ( 'NONE',  ( 1.000000000000000000, 0.000000000000000000, 0.000000000000000000 ) ) ;
#5156 = CARTESIAN_POINT ( 'NONE',  ( 75.35164290873603932, 61.82650661013094862, 3.882889210543307268 ) ) ;
#5157 = VERTEX_POINT ( 'NONE', #9427 ) ;
#5158 = CARTESIAN_POINT ( 'NONE',  ( 23.15855103537317206, 2.689427168583138350, -4.343935680606369587 ) ) ;
#5159 = ORIENTED_EDGE ( 'NONE', *, *, #33812, .T. ) ;
#5160 = DIRECTION ( 'NONE',  ( 0.000000000000000000, 1.000000000000000000, 0.000000000000000000 ) ) ;
#5161 = CARTESIAN_POINT ( 'NONE',  ( 6.019945922396399141, -27.01350538757900210, 7.695279973900954751 ) ) ;
#5162 = LINE ( 'NONE', #17699, #664 ) ;
#5163 = DIRECTION ( 'NONE',  ( -0.000000000000000000, -0.000000000000000000, 1.000000000000000000 ) ) ;
#5164 = CARTESIAN_POINT ( 'NONE',  ( -65.27430759792673598, 36.41843883184812114, 8.800656633793924044 ) ) ;
#5165 = CARTESIAN_POINT ( 'NONE',  ( 81.84810375386635428, 62.06244373962204008, 1.965143080302226508 ) ) ;
#5166 = CARTESIAN_POINT ( 'NONE',  ( 87.09859342968812257, 0.5244505078549105415, -5.068689133590885909 ) ) ;
#5167 = CARTESIAN_POINT ( 'NONE',  ( 30.13988473044573624, 0.1694294105150049301, -5.382122866902316893 ) ) ;
#5168 = DIRECTION ( 'NONE',  ( 0.000000000000000000, 0.000000000000000000, 1.000000000000000000 ) ) ;
#5169 = ADVANCED_FACE ( 'NONE', ( #31894 ), #26335, .T. ) ;
#5170 = EDGE_CURVE ( 'NONE', #10250, #36751, #27655, .T. ) ;
#5171 = CARTESIAN_POINT ( 'NONE',  ( -78.80630328534653017, -5.372281114570830240, -7.948834340388816422 ) ) ;
#5172 = ORIENTED_EDGE ( 'NONE', *, *, #30683, .F. ) ;
#5173 = CARTESIAN_POINT ( 'NONE',  ( 28.89721236653044301, -3.425550027173258627, 4.559861221518604957 ) ) ;
#5174 = FACE_OUTER_BOUND ( 'NONE', #15524, .T. ) ;
#5175 = EDGE_CURVE ( 'NONE', #5140, #23918, #36779, .T. ) ;
#5176 = CARTESIAN_POINT ( 'NONE',  ( 34.36133827824247078, -1.406879114103402273, -5.569315889062961489 ) ) ;
#5177 = CARTESIAN_POINT ( 'NONE',  ( -36.87867591359218977, -26.64985754041175525, 6.800000000000000711 ) ) ;
#5178 = CARTESIAN_POINT ( 'NONE',  ( 5.194214398482093209, -29.67280000852606392, 7.771081512783709400 ) ) ;
#5179 = DIRECTION ( 'NONE',  ( 0.000000000000000000, 0.000000000000000000, 1.000000000000000000 ) ) ;
#5180 = CARTESIAN_POINT ( 'NONE',  ( 0.05942261555421801678, -26.47845355906757447, 7.751599049952173637 ) ) ;
#5181 = CARTESIAN_POINT ( 'NONE',  ( 3.651251297819360531, -26.64985754041175525, 6.700000000000000178 ) ) ;
#5182 = ORIENTED_EDGE ( 'NONE', *, *, #28685, .F. ) ;
#5183 = CARTESIAN_POINT ( 'NONE',  ( 36.96501263788630354, -2.310926168294844985, 5.934243022296812775 ) ) ;
#5184 = CARTESIAN_POINT ( 'NONE',  ( 3.293813124479239018, -32.57342865076346783, 7.754798119455333705 ) ) ;
#5185 = CARTESIAN_POINT ( 'NONE',  ( 66.84954949145740954, 57.97782447864501165, -3.999382933223863734 ) ) ;
#5186 = VECTOR ( 'NONE', #37937, 1000.000000000000114 ) ;
#5187 = CARTESIAN_POINT ( 'NONE',  ( -2.485163400083383323, -30.43163963246801984, 7.754798119455333705 ) ) ;
#5188 = ORIENTED_EDGE ( 'NONE', *, *, #34210, .T. ) ;
#5189 = CARTESIAN_POINT ( 'NONE',  ( 0.000000000000000000, 0.000000000000000000, 2.500000000000000000 ) ) ;
#5190 = CARTESIAN_POINT ( 'NONE',  ( 3.890029461744421102, -32.17099692592865523, 7.763628509615289275 ) ) ;
#5191 = DIRECTION ( 'NONE',  ( 0.000000000000000000, 1.000000000000000000, 0.000000000000000000 ) ) ;
#5192 = CARTESIAN_POINT ( 'NONE',  ( -75.60183227957097074, 10.11098911773139442, 8.848339649221273362 ) ) ;
#5193 = CARTESIAN_POINT ( 'NONE',  ( -70.92837670882107659, -23.80776546975053165, 0.000000000000000000 ) ) ;
#5194 = CARTESIAN_POINT ( 'NONE',  ( 1.260455253761291861, -26.09768921580216627, 6.895394898881670898 ) ) ;
#5195 = ORIENTED_EDGE ( 'NONE', *, *, #10863, .T. ) ;
#5196 = CARTESIAN_POINT ( 'NONE',  ( 22.87897072576537738, 4.322970251960089882, 3.079858772812353429 ) ) ;
#5197 = CARTESIAN_POINT ( 'NONE',  ( 80.38645948019593845, 66.31981033314001195, -1.103079483641125069 ) ) ;
#5198 = CARTESIAN_POINT ( 'NONE',  ( 79.38068533922456993, 65.45287079212486958, 2.940771700540096401 ) ) ;
#5199 = VECTOR ( 'NONE', #12699, 1000.000000000000000 ) ;
#5200 = CARTESIAN_POINT ( 'NONE',  ( -0.1757080581666877195, -32.40546732307887368, 6.979335674598003969 ) ) ;
#5201 = VERTEX_POINT ( 'NONE', #32962 ) ;
#5202 = CARTESIAN_POINT ( 'NONE',  ( 77.83481221125377658, 64.51125116100624268, -3.218236826935536588 ) ) ;
#5204 = CARTESIAN_POINT ( 'NONE',  ( 1.105923466014343548, -33.01907637181788147, 7.635761828346575797 ) ) ;
#5203 = CARTESIAN_POINT ( 'NONE',  ( 22.29360747402898824, 0.2601931310903464190, 7.110083990419366451 ) ) ;
#5205 = CARTESIAN_POINT ( 'NONE',  ( 81.25398435008909814, 63.24110186484434593, -3.279590910092189393 ) ) ;
#5206 = CARTESIAN_POINT ( 'NONE',  ( -0.6444488087166562185, -32.16833941288422238, 7.750000000000000888 ) ) ;
#5207 = CARTESIAN_POINT ( 'NONE',  ( 78.95981124517781780, 62.31610944509175454, 3.691425412862327171 ) ) ;
#5208 = VERTEX_POINT ( 'NONE', #4749 ) ;
#5209 = CARTESIAN_POINT ( 'NONE',  ( 35.37144363141613468, -3.783876837969972762, -5.514777695184551298 ) ) ;
#5210 = CARTESIAN_POINT ( 'NONE',  ( 79.31644831670718077, 66.29498274501730748, 1.214491505233689983 ) ) ;
#5212 = CARTESIAN_POINT ( 'NONE',  ( 10.50357756723356140, 59.39757829809867928, 4.000000000000000000 ) ) ;
#5211 = CARTESIAN_POINT ( 'NONE',  ( 0.000000000000000000, 0.000000000000000000, -2.500000000000000000 ) ) ;
#5213 = CARTESIAN_POINT ( 'NONE',  ( 30.13146195922598380, -4.635528103762326602, -0.9093114724505712010 ) ) ;
#5214 = LINE ( 'NONE', #3185, #22783 ) ;
#5215 = CARTESIAN_POINT ( 'NONE',  ( -1.534173489221649866, -30.61759350290857284, 7.754798119455333705 ) ) ;
#5216 = EDGE_LOOP ( 'NONE', ( #17746, #27735, #38508, #30579 ) ) ;
#5217 = DIRECTION ( 'NONE',  ( 1.000000000000000000, 0.000000000000000000, 0.000000000000000000 ) ) ;
#5218 = CARTESIAN_POINT ( 'NONE',  ( 27.42305978988358461, 1.006780081163760610, -4.486390501344786230 ) ) ;
#5219 = AXIS2_PLACEMENT_3D ( 'NONE', #28928, #16551, #25632 ) ;
#5220 = DIRECTION ( 'NONE',  ( -0.000000000000000000, -0.000000000000000000, -1.000000000000000000 ) ) ;
#5221 = LINE ( 'NONE', #8904, #5314 ) ;
#5222 = CARTESIAN_POINT ( 'NONE',  ( -1.057258846844102873, -31.72486802769777725, 7.754798119455333705 ) ) ;
#5223 = ADVANCED_FACE ( 'NONE', ( #38512 ), #10912, .F. ) ;
#5224 = DIRECTION ( 'NONE',  ( 0.000000000000000000, 0.000000000000000000, 1.000000000000000000 ) ) ;
#5225 = CARTESIAN_POINT ( 'NONE',  ( 36.68443910100898364, -1.916675254377900872, -5.804134546349906998 ) ) ;
#5226 = CARTESIAN_POINT ( 'NONE',  ( 3.369241353962452390, -26.60767842677951833, 7.691066658568955106 ) ) ;
#5227 = PLANE ( 'NONE',  #5811 ) ;
#5228 = LINE ( 'NONE', #35283, #20001 ) ;
#5229 = CARTESIAN_POINT ( 'NONE',  ( -71.84395654979768153, -48.30921343784671507, 5.930300998046988958 ) ) ;
#5230 = DIRECTION ( 'NONE',  ( 0.000000000000000000, 0.000000000000000000, 1.000000000000000000 ) ) ;
#5231 = CARTESIAN_POINT ( 'NONE',  ( 5.095583499898731716, -29.75083557328108697, 6.887945620086122211 ) ) ;
#5232 = CARTESIAN_POINT ( 'NONE',  ( 5.021324086407805254, -24.55319635012989110, 6.700000000000000178 ) ) ;
#5233 = CARTESIAN_POINT ( 'NONE',  ( 24.22011166491034473, 2.157244859911064960, -4.307574350163300814 ) ) ;
#5234 = VECTOR ( 'NONE', #26582, 1000.000000000000000 ) ;
#5235 = CARTESIAN_POINT ( 'NONE',  ( 66.42792150476880408, 57.77419247997864460, 4.000000000000008882 ) ) ;
#5236 = CARTESIAN_POINT ( 'NONE',  ( 72.66268786488812736, 61.76016136843576021, -3.552420216958366517 ) ) ;
#5237 = VERTEX_POINT ( 'NONE', #32367 ) ;
#5238 = PLANE ( 'NONE',  #14687 ) ;
#5239 = CARTESIAN_POINT ( 'NONE',  ( -63.08758708074093136, 36.14363715547679590, 3.800414904976364472 ) ) ;
#5240 = CARTESIAN_POINT ( 'NONE',  ( 3.031610088737084041, -26.44136528038649203, 6.887945620086121323 ) ) ;
#5241 = CARTESIAN_POINT ( 'NONE',  ( 3.300000000000000266, 2.500000000000000000, 0.000000000000000000 ) ) ;
#5242 = ADVANCED_FACE ( 'NONE', ( #32173 ), #32570, .F. ) ;
#5243 = CARTESIAN_POINT ( 'NONE',  ( -18.87867591359219333, -24.55319635012989110, 6.700000000000000178 ) ) ;
#5244 = VERTEX_POINT ( 'NONE', #23680 ) ;
#5245 = DIRECTION ( 'NONE',  ( 1.224646799147353207E-16, 1.000000000000000000, -0.000000000000000000 ) ) ;
#5246 = CIRCLE ( 'NONE', #34197, 12.80480339192541628 ) ;
#5247 =( NAMED_UNIT ( * ) SI_UNIT ( $, .STERADIAN. ) SOLID_ANGLE_UNIT ( ) );
#5248 = ORIENTED_EDGE ( 'NONE', *, *, #9010, .F. ) ;
#5249 = ORIENTED_EDGE ( 'NONE', *, *, #35976, .F. ) ;
#5250 = CARTESIAN_POINT ( 'NONE',  ( 79.70629046221083058, 63.56464109829104814, -3.738478073092015297 ) ) ;
#5251 = CARTESIAN_POINT ( 'NONE',  ( 16.63788139911590847, 9.878167360688344445, -2.500000000000113243 ) ) ;
#5252 = CARTESIAN_POINT ( 'NONE',  ( 81.24504193829289989, 64.75648403698978939, -3.071899782094857478 ) ) ;
#5253 = CARTESIAN_POINT ( 'NONE',  ( 80.75607764207482830, 61.50646045904602488, 2.414331286641654195 ) ) ;
#5254 = DIRECTION ( 'NONE',  ( -1.000000000000000000, 0.000000000000000000, 0.000000000000000000 ) ) ;
#5255 = VECTOR ( 'NONE', #6690, 1000.000000000000000 ) ;
#5256 = CARTESIAN_POINT ( 'NONE',  ( 15.61831370365439930, 11.17526387718623582, -2.611274213471738825 ) ) ;
#5257 = DIRECTION ( 'NONE',  ( 0.000000000000000000, 0.000000000000000000, 1.000000000000000000 ) ) ;
#5258 = CARTESIAN_POINT ( 'NONE',  ( 21.85643539959777826, -11.73360331217645225, -7.400322805736739618 ) ) ;
#5259 = ORIENTED_EDGE ( 'NONE', *, *, #2873, .F. ) ;
#5260 = DIRECTION ( 'NONE',  ( -0.000000000000000000, -0.000000000000000000, -1.000000000000000000 ) ) ;
#5261 = DIRECTION ( 'NONE',  ( 1.000000000000000000, 0.000000000000000000, 0.000000000000000000 ) ) ;
#5262 = CARTESIAN_POINT ( 'NONE',  ( -73.66622939153592142, 5.992931831121631525, -9.675836161015377357 ) ) ;
#5263 = ADVANCED_FACE ( 'NONE', ( #16491 ), #4366, .F. ) ;
#5264 = CARTESIAN_POINT ( 'NONE',  ( 1.497294612651186796, -32.96385891360668552, 6.988553391373221402 ) ) ;
#5265 = DIRECTION ( 'NONE',  ( 1.000000000000000000, 0.000000000000000000, -0.000000000000000000 ) ) ;
#5266 = CARTESIAN_POINT ( 'NONE',  ( -1.534173489221649866, -30.61759350290857284, 7.754798119455333705 ) ) ;
#5267 = CARTESIAN_POINT ( 'NONE',  ( 3.972827115442711055, -27.04089282105746861, 7.761597726988854973 ) ) ;
#5268 = DIRECTION ( 'NONE',  ( 1.000000000000000000, 0.000000000000000000, 0.000000000000000000 ) ) ;
#5269 = CARTESIAN_POINT ( 'NONE',  ( 0.6655969032795109319, -26.22639806170147025, 7.011627023500184741 ) ) ;
#5270 = DIRECTION ( 'NONE',  ( 1.000000000000000000, 0.000000000000000000, 0.000000000000000000 ) ) ;
#5271 = AXIS2_PLACEMENT_3D ( 'NONE', #34935, #6512, #136 ) ;
#5272 = CARTESIAN_POINT ( 'NONE',  ( -64.58659014339545479, 34.69724588627169481, 5.982304021381975367 ) ) ;
#5273 = CARTESIAN_POINT ( 'NONE',  ( -0.4281225035922071043, -26.91860427732644467, 6.874555630061442102 ) ) ;
#5274 = FACE_OUTER_BOUND ( 'NONE', #27150, .T. ) ;
#5275 = ORIENTED_EDGE ( 'NONE', *, *, #7116, .F. ) ;
#5276 =( BOUNDED_CURVE ( )  B_SPLINE_CURVE ( 3, ( #17440, #27341, #39901, #11675 ),
 .UNSPECIFIED., .F., .T. ) 
 B_SPLINE_CURVE_WITH_KNOTS ( ( 4, 4 ),
 ( 1.347909859412854905, 1.534781240595299412 ),
 .UNSPECIFIED. ) 
 CURVE ( )  GEOMETRIC_REPRESENTATION_ITEM ( )  RATIONAL_B_SPLINE_CURVE ( ( 1.000000000000000000, 0.9970920404276226723, 0.9970920404276226723, 1.000000000000000000 ) ) 
 REPRESENTATION_ITEM ( '' )  );
#5277 = CARTESIAN_POINT ( 'NONE',  ( -69.47640242684072120, -47.50614603290127036, 5.821697485475862521 ) ) ;
#5278 = CARTESIAN_POINT ( 'NONE',  ( 67.93540907064681278, 58.63163702635943508, 3.982418445723137967 ) ) ;
#5279 = CARTESIAN_POINT ( 'NONE',  ( 32.78150442608843207, -0.9262738374823473730, 5.322744608008340705 ) ) ;
#5280 = ADVANCED_FACE ( 'NONE', ( #13405 ), #25979, .F. ) ;
#5281 = ORIENTED_EDGE ( 'NONE', *, *, #38674, .T. ) ;
#5282 = CYLINDRICAL_SURFACE ( 'NONE', #6961, 0.09010775117052866046 ) ;
#5283 = CARTESIAN_POINT ( 'NONE',  ( 85.86339947292255204, 1.596523033150343718, -5.427711696011725984 ) ) ;
#5284 = AXIS2_PLACEMENT_3D ( 'NONE', #26803, #7453, #10729 ) ;
#5286 = CARTESIAN_POINT ( 'NONE',  ( 4.842674212786914900, -30.86841026102256791, 6.868387053540519815 ) ) ;
#5285 = CARTESIAN_POINT ( 'NONE',  ( 33.89705139301766224, -5.463269898809035574, -0.9834710557593000502 ) ) ;
#5287 = CARTESIAN_POINT ( 'NONE',  ( -1.628373570674043425, -28.87751162402568639, 6.864651958020304257 ) ) ;
#5288 = CARTESIAN_POINT ( 'NONE',  ( 85.80507661318331714, 1.187011356922548666, 5.731706916149471809 ) ) ;
#5289 = CARTESIAN_POINT ( 'NONE',  ( -0.6209176402083074198, -32.18940249604951731, 6.863805608295729499 ) ) ;
#5290 = ORIENTED_EDGE ( 'NONE', *, *, #21307, .T. ) ;
#5291 = DIRECTION ( 'NONE',  ( -0.000000000000000000, -0.000000000000000000, 1.000000000000000000 ) ) ;
#5292 = CARTESIAN_POINT ( 'NONE',  ( 80.45282402617027628, 62.88786617374236698, -3.531602295408444281 ) ) ;
#5293 = ADVANCED_FACE ( 'NONE', ( #26384 ), #38222, .T. ) ;
#5294 = CARTESIAN_POINT ( 'NONE',  ( -1.524383821632846470, -28.20947427840861366, 7.006248344249653037 ) ) ;
#5295 = ADVANCED_FACE ( 'NONE', ( #10513 ), #23093, .F. ) ;
#5296 = CARTESIAN_POINT ( 'NONE',  ( 81.06761308752996342, 61.31222891353765192, 1.660510093083209737 ) ) ;
#5297 = CARTESIAN_POINT ( 'NONE',  ( 22.33770448043473777, 0.2832778397994459296, 7.020340292902776724 ) ) ;
#5299 = VERTEX_POINT ( 'NONE', #29659 ) ;
#5298 = CARTESIAN_POINT ( 'NONE',  ( 4.777565610504584726, -27.91210591261665641, 7.771081512783700518 ) ) ;
#5300 = ADVANCED_FACE ( 'NONE', ( #1472 ), #14005, .F. ) ;
#5301 = CIRCLE ( 'NONE', #28319, 0.1000000000000028644 ) ;
#5302 = CARTESIAN_POINT ( 'NONE',  ( 74.23991766213896426, 61.26593220986219279, -3.911020515999897640 ) ) ;
#5303 = B_SPLINE_CURVE_WITH_KNOTS ( 'NONE', 3,
 ( #23243, #25931, #4899, #13964, #10664, #26733, #35613, #1624, #26341, #17430, #4705, #14159, #26137, #39270, #20141, #7384, #26530, #11062, #17036 ),
 .UNSPECIFIED., .F., .F.,
 ( 4, 3, 3, 3, 3, 3, 4 ),
 ( 0.000000000000000000, 2.546128104244995842E-05, 5.711050680484009269E-05, 8.113074941675803807E-05, 0.0001053129305727061295, 0.0001360598016347041260, 0.0001612931755702019473 ),
 .UNSPECIFIED. ) ;
#5304 = CARTESIAN_POINT ( 'NONE',  ( -70.05487543777402948, -21.28726014413347656, 5.936291904728155266 ) ) ;
#5306 = CARTESIAN_POINT ( 'NONE',  ( 14.77315594796471743, 13.19392823276620419, 2.499999999999996891 ) ) ;
#5305 = DIRECTION ( 'NONE',  ( -1.000000000000000000, 0.000000000000000000, 0.000000000000000000 ) ) ;
#5307 = CARTESIAN_POINT ( 'NONE',  ( -1.084049423045779115, -33.98664651305095674, 6.954324564059724878 ) ) ;
#5308 = B_SPLINE_CURVE_WITH_KNOTS ( 'NONE', 3,
 ( #15983, #25060, #28550, #2848, #15581, #361, #6120, #9192, #12898, #38008, #28135, #25266, #18654 ),
 .UNSPECIFIED., .F., .F.,
 ( 4, 3, 3, 3, 4 ),
 ( 0.0002056071264154448830, 0.0002117781465860642546, 0.0002420274594459682145, 0.0002722905548971127528, 0.0002816827545175561317 ),
 .UNSPECIFIED. ) ;
#5309 = LINE ( 'NONE', #27326, #11344 ) ;
#5310 = CARTESIAN_POINT ( 'NONE',  ( 22.63677108660874637, 4.537383518013977657, -3.128882317202244856 ) ) ;
#5311 = VERTEX_POINT ( 'NONE', #14408 ) ;
#5312 = CARTESIAN_POINT ( 'NONE',  ( -4.448748702180642667, -26.64985754041175525, 6.700000000000000178 ) ) ;
#5313 = CARTESIAN_POINT ( 'NONE',  ( 23.92064240948634790, 4.179079982057642972, -0.5982227118658990372 ) ) ;
#5314 = VECTOR ( 'NONE', #24355, 1000.000000000000000 ) ;
#5315 = CARTESIAN_POINT ( 'NONE',  ( -8.248748702180632719, -26.64985754041175525, 6.800000000000000711 ) ) ;
#5316 = ADVANCED_FACE ( 'NONE', ( #21211 ), #12126, .T. ) ;
#5317 = VERTEX_POINT ( 'NONE', #21005 ) ;
#5318 = CARTESIAN_POINT ( 'NONE',  ( 4.984671627384348547, -28.36018029005467866, 7.635761828346577573 ) ) ;
#5319 = CARTESIAN_POINT ( 'NONE',  ( 80.84588251005118309, 64.54609234697676357, 3.375310687858769310 ) ) ;
#5320 = CARTESIAN_POINT ( 'NONE',  ( 84.60690941119878516, 3.085063967761199066, 1.108375916024202379 ) ) ;
#5321 = CARTESIAN_POINT ( 'NONE',  ( -18.87867591359219333, -26.64985754041175525, 6.700000000000000178 ) ) ;
#5322 = ORIENTED_EDGE ( 'NONE', *, *, #4069, .T. ) ;
#5323 = DIRECTION ( 'NONE',  ( -0.000000000000000000, 0.000000000000000000, 1.000000000000000000 ) ) ;
#5324 = CARTESIAN_POINT ( 'NONE',  ( -0.000000000000000000, 10.37661300689600097, -6.000000000000000000 ) ) ;
#5325 = CARTESIAN_POINT ( 'NONE',  ( 19.68021815578885736, -2.835469129926569742, -3.275245259520223939 ) ) ;
#5326 = DIRECTION ( 'NONE',  ( -0.000000000000000000, -0.000000000000000000, -1.000000000000000000 ) ) ;
#5327 = FACE_OUTER_BOUND ( 'NONE', #24655, .T. ) ;
#5328 = CARTESIAN_POINT ( 'NONE',  ( 23.09295755050888843, 0.3657069220331809478, -5.919601208922279589 ) ) ;
#5329 = CARTESIAN_POINT ( 'NONE',  ( -0.4693117693055204320, -26.95220437874807118, 7.779495906702012853 ) ) ;
#5330 = ORIENTED_EDGE ( 'NONE', *, *, #24841, .F. ) ;
#5331 = CARTESIAN_POINT ( 'NONE',  ( 35.78599988003760757, -3.160010335899736678, 5.791668787594319134 ) ) ;
#5332 = AXIS2_PLACEMENT_3D ( 'NONE', #5211, #16787, #36503 ) ;
#5333 = CARTESIAN_POINT ( 'NONE',  ( 87.18327248044521127, 0.4293349789342923994, 4.780712506200352152 ) ) ;
#5334 = EDGE_LOOP ( 'NONE', ( #5182, #27575, #7327, #28510 ) ) ;
#5335 = ORIENTED_EDGE ( 'NONE', *, *, #30710, .T. ) ;
#5337 = CARTESIAN_POINT ( 'NONE',  ( 36.20129013013437458, -3.652211045159744707, 5.717050583165211641 ) ) ;
#5336 = CARTESIAN_POINT ( 'NONE',  ( 78.78605531729427014, 66.08782950793384714, -1.450104216466339802 ) ) ;
#5338 = DIRECTION ( 'NONE',  ( -0.000000000000000000, -0.000000000000000000, -1.000000000000000000 ) ) ;
#5339 = CARTESIAN_POINT ( 'NONE',  ( 17.38677253544971890, -3.246026456844883334, -2.884626868749156969 ) ) ;
#5340 = DIRECTION ( 'NONE',  ( -1.000000000000000000, 0.000000000000000000, 0.000000000000000000 ) ) ;
#5341 = ORIENTED_EDGE ( 'NONE', *, *, #26282, .F. ) ;
#5342 = CARTESIAN_POINT ( 'NONE',  ( -0.09519644969557856939, -26.55769863645182483, 7.255881584735164758 ) ) ;
#5343 = VERTEX_POINT ( 'NONE', #11919 ) ;
#5344 = EDGE_CURVE ( 'NONE', #21663, #16587, #20465, .T. ) ;
#5345 = AXIS2_PLACEMENT_3D ( 'NONE', #12105, #14386, #5136 ) ;
#5346 = ORIENTED_EDGE ( 'NONE', *, *, #39305, .F. ) ;
#5347 = CARTESIAN_POINT ( 'NONE',  ( 0.03159606602598123704, -32.53221418380139340, 7.692469944509198854 ) ) ;
#5348 = CARTESIAN_POINT ( 'NONE',  ( 80.60461247708464327, 63.28149962716670984, -3.592474444481850604 ) ) ;
#5349 = CARTESIAN_POINT ( 'NONE',  ( -58.98400447371446376, 28.74159977738611715, -6.613141227606677219 ) ) ;
#5350 = VERTEX_POINT ( 'NONE', #11713 ) ;
#5351 = CARTESIAN_POINT ( 'NONE',  ( 4.281682929012584182, -27.35702998321412593, 7.695279973900954751 ) ) ;
#5352 = ORIENTED_EDGE ( 'NONE', *, *, #4167, .T. ) ;
#5353 = CARTESIAN_POINT ( 'NONE',  ( 23.65230220904194525, 3.215211265575084187, 3.706123801245496008 ) ) ;
#5354 = EDGE_CURVE ( 'NONE', #20784, #5955, #9486, .T. ) ;
#5355 = CARTESIAN_POINT ( 'NONE',  ( 82.04158296082394486, 62.38656886254256051, -2.040045296073659920 ) ) ;
#5356 = LINE ( 'NONE', #12122, #16059 ) ;
#5357 = EDGE_LOOP ( 'NONE', ( #19533, #37436, #32519, #36112 ) ) ;
#5359 = CARTESIAN_POINT ( 'NONE',  ( 1.074641032650325734, -26.22800886213295968, 7.692469944509198854 ) ) ;
#5358 = DIRECTION ( 'NONE',  ( -0.000000000000000000, 1.000000000000000000, -0.000000000000000000 ) ) ;
#5360 = PLANE ( 'NONE',  #7338 ) ;
#5361 = CARTESIAN_POINT ( 'NONE',  ( 74.72764284544139457, 63.14151651683601330, 3.204585025132375975 ) ) ;
#5362 = CARTESIAN_POINT ( 'NONE',  ( 24.16851685081003254, 2.882859430398138301, -3.821847350340896288 ) ) ;
#5363 = ORIENTED_EDGE ( 'NONE', *, *, #1726, .T. ) ;
#5364 = CYLINDRICAL_SURFACE ( 'NONE', #37247, 12.73502530973474123 ) ;
#5365 = DIRECTION ( 'NONE',  ( 0.000000000000000000, 0.000000000000000000, -1.000000000000000000 ) ) ;
#5366 = ORIENTED_EDGE ( 'NONE', *, *, #5820, .T. ) ;
#5367 = CYLINDRICAL_SURFACE ( 'NONE', #17531, 0.09010775117052900740 ) ;
#5368 = CARTESIAN_POINT ( 'NONE',  ( 81.92776049059212085, 62.60942412355771580, 2.397965335136732712 ) ) ;
#5369 = CARTESIAN_POINT ( 'NONE',  ( 85.29288036551089647, 2.552713125850948117, 2.517437320556888736 ) ) ;
#5370 = CARTESIAN_POINT ( 'NONE',  ( 5.138907313317528924, -30.22313780932130456, 6.880608371227949327 ) ) ;
#5371 = CARTESIAN_POINT ( 'NONE',  ( 2.817966617839567700, -32.88670914974743198, 6.865554069792297653 ) ) ;
#5372 = ORIENTED_EDGE ( 'NONE', *, *, #26630, .F. ) ;
#5373 = CARTESIAN_POINT ( 'NONE',  ( 1.700390093233090871, -29.56993018339339940, 2.499999999999998668 ) ) ;
#5374 = CARTESIAN_POINT ( 'NONE',  ( 0.09941021755798716553, -26.45755754540749649, 6.895394898881670898 ) ) ;
#5375 = VECTOR ( 'NONE', #10061, 1000.000000000000000 ) ;
#5376 = CARTESIAN_POINT ( 'NONE',  ( 35.33511153101647295, -3.174037457546911689, -5.721296755953630964 ) ) ;
#5377 = DIRECTION ( 'NONE',  ( -1.000000000000000000, 0.000000000000000000, 0.000000000000000000 ) ) ;
#5378 = DIRECTION ( 'NONE',  ( 1.000000000000000000, 0.000000000000000000, 0.000000000000000000 ) ) ;
#5379 = LINE ( 'NONE', #8856, #5964 ) ;
#5380 = CARTESIAN_POINT ( 'NONE',  ( -72.95330471031414277, 33.71485196875532608, -46.17089178453873188 ) ) ;
#5381 = EDGE_CURVE ( 'NONE', #5651, #5955, #33386, .T. ) ;
#5382 = DIRECTION ( 'NONE',  ( 0.000000000000000000, 0.000000000000000000, 1.000000000000000000 ) ) ;
#5383 = ORIENTED_EDGE ( 'NONE', *, *, #22574, .F. ) ;
#5384 = CARTESIAN_POINT ( 'NONE',  ( 36.19298715789191334, -3.601780938441950575, 5.745406905112727891 ) ) ;
#5385 = CARTESIAN_POINT ( 'NONE',  ( -71.92602134074772380, -0.7038144147489171498, 3.916479336966925295 ) ) ;
#5386 = CARTESIAN_POINT ( 'NONE',  ( 66.88099813915303571, 57.89052526007606758, -3.999029912548879739 ) ) ;
#5387 = EDGE_CURVE ( 'NONE', #35810, #38896, #5768, .T. ) ;
#5388 = DIRECTION ( 'NONE',  ( 0.000000000000000000, -0.000000000000000000, 1.000000000000000000 ) ) ;
#5389 = VERTEX_POINT ( 'NONE', #30071 ) ;
#5390 = CARTESIAN_POINT ( 'NONE',  ( -0.5758167276443872939, -25.38032712238630495, 6.954324564059724878 ) ) ;
#5391 = EDGE_CURVE ( 'NONE', #11501, #26758, #2101, .T. ) ;
#5392 = CARTESIAN_POINT ( 'NONE',  ( -18.44874870218064089, -25.49307895267003587, 6.700000000000000178 ) ) ;
#5393 = CARTESIAN_POINT ( 'NONE',  ( 14.84235502726276934, 12.12055237356136139, 2.522906484353911960 ) ) ;
#5394 = CARTESIAN_POINT ( 'NONE',  ( -77.19718645414111791, 10.97120867451975279, 7.801112875662933099 ) ) ;
#5395 = DIRECTION ( 'NONE',  ( -0.000000000000000000, -0.000000000000000000, 1.000000000000000000 ) ) ;
#5396 = CARTESIAN_POINT ( 'NONE',  ( 1.282747240999764005, -26.09493745707318269, 6.951256099901592655 ) ) ;
#5397 = ORIENTED_EDGE ( 'NONE', *, *, #20884, .F. ) ;
#5398 = CARTESIAN_POINT ( 'NONE',  ( 22.88074270852006009, 4.309495562975050653, 3.097908743967009659 ) ) ;
#5399 = ADVANCED_FACE ( 'NONE', ( #17692, #30272 ), #5360, .T. ) ;
#5400 = CARTESIAN_POINT ( 'NONE',  ( 81.60972716517450465, 65.70321483603501633, -1.303631908149876617 ) ) ;
#5401 = CARTESIAN_POINT ( 'NONE',  ( 78.73074668855629454, 66.04592173387707987, 1.531260274641973895 ) ) ;
#5402 = EDGE_CURVE ( 'NONE', #40691, #2270, #39729, .T. ) ;
#5403 = DIRECTION ( 'NONE',  ( 1.000000000000000000, 5.786005779812646808E-17, 0.000000000000000000 ) ) ;
#5404 = ORIENTED_EDGE ( 'NONE', *, *, #32196, .T. ) ;
#5405 = CARTESIAN_POINT ( 'NONE',  ( 78.38159772055732333, 63.47233311668937006, -3.766285651913922283 ) ) ;
#5407 = CARTESIAN_POINT ( 'NONE',  ( 14.74007919223407370, -5.059642873582679279, -2.500266452831745312 ) ) ;
#5406 = CARTESIAN_POINT ( 'NONE',  ( 21.78353409329961465, 0.2137358133367803226, 8.397885858698352024 ) ) ;
#5408 = CARTESIAN_POINT ( 'NONE',  ( 81.39159673219582203, 61.52361671445444102, -1.704083397383978626 ) ) ;
#5409 = CARTESIAN_POINT ( 'NONE',  ( 79.17274970258583267, 61.87635977960864153, 3.505091495581067029 ) ) ;
#5410 = ORIENTED_EDGE ( 'NONE', *, *, #27668, .T. ) ;
#5411 = VECTOR ( 'NONE', #3353, 1000.000000000000000 ) ;
#5412 = ORIENTED_EDGE ( 'NONE', *, *, #754, .F. ) ;
#5413 = CARTESIAN_POINT ( 'NONE',  ( 36.28349705958110150, -3.620525866554765049, -5.741672296196851377 ) ) ;
#5414 = CARTESIAN_POINT ( 'NONE',  ( 82.46885687451873537, 64.22182207139040599, 1.617049763655828531 ) ) ;
#5416 = CARTESIAN_POINT ( 'NONE',  ( 87.04213330793392345, 0.5878691963682337596, -6.000000000000000000 ) ) ;
#5415 = CARTESIAN_POINT ( 'NONE',  ( 3.477536630118434058, -26.67135291403582187, 7.778050822775628426 ) ) ;
#5417 = CARTESIAN_POINT ( 'NONE',  ( 31.27801355750085222, -2.827678977088778911, 5.603419278764796729 ) ) ;
#5418 = CARTESIAN_POINT ( 'NONE',  ( -1.772036214352060046, -30.00840427972128666, 7.011627023500184741 ) ) ;
#5419 = LINE ( 'NONE', #11569, #13437 ) ;
#5420 = DIRECTION ( 'NONE',  ( 0.1736481776669333843, -0.9848077530122075762, 0.000000000000000000 ) ) ;
#5421 = CARTESIAN_POINT ( 'NONE',  ( 23.07493962920425190, 0.3584799070873228577, -5.937310339541745030 ) ) ;
#5422 = FACE_OUTER_BOUND ( 'NONE', #22342, .T. ) ;
#5423 = ORIENTED_EDGE ( 'NONE', *, *, #6943, .T. ) ;
#5424 = DIRECTION ( 'NONE',  ( -0.9267318687906771491, 0.3757233601570964532, 0.000000000000000000 ) ) ;
#5425 = DIRECTION ( 'NONE',  ( -0.000000000000000000, -0.000000000000000000, 1.000000000000000000 ) ) ;
#5426 = DIRECTION ( 'NONE',  ( -0.000000000000000000, 1.000000000000000000, -0.000000000000000000 ) ) ;
#5427 = CARTESIAN_POINT ( 'NONE',  ( 37.17546804304686248, -2.565784879737412982, -5.981171206039050503 ) ) ;
#5428 = CARTESIAN_POINT ( 'NONE',  ( -26.44874870218064089, -25.49307895267003587, 6.700000000000000178 ) ) ;
#5429 = DIRECTION ( 'NONE',  ( -1.000000000000000000, -3.568978458213368244E-15, 0.000000000000000000 ) ) ;
#5430 = FACE_OUTER_BOUND ( 'NONE', #25314, .T. ) ;
#5431 = DIRECTION ( 'NONE',  ( -0.8660254037844345998, -0.5000000000000071054, -0.000000000000000000 ) ) ;
#5432 = FACE_OUTER_BOUND ( 'NONE', #36298, .T. ) ;
#5433 = CARTESIAN_POINT ( 'NONE',  ( 5.096859737624582998, -29.72513773616743649, 6.871394612369937427 ) ) ;
#5434 = CARTESIAN_POINT ( 'NONE',  ( 0.9213240864078056092, -24.55319635012989110, 6.700000000000000178 ) ) ;
#5435 = DIRECTION ( 'NONE',  ( -0.000000000000000000, -1.000000000000000000, -0.000000000000000000 ) ) ;
#5436 = CARTESIAN_POINT ( 'NONE',  ( 24.70371381655884591, 2.049716166645646265, -4.246171004526042125 ) ) ;
#5437 = ORIENTED_EDGE ( 'NONE', *, *, #14775, .T. ) ;
#5438 = CARTESIAN_POINT ( 'NONE',  ( -70.73084030234451802, -48.60722628301608950, 5.997527803321491824 ) ) ;
#5439 = CARTESIAN_POINT ( 'NONE',  ( 66.41308122482404031, 57.81611748292269937, 4.000000000000022204 ) ) ;
#5440 = CARTESIAN_POINT ( 'NONE',  ( 68.97355662219305827, 59.39279559060015146, -3.921432738910643589 ) ) ;
#5441 = VECTOR ( 'NONE', #6477, 1000.000000000000000 ) ;
#5442 = DIRECTION ( 'NONE',  ( -0.000000000000000000, -0.000000000000000000, 1.000000000000000000 ) ) ;
#5443 = VERTEX_POINT ( 'NONE', #34202 ) ;
#5444 = CARTESIAN_POINT ( 'NONE',  ( 86.71282820137585645, -0.9518751250403653108, -5.452277641718156431 ) ) ;
#5445 = CARTESIAN_POINT ( 'NONE',  ( 0.1758335091890310398, -26.53089376604643590, 6.997764925645182821 ) ) ;
#5446 = CARTESIAN_POINT ( 'NONE',  ( -70.92837670882107659, -48.61702805680358352, 10.00000000000000888 ) ) ;
#5447 = CARTESIAN_POINT ( 'NONE',  ( 2.913702424011483938, -26.39378773199812400, 6.889465824494256374 ) ) ;
#5449 = CARTESIAN_POINT ( 'NONE',  ( 1.272770162583354514, -26.19691824104105748, 6.876076431790004051 ) ) ;
#5448 = CARTESIAN_POINT ( 'NONE',  ( -0.9508493577463464907, -27.28497717535191214, 6.880608371227950215 ) ) ;
#5450 = CONTEXT_DEPENDENT_SHAPE_REPRESENTATION ( #8154, #6250 ) ;
#5451 = CARTESIAN_POINT ( 'NONE',  ( -42.44874870218064444, -26.64985754041175525, 6.700000000000000178 ) ) ;
#5452 = VERTEX_POINT ( 'NONE', #15426 ) ;
#5453 = CARTESIAN_POINT ( 'NONE',  ( -32.34874870218063592, -25.49307895267003587, 6.700000000000000178 ) ) ;
#5454 = ADVANCED_FACE ( 'NONE', ( #28400 ), #34814, .F. ) ;
#5455 = LINE ( 'NONE', #17785, #26064 ) ;
#5456 = EDGE_CURVE ( 'NONE', #1177, #23554, #5970, .T. ) ;
#5457 = EDGE_LOOP ( 'NONE', ( #36330, #27625, #20881, #33478 ) ) ;
#5458 = CARTESIAN_POINT ( 'NONE',  ( 79.56639652130381535, 63.83553059081831549, -3.738478073092013076 ) ) ;
#5459 = CARTESIAN_POINT ( 'NONE',  ( 20.30405656617691434, 6.129814585338576371, -3.484773916750472100 ) ) ;
#5460 = CARTESIAN_POINT ( 'NONE',  ( 81.35720881915658254, 61.41209416231795615, -1.323744132979588928 ) ) ;
#5461 = CARTESIAN_POINT ( 'NONE',  ( 80.87678155331657592, 61.19751495238255501, 1.521414672925271772 ) ) ;
#5462 = EDGE_LOOP ( 'NONE', ( #30702, #33894, #15950, #21765 ) ) ;
#5463 = CARTESIAN_POINT ( 'NONE',  ( 22.77685072273605371, 3.733082073155330249, 3.761276434136069380 ) ) ;
#5464 = CARTESIAN_POINT ( 'NONE',  ( 18.67745381493141110, 13.05554818434302966, 2.500000000000000000 ) ) ;
#5465 = CARTESIAN_POINT ( 'NONE',  ( 21.85643539959777470, -5.354795180264900978, -13.61019886989645933 ) ) ;
#5466 = VERTEX_POINT ( 'NONE', #18935 ) ;
#5467 = CARTESIAN_POINT ( 'NONE',  ( -80.85729187619890013, 11.46329443280617788, 1.443597705564378053 ) ) ;
#5468 = AXIS2_PLACEMENT_3D ( 'NONE', #34692, #33867, #3203 ) ;
#5469 = CARTESIAN_POINT ( 'NONE',  ( -77.61396521033491069, 9.844637789582655785, -7.450128154136889336 ) ) ;
#5470 = FACE_OUTER_BOUND ( 'NONE', #35342, .T. ) ;
#5471 = CARTESIAN_POINT ( 'NONE',  ( 2.480576858534745188, -26.26064724879598344, 7.006423389747790331 ) ) ;
#5472 = LINE ( 'NONE', #12462, #20278 ) ;
#5473 = CARTESIAN_POINT ( 'NONE',  ( 14.65544684909820461, 12.77405410657241092, 2.493734942759960660 ) ) ;
#5474 = CARTESIAN_POINT ( 'NONE',  ( -0.03448549664302677509, -32.60970101154014600, 7.750000000000000000 ) ) ;
#5475 = CARTESIAN_POINT ( 'NONE',  ( -69.92837670882107659, -0.7829914368874778541, 9.949874371066204759 ) ) ;
#5476 = CARTESIAN_POINT ( 'NONE',  ( -69.32837670882108227, -31.30579396504363388, 1.870248747537495149E-15 ) ) ;
#5477 = VECTOR ( 'NONE', #38979, 1000.000000000000000 ) ;
#5478 = CARTESIAN_POINT ( 'NONE',  ( -56.59682361629209879, 30.63869417066593925, -3.015094993620159425 ) ) ;
#5479 = CARTESIAN_POINT ( 'NONE',  ( 87.33194808155565170, 0.2623354871973614388, 4.590518720782623241 ) ) ;
#5480 = CARTESIAN_POINT ( 'NONE',  ( 24.74244792756189426, 2.626221424013070571, -3.930118435553313638 ) ) ;
#5481 = ORIENTED_EDGE ( 'NONE', *, *, #22427, .F. ) ;
#5482 = VERTEX_POINT ( 'NONE', #21622 ) ;
#5483 = CARTESIAN_POINT ( 'NONE',  ( 67.91151009994659660, 58.69545974841741298, 3.974537232972598755 ) ) ;
#5484 = CARTESIAN_POINT ( 'NONE',  ( 36.44794194783038677, -2.352442707074569928, 5.894980856402876945 ) ) ;
#5485 = AXIS2_PLACEMENT_3D ( 'NONE', #5239, #29941, #8102 ) ;
#5486 = CARTESIAN_POINT ( 'NONE',  ( -16.34874870218063592, -26.64985754041175525, 6.800000000000000711 ) ) ;
#5487 = CARTESIAN_POINT ( 'NONE',  ( 87.83080901603209156, -0.9320485544948414747, 4.955211484752597428 ) ) ;
#5488 = CARTESIAN_POINT ( 'NONE',  ( 4.878343045835490166, -30.77848925561357873, 6.894806418505348589 ) ) ;
#5489 = CARTESIAN_POINT ( 'NONE',  ( 1.121324086407811338, -26.64985754041175525, 6.800000000000000711 ) ) ;
#5490 = DIRECTION ( 'NONE',  ( -0.000000000000000000, -0.000000000000000000, 1.000000000000000000 ) ) ;
#5491 = CARTESIAN_POINT ( 'NONE',  ( -0.6881146421603261398, -32.12826045096961991, 6.989977667959442975 ) ) ;
#5492 = VERTEX_POINT ( 'NONE', #35012 ) ;
#5493 = CARTESIAN_POINT ( 'NONE',  ( -70.03118149891237465, -21.22462562410226994, 5.944584973090443647 ) ) ;
#5494 = EDGE_CURVE ( 'NONE', #32500, #35091, #14, .T. ) ;
#5495 = EDGE_LOOP ( 'NONE', ( #9432, #29567, #37334, #13445 ) ) ;
#5496 = CARTESIAN_POINT ( 'NONE',  ( 79.61178798950636804, 64.58589821993882651, -3.525318766974264051 ) ) ;
#5497 = CARTESIAN_POINT ( 'NONE',  ( -1.549564175422862622, -28.27077767054321455, 6.864673517077424236 ) ) ;
#5498 = CARTESIAN_POINT ( 'NONE',  ( 80.80704226153167724, 62.39036624599375358, 3.220356845321973083 ) ) ;
#5499 = CARTESIAN_POINT ( 'NONE',  ( 22.66994700586167255, 0.3178347913156189253, 6.420626853764989761 ) ) ;
#5501 = ORIENTED_EDGE ( 'NONE', *, *, #33705, .F. ) ;
#5500 = CARTESIAN_POINT ( 'NONE',  ( -58.99948754145753327, 28.61410076184086293, 6.947368380125157117 ) ) ;
#5502 = AXIS2_PLACEMENT_3D ( 'NONE', #32883, #20106, #23207 ) ;
#5503 = CARTESIAN_POINT ( 'NONE',  ( 74.17630236427460488, 61.40657735673663353, -3.883841728571264529 ) ) ;
#5504 = CARTESIAN_POINT ( 'NONE',  ( 3.248497749708064486, -32.59703485353012553, 6.882085323592685988 ) ) ;
#5506 = DIRECTION ( 'NONE',  ( -1.000000000000000000, 0.000000000000000000, 0.000000000000000000 ) ) ;
#5505 = CARTESIAN_POINT ( 'NONE',  ( -63.99293516169446150, 35.89893413629672381, -46.17089178453873188 ) ) ;
#5507 = CARTESIAN_POINT ( 'NONE',  ( -63.99293516169446150, 35.89893413629672381, -7.506047544094577084 ) ) ;
#5508 = DIRECTION ( 'NONE',  ( -0.000000000000000000, -0.000000000000000000, 1.000000000000000000 ) ) ;
#5509 = CARTESIAN_POINT ( 'NONE',  ( -1.586485268957895434, -30.74699233443655544, 7.778495531946295394 ) ) ;
#5510 = CARTESIAN_POINT ( 'NONE',  ( 22.02803121022057198, 5.433847407666364759, -3.182498588599022238 ) ) ;
#5511 = ORIENTED_EDGE ( 'NONE', *, *, #20944, .F. ) ;
#5512 = PLANE ( 'NONE',  #32765 ) ;
#5513 = B_SPLINE_CURVE_WITH_KNOTS ( 'NONE', 3,
 ( #21854, #18752, #9478, #18966, #3752, #22681, #38296, #2942, #31530, #15458, #28018, #34430, #6209, #3153, #15668, #28216, #46, #12575, #13595, #25962, #32946, #35444, #7616, #32549, #4348, #26167, #38494, #1263, #36038, #26561, #4734, #7214, #10297, #3956, #19778, #19969, #4147, #17267, #23660, #32353, #17066, #29251, #32158, #1061, #38699, #10494, #16871, #13988, #29645, #23076, #855, #35643, #29451, #13385, #29841, #1656, #26367, #38900, #26764, #36228, #7413, #14191, #13800, #35841, #10694, #39303, #20170, #32753 ),
 .UNSPECIFIED., .F., .F.,
 ( 4, 2, 2, 2, 2, 2, 2, 1, 1, 2, 2, 2, 2, 2, 2, 2, 2, 2, 1, 1, 2, 2, 1, 1, 2, 2, 2, 2, 1, 1, 2, 2, 2, 1, 2, 2, 1, 2, 4 ),
 ( 0.000000000000000000, 0.03012276342170286392, 0.06024552684340572090, 0.09036829026510857787, 0.1204910536868114279, 0.1242563991145242547, 0.1251977354714524926, 0.1261390718283807444, 0.1280217445422372202, 0.1355524353976629293, 0.1506138171085143196, 0.1807365805302170170, 0.2409821073736224395, 0.2485127982290481208, 0.2560434890844738853, 0.2711048707953253034, 0.3012276342170281396, 0.3614731610604337009, 0.3690038519158592711, 0.3727691973435722783, 0.3746518700574291150, 0.3751225382358933658, 0.3755932064143576166, 0.3765345427712861182, 0.3915959244821413110, 0.4217186879038513081, 0.4367800696147063344, 0.4377214059716350025, 0.4386627423285636707, 0.4405454150424208404, 0.4443107604701349578, 0.4518414513255630260, 0.4669028330364197732, 0.4678441693933488854, 0.4683148375718130807, 0.4687855057502772760, 0.4706681784641342237, 0.4744335238918481190, 0.4819642147472753546 ),
 .UNSPECIFIED. ) ;
#5514 = CARTESIAN_POINT ( 'NONE',  ( 25.11613067079463590, -2.903500246237137983, -5.705645831387469613 ) ) ;
#5515 = CARTESIAN_POINT ( 'NONE',  ( 0.7201709579117279159, -51.60714625320436255, 6.000000000000000000 ) ) ;
#5516 = CARTESIAN_POINT ( 'NONE',  ( 1.044648904753755714, -32.99305463038944453, 7.785344483711591934 ) ) ;
#5517 = CARTESIAN_POINT ( 'NONE',  ( 78.81184074671354267, 66.10527324714757924, 1.416821487223875131 ) ) ;
#5518 = CARTESIAN_POINT ( 'NONE',  ( 86.79384979562775015, -0.7021008148363506729, 5.624057257660853182 ) ) ;
#5519 =( BOUNDED_CURVE ( )  B_SPLINE_CURVE ( 3, ( #8046, #10342, #22915, #29682 ),
 .UNSPECIFIED., .F., .T. ) 
 B_SPLINE_CURVE_WITH_KNOTS ( ( 4, 4 ),
 ( 1.422658486313809423, 1.570796326794892561 ),
 .UNSPECIFIED. ) 
 CURVE ( )  GEOMETRIC_REPRESENTATION_ITEM ( )  RATIONAL_B_SPLINE_CURVE ( ( 1.000000000000000000, 0.9981721009331622207, 0.9981721009331622207, 1.000000000000000000 ) ) 
 REPRESENTATION_ITEM ( '' )  );
#5520 = DIRECTION ( 'NONE',  ( 0.5000000000000101030, -0.8660254037844328234, -0.000000000000000000 ) ) ;
#5521 = ORIENTED_EDGE ( 'NONE', *, *, #10304, .F. ) ;
#5522 = CARTESIAN_POINT ( 'NONE',  ( 2.931185808669444448, -32.84638282411071941, 7.695279973900954751 ) ) ;
#5523 = EDGE_CURVE ( 'NONE', #31377, #37191, #31501, .T. ) ;
#5524 = CARTESIAN_POINT ( 'NONE',  ( 4.077110055691020918, -27.00064969655394620, 7.013842709614101167 ) ) ;
#5525 = CARTESIAN_POINT ( 'NONE',  ( 18.23157317310702652, -3.007012085376574717, -3.040421556899932209 ) ) ;
#5526 = CARTESIAN_POINT ( 'NONE',  ( -71.92837670882106238, -42.87473357531881391, -1.732050807568860318 ) ) ;
#5527 = DIRECTION ( 'NONE',  ( 0.9848077530122103518, -0.1736481776669172583, -0.000000000000000000 ) ) ;
#5528 = EDGE_CURVE ( 'NONE', #24744, #4780, #6786, .T. ) ;
#5529 = CARTESIAN_POINT ( 'NONE',  ( 1.899862297872551897, -26.17578186266363360, 6.911401339314954484 ) ) ;
#5530 = VERTEX_POINT ( 'NONE', #37858 ) ;
#5531 = CARTESIAN_POINT ( 'NONE',  ( 30.51366675730394817, -0.1447508928393422822, 4.968793691933281131 ) ) ;
#5532 = EDGE_CURVE ( 'NONE', #29219, #10909, #6387, .T. ) ;
#5533 = CARTESIAN_POINT ( 'NONE',  ( -0.8208322467303189596, -33.90981015991838632, 7.635761828346577573 ) ) ;
#5534 = VECTOR ( 'NONE', #37854, 1000.000000000000000 ) ;
#5535 = VECTOR ( 'NONE', #9973, 1000.000000000000000 ) ;
#5536 = CARTESIAN_POINT ( 'NONE',  ( -1.218159702771259179, -27.82577619805188007, 6.892063359921932530 ) ) ;
#5537 = EDGE_LOOP ( 'NONE', ( #33426, #26109, #21146, #39525, #33214 ) ) ;
#5538 = VERTEX_POINT ( 'NONE', #40533 ) ;
#5540 = CARTESIAN_POINT ( 'NONE',  ( 35.73138356448509256, -1.302398868511517760, 5.536388820249604770 ) ) ;
#5539 = CARTESIAN_POINT ( 'NONE',  ( 80.28274408427735409, 64.63090917800610669, -3.500437194783550421 ) ) ;
#5541 = CARTESIAN_POINT ( 'NONE',  ( 18.10821205226829278, -2.857188514361614473, 3.032622458156649881 ) ) ;
#5542 = CARTESIAN_POINT ( 'NONE',  ( 22.07542296685559435, -3.076855778316415879, -3.556068286084799190 ) ) ;
#5543 = ORIENTED_EDGE ( 'NONE', *, *, #4389, .T. ) ;
#5544 = CARTESIAN_POINT ( 'NONE',  ( 3.751251297819363728, -26.64985754041175525, 6.700000000000000178 ) ) ;
#5545 = AXIS2_PLACEMENT_3D ( 'NONE', #40010, #14476, #9123 ) ;
#5546 = EDGE_LOOP ( 'NONE', ( #23614, #37724, #33149, #7563 ) ) ;
#5547 = ORIENTED_EDGE ( 'NONE', *, *, #38564, .F. ) ;
#5548 = CARTESIAN_POINT ( 'NONE',  ( 1.700390093233090871, -29.56993018339339940, 7.750000000000000888 ) ) ;
#5549 = EDGE_CURVE ( 'NONE', #33766, #32438, #31045, .T. ) ;
#5550 = CARTESIAN_POINT ( 'NONE',  ( 80.42360172120015704, 63.56407742133696104, -3.661914029440274998 ) ) ;
#5551 = CARTESIAN_POINT ( 'NONE',  ( 14.75654458176583006, -5.136929176716047429, 2.500022312476919417 ) ) ;
#5552 = ORIENTED_EDGE ( 'NONE', *, *, #13112, .F. ) ;
#5554 = CARTESIAN_POINT ( 'NONE',  ( -12.99139449055068241, -10.90558813203967148, 2.500000000000000000 ) ) ;
#5553 = CARTESIAN_POINT ( 'NONE',  ( 22.70712101228993873, 2.614415518154956430, 4.662403001875633279 ) ) ;
#5555 = ORIENTED_EDGE ( 'NONE', *, *, #16967, .T. ) ;
#5556 = CARTESIAN_POINT ( 'NONE',  ( 82.03714350014146817, 63.99860240201132910, -2.622983904469594396 ) ) ;
#5557 = CARTESIAN_POINT ( 'NONE',  ( -71.72810306468316810, -21.39745238146776884, 3.947195235487914289 ) ) ;
#5559 = CARTESIAN_POINT ( 'NONE',  ( 26.18165949521383951, -2.762208175416757339, -4.292679188692566150 ) ) ;
#5558 = CARTESIAN_POINT ( 'NONE',  ( -69.08758708074093136, 36.88538962427716683, -9.800414904976365804 ) ) ;
#5560 = CARTESIAN_POINT ( 'NONE',  ( -1.798045670483560343, -29.46480087874731169, 6.863784140767622333 ) ) ;
#5561 = CARTESIAN_POINT ( 'NONE',  ( 73.97359482965943300, 60.32890003735500528, 3.899931323540654748 ) ) ;
#5562 = CARTESIAN_POINT ( 'NONE',  ( 23.71103289728280927, 3.002135961463958669, -3.868039065086897654 ) ) ;
#5563 = ADVANCED_FACE ( 'NONE', ( #24914 ), #3722, .F. ) ;
#5564 = CARTESIAN_POINT ( 'NONE',  ( 21.85643539959777470, 9.109670159223330899, 10.09094178405049647 ) ) ;
#5565 = AXIS2_PLACEMENT_3D ( 'NONE', #5115, #7792, #11267 ) ;
#5566 = ADVANCED_FACE ( 'NONE', ( #25116 ), #34610, .F. ) ;
#5567 = CARTESIAN_POINT ( 'NONE',  ( -30.24874870218063450, -26.64985754041175525, 6.700000000000000178 ) ) ;
#5568 = ORIENTED_EDGE ( 'NONE', *, *, #16410, .F. ) ;
#5569 = FACE_OUTER_BOUND ( 'NONE', #11977, .T. ) ;
#5570 = CARTESIAN_POINT ( 'NONE',  ( 79.93288853953367834, 66.07525097314720597, 2.222430037835993133 ) ) ;
#5571 = CARTESIAN_POINT ( 'NONE',  ( 86.87490948991990081, 0.7757029256828257280, 5.355124474773749199 ) ) ;
#5572 = DIRECTION ( 'NONE',  ( 0.000000000000000000, 0.000000000000000000, 1.000000000000000000 ) ) ;
#5573 = CARTESIAN_POINT ( 'NONE',  ( -33.07867591359219972, -26.64985754041175525, 6.800000000000000711 ) ) ;
#5574 = AXIS2_PLACEMENT_3D ( 'NONE', #22279, #34849, #28221 ) ;
#5575 = CARTESIAN_POINT ( 'NONE',  ( 2.808265793782570796, -32.88997780688298178, 6.863805608295730387 ) ) ;
#5576 = CARTESIAN_POINT ( 'NONE',  ( 33.95810710317707759, -3.751921607304459005, 5.289039422336568208 ) ) ;
#5577 = CARTESIAN_POINT ( 'NONE',  ( 1.077276024005688448, -26.12584348203982643, 7.638132480492517473 ) ) ;
#5578 = CARTESIAN_POINT ( 'NONE',  ( 36.42103784419850143, -3.116709639155254674, -5.890781820352805731 ) ) ;
#5579 = DIRECTION ( 'NONE',  ( 0.000000000000000000, -1.000000000000000000, 0.000000000000000000 ) ) ;
#5580 = CARTESIAN_POINT ( 'NONE',  ( 5.194824081808306460, -29.57876364156226856, 7.773839561854631874 ) ) ;
#5581 = EDGE_CURVE ( 'NONE', #10252, #32142, #15843, .T. ) ;
#5582 = EDGE_CURVE ( 'NONE', #30328, #29646, #9044, .T. ) ;
#5583 = LINE ( 'NONE', #30714, #4646 ) ;
#5584 = EDGE_CURVE ( 'NONE', #16788, #5201, #2789, .T. ) ;
#5585 = DIRECTION ( 'NONE',  ( -0.8820753183692411348, 0.4711084086744811161, -0.000000000000000000 ) ) ;
#5586 = CARTESIAN_POINT ( 'NONE',  ( -69.79879845479261746, -46.12525168278317977, 5.893131031833197753 ) ) ;
#5587 = ORIENTED_EDGE ( 'NONE', *, *, #18430, .F. ) ;
#5588 = CARTESIAN_POINT ( 'NONE',  ( 35.82506826730624283, -3.676139994978682601, 5.658754788095917476 ) ) ;
#5589 = B_SPLINE_CURVE_WITH_KNOTS ( 'NONE', 3,
 ( #1942, #27439, #14461, #33442, #27034, #39579, #17748, #266, #3182, #12806, #15696, #28046, #2969, #34054, #9304, #22093, #37509, #21882, #21476, #22304, #37916, #24972, #34459, #18779, #9511, #12404, #24553, #12605, #25171, #31356, #6235 ),
 .UNSPECIFIED., .F., .F.,
 ( 4, 3, 3, 3, 3, 3, 3, 3, 3, 3, 4 ),
 ( 0.000000000000000000, 3.077658087705419847E-05, 6.152638666999087351E-05, 9.267501192706417050E-05, 0.0001241882240135146176, 0.0001556618703051724378, 0.0001866161554452211381, 0.0002167966385860937832, 0.0002463805737537747790, 0.0002758761370306506470, 0.0002847094172290062959 ),
 .UNSPECIFIED. ) ;
#5590 = DIRECTION ( 'NONE',  ( 0.000000000000000000, 0.000000000000000000, 1.000000000000000000 ) ) ;
#5591 = CARTESIAN_POINT ( 'NONE',  ( 66.95378024648879034, 58.14766406364808660, -3.994852852620100592 ) ) ;
#5592 = CARTESIAN_POINT ( 'NONE',  ( -89.20959394718985891, -29.69173459304409946, 7.754798119455333705 ) ) ;
#5593 = CARTESIAN_POINT ( 'NONE',  ( 5.209482458574877128, -25.70382654691659496, 6.954324564059724878 ) ) ;
#5594 = VECTOR ( 'NONE', #7551, 1000.000000000000000 ) ;
#5595 = ORIENTED_EDGE ( 'NONE', *, *, #7859, .T. ) ;
#5596 = CIRCLE ( 'NONE', #31239, 8.080217238368755162 ) ;
#5597 = CARTESIAN_POINT ( 'NONE',  ( -0.4706772961942385369, -32.18650550059052051, 7.748216051605114174 ) ) ;
#5598 = DIRECTION ( 'NONE',  ( -0.000000000000000000, -0.000000000000000000, 1.000000000000000000 ) ) ;
#5599 = CARTESIAN_POINT ( 'NONE',  ( 15.12608719890447695, 11.51997479474082020, 2.567189751827102295 ) ) ;
#5600 = CARTESIAN_POINT ( 'NONE',  ( -80.85559708689355318, 11.46349645673830686, 1.470518245667309376 ) ) ;
#5601 = DIRECTION ( 'NONE',  ( 0.000000000000000000, 0.000000000000000000, 1.000000000000000000 ) ) ;
#5602 = AXIS2_PLACEMENT_3D ( 'NONE', #29730, #5230, #14074 ) ;
#5603 = VERTEX_POINT ( 'NONE', #418 ) ;
#5604 = LINE ( 'NONE', #30731, #15499 ) ;
#5605 = CARTESIAN_POINT ( 'NONE',  ( 5.751251297819365504, -26.64985754041175525, 6.800000000000000711 ) ) ;
#5606 = ORIENTED_EDGE ( 'NONE', *, *, #31294, .F. ) ;
#5607 = CARTESIAN_POINT ( 'NONE',  ( 21.71895566332458571, 6.267330856689260266, 3.214934355689595957 ) ) ;
#5608 = CARTESIAN_POINT ( 'NONE',  ( 82.56222392620334460, 63.90769089702597228, -1.000000000000000000 ) ) ;
#5609 = CARTESIAN_POINT ( 'NONE',  ( 79.16740428156646203, 65.60392721301286656, 2.747716423863120649 ) ) ;
#5610 = CARTESIAN_POINT ( 'NONE',  ( -0.1471056227823456797, -32.42418307676227585, 6.882085323592684212 ) ) ;
#5611 = VERTEX_POINT ( 'NONE', #37450 ) ;
#5612 = CARTESIAN_POINT ( 'NONE',  ( 77.40632518803428752, 64.64540924511489095, -2.913524936156950851 ) ) ;
#5614 = CARTESIAN_POINT ( 'NONE',  ( 2.255350295996689347, -26.21552723005750352, 7.693875151218753317 ) ) ;
#5613 = CARTESIAN_POINT ( 'NONE',  ( 22.29093078930348781, 0.2567994035360497973, 7.116204519797545203 ) ) ;
#5615 = CARTESIAN_POINT ( 'NONE',  ( 81.42004705249084395, 62.63944267392457022, -2.989933650881958727 ) ) ;
#5616 = CARTESIAN_POINT ( 'NONE',  ( 78.58187568275398860, 60.86241699943124672, 3.054665556626515510 ) ) ;
#5617 = EDGE_CURVE ( 'NONE', #29634, #22430, #1807, .T. ) ;
#5618 = FACE_OUTER_BOUND ( 'NONE', #20905, .T. ) ;
#5619 = CARTESIAN_POINT ( 'NONE',  ( 80.96936403957158745, 66.06451342975873331, 1.623788564013679547 ) ) ;
#5621 = CARTESIAN_POINT ( 'NONE',  ( -1.693538636980199907, -29.36683470281148445, 6.988553391373221402 ) ) ;
#5620 = CARTESIAN_POINT ( 'NONE',  ( 3.469639963590166687, -26.66651138929124798, 7.782034975670473642 ) ) ;
#5622 = CARTESIAN_POINT ( 'NONE',  ( 30.65010716405877034, -0.4808061152566996399, -5.754690052858093097 ) ) ;
#5623 = CARTESIAN_POINT ( 'NONE',  ( -1.772492569845566246, -30.00477039368643162, 7.006908160621414083 ) ) ;
#5624 = DIRECTION ( 'NONE',  ( -0.000000000000000000, -0.000000000000000000, 1.000000000000000000 ) ) ;
#5625 = LINE ( 'NONE', #39378, #31442 ) ;
#5626 = CARTESIAN_POINT ( 'NONE',  ( 24.73872378485249968, 0.6063834911445746823, -4.778905198491438355 ) ) ;
#5627 = EDGE_CURVE ( 'NONE', #30413, #19523, #5765, .T. ) ;
#5628 = CARTESIAN_POINT ( 'NONE',  ( 1.700390093233090871, -29.56993018339339940, -8.199999999999999289 ) ) ;
#5629 = AXIS2_PLACEMENT_3D ( 'NONE', #37575, #30818, #19062 ) ;
#5630 = CARTESIAN_POINT ( 'NONE',  ( -63.99293516169446150, 35.89893413629672381, -12.49999999999999645 ) ) ;
#5631 = CIRCLE ( 'NONE', #22722, 0.1000000000000028644 ) ;
#5632 = CARTESIAN_POINT ( 'NONE',  ( 81.01439173330787469, 61.24733602610728411, 1.383572655854213185 ) ) ;
#5633 = EDGE_CURVE ( 'NONE', #650, #10252, #9247, .T. ) ;
#5634 = CARTESIAN_POINT ( 'NONE',  ( -72.42837670882107659, -47.11702805680359063, 9.886859966642603581 ) ) ;
#5635 = CARTESIAN_POINT ( 'NONE',  ( 37.08867879065032724, -2.428124687478105947, -5.958193899595366716 ) ) ;
#5636 = CARTESIAN_POINT ( 'NONE',  ( -26.34874870218063947, -25.49307895267003587, 6.700000000000000178 ) ) ;
#5637 = CARTESIAN_POINT ( 'NONE',  ( 5.904749997263966321, -30.32498317729107740, 7.635761828346577573 ) ) ;
#5638 = CARTESIAN_POINT ( 'NONE',  ( -0.06469087068677582819, -26.54759843608177761, 7.750000000000000888 ) ) ;
#5639 = DIRECTION ( 'NONE',  ( 1.047444401652940007E-14, -1.000000000000000000, -0.000000000000000000 ) ) ;
#5640 = CARTESIAN_POINT ( 'NONE',  ( -62.92837670882106238, -23.80776546975053520, 6.000000000000000000 ) ) ;
#5641 = CARTESIAN_POINT ( 'NONE',  ( 5.099365965258681577, -29.65337490394464481, 6.870716933885662847 ) ) ;
#5642 = EDGE_CURVE ( 'NONE', #4832, #15795, #7378, .T. ) ;
#5643 = CARTESIAN_POINT ( 'NONE',  ( 4.896323676056323571, -28.40975410443699900, 7.769368695748486431 ) ) ;
#5644 = DIRECTION ( 'NONE',  ( -0.000000000000000000, -0.000000000000000000, 1.000000000000000000 ) ) ;
#5645 = CARTESIAN_POINT ( 'NONE',  ( 25.15062346579604480, 2.408171519380073899, -4.029033621008475841 ) ) ;
#5646 = EDGE_LOOP ( 'NONE', ( #16328, #1258, #15496, #36918, #5372 ) ) ;
#5647 =( BOUNDED_CURVE ( )  B_SPLINE_CURVE ( 3, ( #12905, #30850, #12076, #6130 ),
 .UNSPECIFIED., .F., .F. ) 
 B_SPLINE_CURVE_WITH_KNOTS ( ( 4, 4 ),
 ( 1.381924640371166690, 1.574767692156074483 ),
 .UNSPECIFIED. ) 
 CURVE ( )  GEOMETRIC_REPRESENTATION_ITEM ( )  RATIONAL_B_SPLINE_CURVE ( ( 1.000000000000000000, 0.9969033633783033199, 0.9969033633783033199, 1.000000000000000000 ) ) 
 REPRESENTATION_ITEM ( '' )  );
#5648 = ORIENTED_EDGE ( 'NONE', *, *, #40236, .F. ) ;
#5649 = CARTESIAN_POINT ( 'NONE',  ( 6.372929778535830536, -30.51927953399086846, 6.954324564059724878 ) ) ;
#5650 = CARTESIAN_POINT ( 'NONE',  ( 70.96793116520528599, 59.41887718710786714, -3.976054184260645386 ) ) ;
#5651 = VERTEX_POINT ( 'NONE', #1233 ) ;
#5652 = CARTESIAN_POINT ( 'NONE',  ( 84.69769694898896262, 2.275084749292730635, 4.163914512140848068 ) ) ;
#5653 = CARTESIAN_POINT ( 'NONE',  ( -6.978675913592191193, -26.64985754041175525, 6.700000000000000178 ) ) ;
#5654 = CARTESIAN_POINT ( 'NONE',  ( 69.94804423520642445, 58.60696991578217308, 3.944663542062682993 ) ) ;
#5655 = CARTESIAN_POINT ( 'NONE',  ( 4.806945244714058596, -28.17076227882084183, 7.505001789837628223 ) ) ;
#5656 = CARTESIAN_POINT ( 'NONE',  ( 4.856901937812163617, -30.83345229474961613, 7.768425012602592439 ) ) ;
#5657 = DIRECTION ( 'NONE',  ( -0.000000000000000000, -1.000000000000000000, -0.000000000000000000 ) ) ;
#5658 = VERTEX_POINT ( 'NONE', #10464 ) ;
#5659 = CARTESIAN_POINT ( 'NONE',  ( 22.18507716018001474, 5.290272291513682390, 3.054672883570451081 ) ) ;
#5660 = CARTESIAN_POINT ( 'NONE',  ( 22.64483291760767258, -3.096555847357584934, 3.637248286138076825 ) ) ;
#5661 = AXIS2_PLACEMENT_3D ( 'NONE', #23400, #11424, #36364 ) ;
#5662 = AXIS2_PLACEMENT_3D ( 'NONE', #19730, #23224, #25908 ) ;
#5663 = EDGE_LOOP ( 'NONE', ( #32801, #30202, #33750, #22974 ) ) ;
#5664 = ORIENTED_EDGE ( 'NONE', *, *, #33915, .T. ) ;
#5665 = CARTESIAN_POINT ( 'NONE',  ( 78.41749725426429052, 65.86496093260605278, -1.552792442904348036 ) ) ;
#5666 = CARTESIAN_POINT ( 'NONE',  ( -1.576062547484235354, -30.80072589882973944, 7.695279973900954751 ) ) ;
#5667 = CARTESIAN_POINT ( 'NONE',  ( 81.51618470504202207, 61.58087653888391344, -1.588372325568315535 ) ) ;
#5668 = CARTESIAN_POINT ( 'NONE',  ( 80.84620594802116500, 61.52815374075451871, 2.368006059520743722 ) ) ;
#5669 = AXIS2_PLACEMENT_3D ( 'NONE', #14017, #26589, #10925 ) ;
#5670 = LINE ( 'NONE', #18208, #23214 ) ;
#5671 = CARTESIAN_POINT ( 'NONE',  ( 22.63946314531691328, -3.430231901737621492, -8.286483013797429464 ) ) ;
#5672 = EDGE_LOOP ( 'NONE', ( #15310, #14150, #29169, #26671, #19624 ) ) ;
#5673 = CARTESIAN_POINT ( 'NONE',  ( 2.570535995292712705, -32.96706368601960691, 7.501983001166817822 ) ) ;
#5674 = CARTESIAN_POINT ( 'NONE',  ( -1.315039247493585250, -27.79308300620435901, 6.894806418505347700 ) ) ;
#5675 = CARTESIAN_POINT ( 'NONE',  ( -77.86806181146356209, 9.955796112368622275, -7.213709624780306306 ) ) ;
#5676 = CARTESIAN_POINT ( 'NONE',  ( 3.419158195859356653, -26.52102280379090971, 7.695279973900954751 ) ) ;
#5677 = CARTESIAN_POINT ( 'NONE',  ( 37.00868671504413498, -3.246586382702952633, -5.946932760037821453 ) ) ;
#5678 = CARTESIAN_POINT ( 'NONE',  ( 3.729508372841241925, -32.29806033631375328, 6.997764925645183709 ) ) ;
#5679 = CARTESIAN_POINT ( 'NONE',  ( 15.37661900244130209, 11.52640166518511222, 2.577936354164439781 ) ) ;
#5680 = CARTESIAN_POINT ( 'NONE',  ( -0.4487487021806388365, -25.49307895267003587, 6.700000000000000178 ) ) ;
#5681 = DIRECTION ( 'NONE',  ( 0.000000000000000000, 0.000000000000000000, 1.000000000000000000 ) ) ;
#5682 = CARTESIAN_POINT ( 'NONE',  ( 5.061789821607289852, -29.05897258848950671, 7.782034975670476307 ) ) ;
#5683 = EDGE_CURVE ( 'NONE', #13567, #10739, #17236, .T. ) ;
#5684 = EDGE_CURVE ( 'NONE', #7585, #17512, #7581, .T. ) ;
#5685 = CARTESIAN_POINT ( 'NONE',  ( 18.18564233718114664, 13.54291529513208125, -2.500000000000000444 ) ) ;
#5686 = CARTESIAN_POINT ( 'NONE',  ( 37.20079544340044464, -2.795532513595198054, -5.999424151161432128 ) ) ;
#5687 = ADVANCED_FACE ( 'NONE', ( #7781 ), #26526, .F. ) ;
#5688 = CARTESIAN_POINT ( 'NONE',  ( 24.35226569962506815, 2.912787986373579052, -3.759256437568978093 ) ) ;
#5689 = ORIENTED_EDGE ( 'NONE', *, *, #37373, .T. ) ;
#5690 = AXIS2_PLACEMENT_3D ( 'NONE', #19486, #18867, #12686 ) ;
#5691 = CARTESIAN_POINT ( 'NONE',  ( 66.96362040430034313, 58.12048686563063882, 3.996315564296190725 ) ) ;
#5692 = CARTESIAN_POINT ( 'NONE',  ( 23.01849606021741579, 2.906675443451126384, 3.798991033265373130 ) ) ;
#5693 = DIRECTION ( 'NONE',  ( -0.9999026450364576490, -0.01395351027862084224, 0.000000000000000000 ) ) ;
#5694 = CIRCLE ( 'NONE', #3753, 0.1000000000000028644 ) ;
#5695 = CARTESIAN_POINT ( 'NONE',  ( -89.20959394718985891, -29.69173459304409946, 7.754798119455333705 ) ) ;
#5696 = CARTESIAN_POINT ( 'NONE',  ( 85.01740037914012760, 2.610285099004062470, -3.580537606963684283 ) ) ;
#5698 = CARTESIAN_POINT ( 'NONE',  ( 4.854410821503884144, -30.83963615157586702, 6.864276522220859711 ) ) ;
#5697 = CARTESIAN_POINT ( 'NONE',  ( 32.62845853548997610, -2.537451394787784142, 5.899574533259067444 ) ) ;
#5699 = ORIENTED_EDGE ( 'NONE', *, *, #34988, .T. ) ;
#5700 = CARTESIAN_POINT ( 'NONE',  ( 11.29080664838498649, 1.564594260697056104E-15, -6.000000000000000000 ) ) ;
#5701 = CARTESIAN_POINT ( 'NONE',  ( -0.6442351191163634416, -32.16855289001363616, 6.867199677474201458 ) ) ;
#5702 = VERTEX_POINT ( 'NONE', #29808 ) ;
#5703 = CARTESIAN_POINT ( 'NONE',  ( -69.92837670882107659, -20.82254431570259001, 5.928123921495640936 ) ) ;
#5704 = UNCERTAINTY_MEASURE_WITH_UNIT (LENGTH_MEASURE( 1.000000000000000082E-05 ), #38397, 'distance_accuracy_value', 'NONE');
#5705 = VERTEX_POINT ( 'NONE', #32126 ) ;
#5706 = CARTESIAN_POINT ( 'NONE',  ( 81.02333598550073646, 61.30014629029354722, -1.703597047176645507 ) ) ;
#5707 = CARTESIAN_POINT ( 'NONE',  ( 2.685785295776140114, -32.82400398323339630, 7.013842709614101167 ) ) ;
#5708 = CARTESIAN_POINT ( 'NONE',  ( 78.60310727342863402, 65.99661392892443246, 1.312782405654750129 ) ) ;
#5710 = VERTEX_POINT ( 'NONE', #16834 ) ;
#5709 = CARTESIAN_POINT ( 'NONE',  ( -1.343169602973049548, -31.08543165182933876, 6.969307238440504371 ) ) ;
#5712 = AXIS2_PLACEMENT_3D ( 'NONE', #30670, #9024, #24268 ) ;
#5711 = CARTESIAN_POINT ( 'NONE',  ( 74.40173173411091057, 59.34324565254589601, -3.478821770173325501 ) ) ;
#5713 = CARTESIAN_POINT ( 'NONE',  ( 3.255859414528191387, -32.59326998547489040, 6.876076431790004939 ) ) ;
#5715 = CARTESIAN_POINT ( 'NONE',  ( -64.08758708074091714, 38.43534281692514298, -4.049547700704213327 ) ) ;
#5714 = CARTESIAN_POINT ( 'NONE',  ( 4.923146412972194241, -30.93516854733796961, 6.998987538705428335 ) ) ;
#5716 = CARTESIAN_POINT ( 'NONE',  ( -1.184830056622453887, -27.77117931491062208, 7.761597726988851420 ) ) ;
#5717 = VECTOR ( 'NONE', #39706, 1000.000000000000000 ) ;
#5718 = CARTESIAN_POINT ( 'NONE',  ( -1.534173489221649866, -30.61759350290857284, 7.754798119455333705 ) ) ;
#5719 = VECTOR ( 'NONE', #1594, 1000.000000000000000 ) ;
#5720 = CARTESIAN_POINT ( 'NONE',  ( 22.05245566893604092, 5.319511344851127532, -3.238308893631721919 ) ) ;
#5721 = ORIENTED_EDGE ( 'NONE', *, *, #1032, .F. ) ;
#5722 = CARTESIAN_POINT ( 'NONE',  ( 5.020414555553945668, -30.30303151990228727, 6.868387053540521592 ) ) ;
#5723 = VECTOR ( 'NONE', #34985, 1000.000000000000000 ) ;
#5724 = CARTESIAN_POINT ( 'NONE',  ( 26.57131730419879290, 2.962615056577905026, -1.092182624680714254 ) ) ;
#5725 = CARTESIAN_POINT ( 'NONE',  ( 23.31126753349915504, 9.638235383039575055, 2.500000000000000444 ) ) ;
#5726 = LINE ( 'NONE', #11263, #30076 ) ;
#5727 = CARTESIAN_POINT ( 'NONE',  ( 81.35401977072818624, 62.93507997573772883, 3.162824939346248865 ) ) ;
#5728 = CARTESIAN_POINT ( 'NONE',  ( 86.59537683758360060, -0.3992097724244685342, -5.811584838773467432 ) ) ;
#5729 = CARTESIAN_POINT ( 'NONE',  ( 15.36874315909924249, 11.54028096791004998, 2.577200810392474839 ) ) ;
#5730 = VERTEX_POINT ( 'NONE', #4512 ) ;
#5731 = DIRECTION ( 'NONE',  ( -1.000000000000000000, 0.000000000000000000, 0.000000000000000000 ) ) ;
#5732 = CARTESIAN_POINT ( 'NONE',  ( -72.05775109714784321, -46.12502802752712938, 9.936264230343166304 ) ) ;
#5733 = CARTESIAN_POINT ( 'NONE',  ( 0.000000000000000000, 0.000000000000000000, -6.000000000000000000 ) ) ;
#5734 = CARTESIAN_POINT ( 'NONE',  ( 31.36895993190770682, -3.421856983129734964, -5.044461153598384762 ) ) ;
#5735 = EDGE_CURVE ( 'NONE', #20646, #1547, #35212, .T. ) ;
#5736 = CARTESIAN_POINT ( 'NONE',  ( -67.91293329751151475, 37.48821246048833444, -8.742028012083927990 ) ) ;
#5737 = CARTESIAN_POINT ( 'NONE',  ( 85.67377067720147465, 0.8449287747730311882, 5.870810042200333534 ) ) ;
#5738 = CARTESIAN_POINT ( 'NONE',  ( 1.835860697290446986, -26.17261544377572946, 6.865312560952603782 ) ) ;
#5739 = CARTESIAN_POINT ( 'NONE',  ( 5.021324086407805254, -26.64985754041175525, 6.700000000000000178 ) ) ;
#5740 = CARTESIAN_POINT ( 'NONE',  ( 88.26779375368444391, -0.7888507896528732521, -1.681504516799547710 ) ) ;
#5741 = VERTEX_POINT ( 'NONE', #1427 ) ;
#5742 = EDGE_LOOP ( 'NONE', ( #16157, #12740, #16436, #9941, #6866 ) ) ;
#5744 = CARTESIAN_POINT ( 'NONE',  ( 36.71960778968895056, -3.460346308713754038, 5.859997665240682885 ) ) ;
#5743 = CARTESIAN_POINT ( 'NONE',  ( 81.14684024915200666, 61.29565758240214279, -1.145133111591833286 ) ) ;
#5745 = CARTESIAN_POINT ( 'NONE',  ( 26.16557211405898187, -2.761525329003165830, 4.290168363788568584 ) ) ;
#5746 = CIRCLE ( 'NONE', #22833, 3.000000000000003109 ) ;
#5747 = CARTESIAN_POINT ( 'NONE',  ( 22.02893036045224662, -3.075429753726866888, -3.549435909675389578 ) ) ;
#5748 = AXIS2_PLACEMENT_3D ( 'NONE', #1951, #7896, #20859 ) ;
#5749 = DIRECTION ( 'NONE',  ( 0.000000000000000000, -0.000000000000000000, 1.000000000000000000 ) ) ;
#5750 = AXIS2_PLACEMENT_3D ( 'NONE', #16178, #28745, #25651 ) ;
#5751 = EDGE_LOOP ( 'NONE', ( #40519, #36610, #36898, #6468 ) ) ;
#5752 = CARTESIAN_POINT ( 'NONE',  ( -1.743019459741919519, -30.19677198997656120, 7.643192810543824045 ) ) ;
#5753 = ORIENTED_EDGE ( 'NONE', *, *, #32289, .T. ) ;
#5754 = VERTEX_POINT ( 'NONE', #7183 ) ;
#5755 = LINE ( 'NONE', #28542, #34558 ) ;
#5756 = CARTESIAN_POINT ( 'NONE',  ( 79.07783777134646641, 65.79916784333097723, -2.450942308261427005 ) ) ;
#5757 = CARTESIAN_POINT ( 'NONE',  ( -0.8208322467303189596, -33.90981015991838632, 7.635761828346577573 ) ) ;
#5758 = EDGE_CURVE ( 'NONE', #25658, #23544, #29419, .T. ) ;
#5760 = CARTESIAN_POINT ( 'NONE',  ( 31.36572658741310704, 0.5137713814500121101, 4.593329244990838056 ) ) ;
#5759 = CARTESIAN_POINT ( 'NONE',  ( 22.04698793031429105, 2.546066460137037524, 5.281988517684759188 ) ) ;
#5761 = CARTESIAN_POINT ( 'NONE',  ( 81.16843721835843439, 61.30356250071481128, -1.032522165606414744 ) ) ;
#5762 = DIRECTION ( 'NONE',  ( 0.000000000000000000, 0.000000000000000000, 1.000000000000000000 ) ) ;
#5763 = DIRECTION ( 'NONE',  ( -1.000000000000000000, 0.000000000000000000, 0.000000000000000000 ) ) ;
#5764 = ORIENTED_EDGE ( 'NONE', *, *, #38341, .F. ) ;
#5765 =( BOUNDED_CURVE ( )  B_SPLINE_CURVE ( 3, ( #34405, #6177, #18719, #3123 ),
 .UNSPECIFIED., .F., .T. ) 
 B_SPLINE_CURVE_WITH_KNOTS ( ( 4, 4 ),
 ( 1.347909859412853795, 1.534781240595299190 ),
 .UNSPECIFIED. ) 
 CURVE ( )  GEOMETRIC_REPRESENTATION_ITEM ( )  RATIONAL_B_SPLINE_CURVE ( ( 1.000000000000000000, 0.9970920404276226723, 0.9970920404276226723, 1.000000000000000000 ) ) 
 REPRESENTATION_ITEM ( '' )  );
#5767 = CARTESIAN_POINT ( 'NONE',  ( 1.700390093233090871, -29.56993018339339940, 6.850000000000000533 ) ) ;
#5766 = DIRECTION ( 'NONE',  ( 1.000000000000000000, 0.000000000000000000, 0.000000000000000000 ) ) ;
#5768 = LINE ( 'NONE', #2706, #33667 ) ;
#5769 = CARTESIAN_POINT ( 'NONE',  ( 72.90994289418092933, 61.20204674871914818, 3.824679913472085246 ) ) ;
#5770 = ORIENTED_EDGE ( 'NONE', *, *, #21819, .T. ) ;
#5771 = CARTESIAN_POINT ( 'NONE',  ( 23.46071017023546901, 3.155770004481628810, -3.834925600461499773 ) ) ;
#5772 = EDGE_LOOP ( 'NONE', ( #32075, #7390, #19563, #24589 ) ) ;
#5773 = EDGE_CURVE ( 'NONE', #2073, #26853, #6984, .T. ) ;
#5774 = AXIS2_PLACEMENT_3D ( 'NONE', #14358, #18467, #34159 ) ;
#5775 = CARTESIAN_POINT ( 'NONE',  ( 21.85643539959778181, 11.38078789530947788, 4.862784767728865809 ) ) ;
#5776 = CARTESIAN_POINT ( 'NONE',  ( 3.468923106531234257, -26.56255022247102104, 7.781480525794718162 ) ) ;
#5777 = ORIENTED_EDGE ( 'NONE', *, *, #23425, .F. ) ;
#5778 = CARTESIAN_POINT ( 'NONE',  ( 81.16688244586958945, 61.30299313749269174, 1.050153991572631895 ) ) ;
#5779 = CARTESIAN_POINT ( 'NONE',  ( 88.53816506398004549, -1.092544677973264378, 2.020403607635292254 ) ) ;
#5780 = LINE ( 'NONE', #30909, #25421 ) ;
#5781 = AXIS2_PLACEMENT_3D ( 'NONE', #2495, #11913, #5762 ) ;
#5782 = CARTESIAN_POINT ( 'NONE',  ( 2.798136362750837325, -32.89334079469422534, 6.863784140767622333 ) ) ;
#5783 = CARTESIAN_POINT ( 'NONE',  ( 31.36983548603388527, -3.544126911492940568, 4.957555829163103667 ) ) ;
#5784 = CARTESIAN_POINT ( 'NONE',  ( 21.54940507516195680, 7.328906648784134781, -1.954559343662467308 ) ) ;
#5785 = EDGE_CURVE ( 'NONE', #1114, #33628, #10618, .T. ) ;
#5786 = CARTESIAN_POINT ( 'NONE',  ( 27.40856500620434488, 0.9677877529870252404, -4.484167466504554334 ) ) ;
#5787 = CARTESIAN_POINT ( 'NONE',  ( 5.100255277763929840, -29.60020768353928133, 7.782167645815905033 ) ) ;
#5788 = CARTESIAN_POINT ( 'NONE',  ( 4.634613070157855397, -31.47789877608044051, 6.989977667959441199 ) ) ;
#5789 = VERTEX_POINT ( 'NONE', #23238 ) ;
#5790 = LINE ( 'NONE', #40355, #11847 ) ;
#5791 = CARTESIAN_POINT ( 'NONE',  ( 4.378698603929789712, -31.81803082612050915, 7.767720160662272555 ) ) ;
#5792 = CARTESIAN_POINT ( 'NONE',  ( 1.732966464757989877, -32.97687815986694204, 7.257242401810562349 ) ) ;
#5793 = VERTEX_POINT ( 'NONE', #35609 ) ;
#5794 = CARTESIAN_POINT ( 'NONE',  ( 33.91383790368941931, -0.5462175910584815552, 5.194263850780147074 ) ) ;
#5795 = LINE ( 'NONE', #40361, #4109 ) ;
#5796 = ORIENTED_EDGE ( 'NONE', *, *, #2553, .T. ) ;
#5797 = CARTESIAN_POINT ( 'NONE',  ( 66.89671537544454338, 57.84689108302589489, -3.997688572865332635 ) ) ;
#5798 = CARTESIAN_POINT ( 'NONE',  ( -0.3487487021806359722, -25.49307895267003587, 6.800000000000000711 ) ) ;
#5799 = EDGE_CURVE ( 'NONE', #35245, #25861, #13277, .T. ) ;
#5800 = DIRECTION ( 'NONE',  ( -0.000000000000000000, -0.000000000000000000, -1.000000000000000000 ) ) ;
#5801 = VECTOR ( 'NONE', #31672, 1000.000000000000114 ) ;
#5802 = ORIENTED_EDGE ( 'NONE', *, *, #2902, .F. ) ;
#5803 = CARTESIAN_POINT ( 'NONE',  ( -0.4752369984505682154, -32.18272215034290440, 7.756377446753160321 ) ) ;
#5804 = CARTESIAN_POINT ( 'NONE',  ( 14.93041183113045278, 11.91532239571927221, 2.536649878259312541 ) ) ;
#5805 = VERTEX_POINT ( 'NONE', #20136 ) ;
#5806 = DIRECTION ( 'NONE',  ( -0.000000000000000000, -0.000000000000000000, -1.000000000000000000 ) ) ;
#5807 = CARTESIAN_POINT ( 'NONE',  ( -71.92837670882107659, -20.78299143688747819, 5.916079783099621459 ) ) ;
#5808 = ORIENTED_EDGE ( 'NONE', *, *, #25291, .F. ) ;
#5809 = CARTESIAN_POINT ( 'NONE',  ( 21.86077673335558202, 5.786921160339534964, 3.210078130593202683 ) ) ;
#5810 = CARTESIAN_POINT ( 'NONE',  ( 81.47505553675507883, 61.46950381087523141, -1.024355359505926266 ) ) ;
#5811 = AXIS2_PLACEMENT_3D ( 'NONE', #18177, #2365, #9122 ) ;
#5812 = CARTESIAN_POINT ( 'NONE',  ( 81.11661571137585725, 61.75122346557051145, 2.482170738714641445 ) ) ;
#5813 = CARTESIAN_POINT ( 'NONE',  ( -0.1240150654202767239, -32.43899724728002099, 6.868387053540519815 ) ) ;
#5814 = VERTEX_POINT ( 'NONE', #32514 ) ;
#5815 = CARTESIAN_POINT ( 'NONE',  ( 76.92031397606369580, 59.90536750123401077, -2.950589020716169131 ) ) ;
#5817 = CARTESIAN_POINT ( 'NONE',  ( 0.1825688514500733994, -0.6000000000000004219, 3.931742364882332197 ) ) ;
#5816 = CARTESIAN_POINT ( 'NONE',  ( -72.42837670882109080, -47.01877623127393946, 5.809475019311129529 ) ) ;
#5818 = CARTESIAN_POINT ( 'NONE',  ( -14.24874870218063450, -26.64985754041175525, 6.700000000000000178 ) ) ;
#5819 = ADVANCED_FACE ( 'NONE', ( #4118 ), #821, .F. ) ;
#5820 = EDGE_CURVE ( 'NONE', #5754, #35842, #23779, .T. ) ;
#5821 = CARTESIAN_POINT ( 'NONE',  ( 81.44732304147247248, 62.37541782543058844, -2.773332820897494777 ) ) ;
#5822 = CARTESIAN_POINT ( 'NONE',  ( 76.69853897424475520, 64.65515986876397392, 2.498359881428380724 ) ) ;
#5823 = EDGE_CURVE ( 'NONE', #27773, #26423, #39061, .T. ) ;
#5824 = CARTESIAN_POINT ( 'NONE',  ( -62.92837670882106238, 10.37661300689600097, -6.000000000000000000 ) ) ;
#5825 = VECTOR ( 'NONE', #34273, 1000.000000000000000 ) ;
#5826 = CARTESIAN_POINT ( 'NONE',  ( 79.60403240858897789, 66.28972460246990295, 1.461108304021875970 ) ) ;
#5828 = CARTESIAN_POINT ( 'NONE',  ( -1.576062547484236243, -30.80072589882973944, 7.686927408461904143 ) ) ;
#5827 = PLANE ( 'NONE',  #6671 ) ;
#5829 = VECTOR ( 'NONE', #17337, 1000.000000000000000 ) ;
#5830 = CARTESIAN_POINT ( 'NONE',  ( 33.42314280165584961, -3.731500252021894948, -5.214789010484834897 ) ) ;
#5831 = CARTESIAN_POINT ( 'NONE',  ( -1.391618227887877035, -31.20992771383839681, 6.867199677474202346 ) ) ;
#5832 = CARTESIAN_POINT ( 'NONE',  ( -32.34874870218063592, -25.49307895267003587, 6.700000000000000178 ) ) ;
#5833 = CARTESIAN_POINT ( 'NONE',  ( 1.508261857771285630, -33.06465288214051412, 6.951256099901591767 ) ) ;
#5834 = CARTESIAN_POINT ( 'NONE',  ( 22.00567502167365319, 0.2472497164922489998, -7.635414579327273188 ) ) ;
#5835 = DIRECTION ( 'NONE',  ( 1.000000000000000000, 0.000000000000000000, 0.000000000000000000 ) ) ;
#5836 = ORIENTED_EDGE ( 'NONE', *, *, #30264, .T. ) ;
#5837 = FACE_OUTER_BOUND ( 'NONE', #30901, .T. ) ;
#5838 = CARTESIAN_POINT ( 'NONE',  ( -0.4171441595639596156, -26.78316706317107787, 7.013842709614101167 ) ) ;
#5839 = CARTESIAN_POINT ( 'NONE',  ( -75.45330471031414277, 33.71485196875532608, 15.50000000000000000 ) ) ;
#5840 = CARTESIAN_POINT ( 'NONE',  ( -71.06003735762037365, 0.2170295740194823630, 3.999999999923639304 ) ) ;
#5841 = EDGE_CURVE ( 'NONE', #16079, #3202, #36943, .T. ) ;
#5842 = CARTESIAN_POINT ( 'NONE',  ( 27.74723518964530555, 1.752444360904438225, -4.134722068930840599 ) ) ;
#5843 = CARTESIAN_POINT ( 'NONE',  ( 3.358214364009863839, -32.64710570066487350, 7.771081512783699630 ) ) ;
#5844 = CARTESIAN_POINT ( 'NONE',  ( 5.200390093233091093, -29.58029039483751532, 6.917973428066312103 ) ) ;
#5845 = CARTESIAN_POINT ( 'NONE',  ( 5.042311414493532595, -28.94418112281064381, 7.692469944509197077 ) ) ;
#5846 = CARTESIAN_POINT ( 'NONE',  ( -2.371969930399573379, -31.07359169918526121, 7.013842709614101167 ) ) ;
#5847 = CARTESIAN_POINT ( 'NONE',  ( -89.20959394718985891, -29.62408108485141511, 7.695279973900954751 ) ) ;
#5848 = CARTESIAN_POINT ( 'NONE',  ( -73.82198138812172772, 6.296306154009471356, 10.81584845386062810 ) ) ;
#5849 = CARTESIAN_POINT ( 'NONE',  ( -1.718189074305093600, -25.68532020122240311, 7.754798119455333705 ) ) ;
#5850 = CIRCLE ( 'NONE', #12424, 10.00000000000000888 ) ;
#5851 = DIRECTION ( 'NONE',  ( 0.9961946980917455452, 1.067350013832301366E-17, 0.08715574274765851281 ) ) ;
#5852 = CARTESIAN_POINT ( 'NONE',  ( 22.99834754057519248, 2.264180960916559293, -4.739916070323666020 ) ) ;
#5853 = CARTESIAN_POINT ( 'NONE',  ( -1.528613082588902161, -30.63465995288272126, 6.864651958020303368 ) ) ;
#5854 = ORIENTED_EDGE ( 'NONE', *, *, #11768, .F. ) ;
#5855 = ORIENTED_EDGE ( 'NONE', *, *, #34299, .T. ) ;
#5856 = DIRECTION ( 'NONE',  ( -0.000000000000000000, 0.000000000000000000, 1.000000000000000000 ) ) ;
#5857 = CARTESIAN_POINT ( 'NONE',  ( 69.05402862303502332, 59.18504256499077343, -3.962610901733955693 ) ) ;
#5858 = EDGE_CURVE ( 'NONE', #21009, #37250, #30426, .T. ) ;
#5859 = ORIENTED_EDGE ( 'NONE', *, *, #1308, .T. ) ;
#5860 = CARTESIAN_POINT ( 'NONE',  ( 87.93534175303985023, -2.522256948347837202, 0.2133659395812929627 ) ) ;
#5861 = CARTESIAN_POINT ( 'NONE',  ( 21.85643539959776760, -15.11427361947482062, -2.500000000000000000 ) ) ;
#5862 = CARTESIAN_POINT ( 'NONE',  ( 21.63674588113149611, 6.916792737387225110, 2.999788494245204440 ) ) ;
#5863 = CARTESIAN_POINT ( 'NONE',  ( 4.866926447731218630, -30.80812779013709246, 7.782034975670474530 ) ) ;
#5864 = EDGE_CURVE ( 'NONE', #26146, #34445, #11457, .T. ) ;
#5865 = CARTESIAN_POINT ( 'NONE',  ( 5.050947857257105156, -30.14768253047834179, 7.756377446753164762 ) ) ;
#5866 = VERTEX_POINT ( 'NONE', #27124 ) ;
#5867 = CARTESIAN_POINT ( 'NONE',  ( 23.75598750291871042, 3.574640555080575322, 3.141240283659741284 ) ) ;
#5868 = CARTESIAN_POINT ( 'NONE',  ( 4.077110055691020918, -27.00064969655394620, 7.013842709614101167 ) ) ;
#5869 = ADVANCED_FACE ( 'NONE', ( #14354 ), #39467, .F. ) ;
#5870 = EDGE_LOOP ( 'NONE', ( #27582, #40559, #22660, #20284 ) ) ;
#5871 = CARTESIAN_POINT ( 'NONE',  ( 78.53532592461078821, 65.52573200842934398, -2.475680338657053170 ) ) ;
#5872 = DIRECTION ( 'NONE',  ( -0.000000000000000000, -1.000000000000000000, -0.000000000000000000 ) ) ;
#5873 = CARTESIAN_POINT ( 'NONE',  ( 81.92776049059203558, 62.60942412355767317, -2.397965335136836185 ) ) ;
#5874 = CARTESIAN_POINT ( 'NONE',  ( 78.40460260197330911, 65.77602943765538157, 1.910479420724411126 ) ) ;
#5875 = EDGE_CURVE ( 'NONE', #16084, #17878, #1620, .T. ) ;
#5876 = AXIS2_PLACEMENT_3D ( 'NONE', #3190, #18378, #25181 ) ;
#5877 = LINE ( 'NONE', #28093, #28062 ) ;
#5878 = DIRECTION ( 'NONE',  ( 1.000000000000000000, 0.000000000000000000, -0.000000000000000000 ) ) ;
#5879 = CARTESIAN_POINT ( 'NONE',  ( 22.32070839933769690, 6.022037317923602195, -2.674548383380369376 ) ) ;
#5880 = VERTEX_POINT ( 'NONE', #17843 ) ;
#5881 = CARTESIAN_POINT ( 'NONE',  ( -76.33961693584673469, 9.111181514875148935, 8.435660748604236758 ) ) ;
#5882 = CARTESIAN_POINT ( 'NONE',  ( 37.04963165681110127, -3.191030522870556219, 5.959957271559491510 ) ) ;
#5883 = CARTESIAN_POINT ( 'NONE',  ( -1.314331979139722328, -31.34797709682064948, 7.670465701733750308 ) ) ;
#5884 = DIRECTION ( 'NONE',  ( 0.6605219282605377940, 0.000000000000000000, 0.7508067542896647018 ) ) ;
#5885 = VECTOR ( 'NONE', #35608, 999.9999999999998863 ) ;
#5886 = CARTESIAN_POINT ( 'NONE',  ( 32.91122043559692401, -3.130653418612100225, -5.342989928665543786 ) ) ;
#5887 = CARTESIAN_POINT ( 'NONE',  ( 35.36827583184471990, -3.794046567535431347, -5.509537208948445119 ) ) ;
#5888 = CARTESIAN_POINT ( 'NONE',  ( -1.743814956362963020, -30.10855858896023562, 7.784725160561909441 ) ) ;
#5889 = CARTESIAN_POINT ( 'NONE',  ( -0.2487487021806331078, -25.49307895267003587, 6.800000000000000711 ) ) ;
#5890 = CARTESIAN_POINT ( 'NONE',  ( -10.34874870218063769, -25.49307895267003587, 6.700000000000000178 ) ) ;
#5891 = CARTESIAN_POINT ( 'NONE',  ( 21.85643539959776760, 1.710603452083953179E-15, 2.500000000000000000 ) ) ;
#5892 = CARTESIAN_POINT ( 'NONE',  ( 4.327908163969746980, -31.72774129374395713, 7.695279973900954751 ) ) ;
#5893 = DIRECTION ( 'NONE',  ( 4.199171463528975886E-18, -0.9994119649315837961, 0.03428883712799970368 ) ) ;
#5894 = CARTESIAN_POINT ( 'NONE',  ( 37.19853941620289106, -2.831595418823658061, -6.000000013228142137 ) ) ;
#5895 = CARTESIAN_POINT ( 'NONE',  ( 24.52768585756376751, 2.971958902176091044, -3.615748989836667704 ) ) ;
#5896 = ORIENTED_EDGE ( 'NONE', *, *, #19889, .T. ) ;
#5897 = CARTESIAN_POINT ( 'NONE',  ( 67.54222599743037847, 57.89884484782556484, 3.985038673850038737 ) ) ;
#5898 = CARTESIAN_POINT ( 'NONE',  ( 37.07722502896399419, -2.790003627308526468, 5.993195700482429444 ) ) ;
#5899 = CARTESIAN_POINT ( 'NONE',  ( 4.949073456306528840, -30.85287970687986459, 7.776484688137387913 ) ) ;
#5900 = AXIS2_PLACEMENT_3D ( 'NONE', #34352, #3067, #12282 ) ;
#5901 = ADVANCED_FACE ( 'NONE', ( #24442 ), #37002, .F. ) ;
#5902 = DIRECTION ( 'NONE',  ( -0.8831583674551010121, 0.4690749385695646700, 0.000000000000000000 ) ) ;
#5903 = CARTESIAN_POINT ( 'NONE',  ( 87.00256539079671825, 0.09090593131677454641, 5.889906316148251442 ) ) ;
#5905 = CARTESIAN_POINT ( 'NONE',  ( 35.96793650919964591, -2.128746960111746134, -5.820064398729031474 ) ) ;
#5904 = CARTESIAN_POINT ( 'NONE',  ( -71.80179680180437174, -21.28723728285361005, 5.936304882227263491 ) ) ;
#5906 = ORIENTED_EDGE ( 'NONE', *, *, #11088, .F. ) ;
#5907 = CARTESIAN_POINT ( 'NONE',  ( 24.70447383357791793, 2.647224887469914467, 3.920167867705436571 ) ) ;
#5908 = CARTESIAN_POINT ( 'NONE',  ( 5.200381411266750575, -29.56092842603204573, 7.630645770930537530 ) ) ;
#5909 = ORIENTED_EDGE ( 'NONE', *, *, #38341, .T. ) ;
#5910 = FACE_OUTER_BOUND ( 'NONE', #27777, .T. ) ;
#5911 = ADVANCED_FACE ( 'NONE', ( #8583 ), #33729, .F. ) ;
#5912 = AXIS2_PLACEMENT_3D ( 'NONE', #39931, #33573, #17273 ) ;
#5913 = ORIENTED_EDGE ( 'NONE', *, *, #6200, .F. ) ;
#5914 = CARTESIAN_POINT ( 'NONE',  ( 79.14833415808527661, 65.26800409942002545, -3.041370705153016107 ) ) ;
#5915 = DIRECTION ( 'NONE',  ( 0.000000000000000000, 0.000000000000000000, -1.000000000000000000 ) ) ;
#5916 = CARTESIAN_POINT ( 'NONE',  ( 79.12326768591945836, 65.24646460380061797, 3.052025427726082540 ) ) ;
#5918 = ORIENTED_EDGE ( 'NONE', *, *, #34021, .F. ) ;
#5917 = CARTESIAN_POINT ( 'NONE',  ( -1.341942858788335524, -31.08789270237882718, 6.929923840112062194 ) ) ;
#5919 = EDGE_CURVE ( 'NONE', #3549, #7709, #35556, .T. ) ;
#5920 = CARTESIAN_POINT ( 'NONE',  ( 74.16083781478751291, 62.90537518464178390, -3.184487947857685519 ) ) ;
#5922 = ADVANCED_FACE ( 'NONE', ( #1831 ), #21162, .F. ) ;
#5921 = CARTESIAN_POINT ( 'NONE',  ( -58.80675025188774185, 28.82475471880029616, 5.862912209848245126 ) ) ;
#5923 = CARTESIAN_POINT ( 'NONE',  ( 4.944205726023573888, -30.88437588337916750, 6.867199677474200570 ) ) ;
#5924 = CARTESIAN_POINT ( 'NONE',  ( -71.43192785570207093, -21.65683240571980406, 9.988048282181825499 ) ) ;
#5925 = CARTESIAN_POINT ( 'NONE',  ( 33.89873586150555695, -5.477242531774048295, 0.02003360515015548127 ) ) ;
#5926 = CARTESIAN_POINT ( 'NONE',  ( 22.23079900249558349, 5.088912589733261882, -3.182692338938402532 ) ) ;
#5927 = ORIENTED_EDGE ( 'NONE', *, *, #12119, .F. ) ;
#5928 = CARTESIAN_POINT ( 'NONE',  ( -12.24874870218063627, -25.49307895267003587, 6.700000000000000178 ) ) ;
#5929 = AXIS2_PLACEMENT_3D ( 'NONE', #35134, #32247, #7305 ) ;
#5930 = CARTESIAN_POINT ( 'NONE',  ( -77.11750342460615570, -4.735368223276241295, -7.872399780471171837 ) ) ;
#5931 = CARTESIAN_POINT ( 'NONE',  ( -57.16504416091206053, 33.41445838748276742, 1.000000000000000000 ) ) ;
#5932 = CARTESIAN_POINT ( 'NONE',  ( 81.29167079631679371, 61.38276384236276328, 1.400336002811339631 ) ) ;
#5933 = CARTESIAN_POINT ( 'NONE',  ( 88.36353413610991936, -2.347965962749813063, -0.8794284646705250452 ) ) ;
#5934 = DIRECTION ( 'NONE',  ( -0.8660254037844344888, -0.5000000000000069944, -0.000000000000000000 ) ) ;
#5935 = ORIENTED_EDGE ( 'NONE', *, *, #4293, .F. ) ;
#5936 = CARTESIAN_POINT ( 'NONE',  ( -64.13023603728508704, 35.23430396804722875, -4.479415521045631010 ) ) ;
#5937 = CARTESIAN_POINT ( 'NONE',  ( 3.524795251886475800, -26.70086311950679203, 6.868387053540519815 ) ) ;
#5938 = CARTESIAN_POINT ( 'NONE',  ( 4.072390683603376083, -26.99628265760808077, 6.887547729233689964 ) ) ;
#5939 = AXIS2_PLACEMENT_3D ( 'NONE', #5554, #34399, #28181 ) ;
#5940 = CARTESIAN_POINT ( 'NONE',  ( 28.89993508709290282, -3.472368636922807728, -4.526205258352716143 ) ) ;
#5941 = CARTESIAN_POINT ( 'NONE',  ( 33.62640329583895493, -1.235465025675091422, -5.454611510589393752 ) ) ;
#5942 = CARTESIAN_POINT ( 'NONE',  ( -70.42837670882107659, -36.87473357531881391, -0.8660254037844368202 ) ) ;
#5943 = CARTESIAN_POINT ( 'NONE',  ( 5.021324086407805254, -26.64985754041175525, 6.700000000000000178 ) ) ;
#5944 = CARTESIAN_POINT ( 'NONE',  ( 36.42068411451688092, -3.113243699955915211, 5.890726612280997365 ) ) ;
#5945 = DIRECTION ( 'NONE',  ( 1.000000000000000000, 0.000000000000000000, 0.000000000000000000 ) ) ;
#5946 = ORIENTED_EDGE ( 'NONE', *, *, #21078, .T. ) ;
#5948 = CARTESIAN_POINT ( 'NONE',  ( 27.81821396243497091, 1.847154100788544140, 3.899782868931562785 ) ) ;
#5947 = CARTESIAN_POINT ( 'NONE',  ( 78.92617879813647619, 66.06909554768878934, -1.766895996212476838 ) ) ;
#5949 = CARTESIAN_POINT ( 'NONE',  ( 22.11550089188394352, -2.652446215743125002, 3.658056798225496564 ) ) ;
#5950 = CARTESIAN_POINT ( 'NONE',  ( -70.92837670882107659, -45.61702805680359063, 10.00000000000000888 ) ) ;
#5951 = CARTESIAN_POINT ( 'NONE',  ( -24.44874870218064089, -26.64985754041175525, 6.700000000000000178 ) ) ;
#5952 = ORIENTED_EDGE ( 'NONE', *, *, #19722, .F. ) ;
#5953 = CARTESIAN_POINT ( 'NONE',  ( 28.37783869506044354, -4.100928795493604007, -4.014438774076839245 ) ) ;
#5954 = VERTEX_POINT ( 'NONE', #33941 ) ;
#5955 = VERTEX_POINT ( 'NONE', #14550 ) ;
#5956 = CARTESIAN_POINT ( 'NONE',  ( 78.95300076920055687, 65.89750638847961284, -2.156541836018598612 ) ) ;
#5957 = CARTESIAN_POINT ( 'NONE',  ( -58.86630245980595788, 29.17574657131979521, -6.015288659391247350 ) ) ;
#5958 = VERTEX_POINT ( 'NONE', #36598 ) ;
#5960 = CARTESIAN_POINT ( 'NONE',  ( 4.367500526856323617, -27.46123205189602601, 7.774064877406527962 ) ) ;
#5959 = CARTESIAN_POINT ( 'NONE',  ( 24.37905646352311351, 2.670070934302906540, 3.939568903014517343 ) ) ;
#5961 = ORIENTED_EDGE ( 'NONE', *, *, #13331, .F. ) ;
#5962 = CARTESIAN_POINT ( 'NONE',  ( 81.84810375386628323, 62.06244373962199745, -1.965143080302317768 ) ) ;
#5963 = EDGE_CURVE ( 'NONE', #14079, #38489, #9989, .T. ) ;
#5964 = VECTOR ( 'NONE', #24099, 1000.000000000000000 ) ;
#5966 = EDGE_CURVE ( 'NONE', #16055, #32703, #39966, .T. ) ;
#5965 = DIRECTION ( 'NONE',  ( -0.7541618601367574559, 0.000000000000000000, 0.6566885781822809909 ) ) ;
#5967 = VERTEX_POINT ( 'NONE', #33322 ) ;
#5969 = CARTESIAN_POINT ( 'NONE',  ( 86.88012133546156690, 0.7698487334013246475, -5.007445623867876172 ) ) ;
#5968 = DIRECTION ( 'NONE',  ( 0.000000000000000000, 0.000000000000000000, -1.000000000000000000 ) ) ;
#5970 = LINE ( 'NONE', #28187, #25104 ) ;
#5971 = DIRECTION ( 'NONE',  ( -0.000000000000000000, -0.000000000000000000, -1.000000000000000000 ) ) ;
#5972 = CARTESIAN_POINT ( 'NONE',  ( 73.68135292868622344, 60.99150118422435440, 3.923277237825058439 ) ) ;
#5973 = ORIENTED_EDGE ( 'NONE', *, *, #25995, .T. ) ;
#5974 = CARTESIAN_POINT ( 'NONE',  ( 22.43120517420025806, 3.420092575442463367, -4.253115007774507461 ) ) ;
#5975 = ORIENTED_EDGE ( 'NONE', *, *, #37729, .T. ) ;
#5976 = CARTESIAN_POINT ( 'NONE',  ( 4.712621640174670112, -27.77434364046474258, 7.255881584735163869 ) ) ;
#5977 = CARTESIAN_POINT ( 'NONE',  ( 21.85643539959778892, 11.01376456104441104, -6.033145431426138572 ) ) ;
#5978 = B_SPLINE_CURVE_WITH_KNOTS ( 'NONE', 3,
 ( #32275, #35370, #1383, #10814, #32076, #4074, #3880, #23389, #16397, #35957, #773, #13305, #25878, #38418, #10218, #22798 ),
 .UNSPECIFIED., .F., .F.,
 ( 4, 3, 3, 3, 3, 4 ),
 ( 0.0001585009270395748831, 0.0001815657551981855495, 0.0002118214035944150533, 0.0002420761345915980979, 0.0002723302478207033470, 0.0002816811360866766385 ),
 .UNSPECIFIED. ) ;
#5979 = CARTESIAN_POINT ( 'NONE',  ( -58.96492457584757574, 28.81155473361731723, -6.495248013871978365 ) ) ;
#5980 = ORIENTED_EDGE ( 'NONE', *, *, #11186, .T. ) ;
#5981 = ORIENTED_EDGE ( 'NONE', *, *, #29570, .T. ) ;
#5982 = CARTESIAN_POINT ( 'NONE',  ( -54.01549048184568846, -30.38627270959228710, 6.799999999999999822 ) ) ;
#5983 = CARTESIAN_POINT ( 'NONE',  ( 79.54388053879588938, 66.09379204087662174, 2.134710458528629395 ) ) ;
#5984 = CARTESIAN_POINT ( 'NONE',  ( 88.28392341775159480, -0.8069683938931414557, -2.555979571574120257 ) ) ;
#5985 = VERTEX_POINT ( 'NONE', #5104 ) ;
#5986 = VECTOR ( 'NONE', #5435, 1000.000000000000000 ) ;
#5987 = CARTESIAN_POINT ( 'NONE',  ( 2.717497961161612352, -32.91888605690400027, 6.931070083220557621 ) ) ;
#5988 = EDGE_LOOP ( 'NONE', ( #30833, #13755, #27770, #37888 ) ) ;
#5989 = CARTESIAN_POINT ( 'NONE',  ( 14.68417304430366066, -5.052781308733836241, 2.495429214815205299 ) ) ;
#5990 = CARTESIAN_POINT ( 'NONE',  ( 1.063398716408742395, -26.12838261010132257, 7.660770905198780234 ) ) ;
#5991 = CARTESIAN_POINT ( 'NONE',  ( 25.34284313847354397, 1.862862106151733643, -4.161761609372907067 ) ) ;
#5992 = CARTESIAN_POINT ( 'NONE',  ( 5.141725130632948115, -28.98151016813169889, 7.778495531946298058 ) ) ;
#5993 = DIRECTION ( 'NONE',  ( 0.000000000000000000, 0.000000000000000000, 1.000000000000000000 ) ) ;
#5994 = CIRCLE ( 'NONE', #13956, 0.1000000000000028644 ) ;
#5995 = ORIENTED_EDGE ( 'NONE', *, *, #37321, .T. ) ;
#5996 = CARTESIAN_POINT ( 'NONE',  ( 21.79071535907295498, 5.485802459903661443, -3.529903039149067556 ) ) ;
#5997 = CARTESIAN_POINT ( 'NONE',  ( -69.46739714565912038, -46.72383415856366895, 5.819932703929897144 ) ) ;
#5998 = VECTOR ( 'NONE', #5424, 1000.000000000000000 ) ;
#5999 = ORIENTED_EDGE ( 'NONE', *, *, #2280, .T. ) ;
#6000 = ORIENTED_EDGE ( 'NONE', *, *, #25541, .F. ) ;
#6001 = CARTESIAN_POINT ( 'NONE',  ( 36.65981812739566692, -1.958039781240433763, 5.826225346727439636 ) ) ;
#6002 = FACE_OUTER_BOUND ( 'NONE', #31807, .T. ) ;
#6003 = VERTEX_POINT ( 'NONE', #8376 ) ;
#6004 = CARTESIAN_POINT ( 'NONE',  ( 66.86134338034700875, 57.94508673653880493, -3.999594749380241510 ) ) ;
#6005 = ADVANCED_FACE ( 'NONE', ( #17637 ), #30642, .T. ) ;
#6006 = ORIENTED_EDGE ( 'NONE', *, *, #10369, .F. ) ;
#6007 = CARTESIAN_POINT ( 'NONE',  ( 87.73487586818573902, -0.1902521268519785647, -3.837085321992326659 ) ) ;
#6008 = CARTESIAN_POINT ( 'NONE',  ( -72.89579999368469032, 7.037834574950979416, -9.806287887461893504 ) ) ;
#6009 = CARTESIAN_POINT ( 'NONE',  ( 22.01622206693788897, 4.835086392017111656, 3.641232820207879417 ) ) ;
#6010 =( BOUNDED_CURVE ( )  B_SPLINE_CURVE ( 3, ( #31762, #6648, #23444, #17040 ),
 .UNSPECIFIED., .F., .T. ) 
 B_SPLINE_CURVE_WITH_KNOTS ( ( 4, 4 ),
 ( 1.347909859412853795, 1.534781240595298968 ),
 .UNSPECIFIED. ) 
 CURVE ( )  GEOMETRIC_REPRESENTATION_ITEM ( )  RATIONAL_B_SPLINE_CURVE ( ( 1.000000000000000000, 0.9970920404276226723, 0.9970920404276226723, 1.000000000000000000 ) ) 
 REPRESENTATION_ITEM ( '' )  );
#6011 = FACE_OUTER_BOUND ( 'NONE', #32748, .T. ) ;
#6012 = CARTESIAN_POINT ( 'NONE',  ( 25.11437021580303863, 164.7550792202006562, -4.000000000000000000 ) ) ;
#6013 = ORIENTED_EDGE ( 'NONE', *, *, #4879, .F. ) ;
#6014 = CARTESIAN_POINT ( 'NONE',  ( 21.72140077180526418, 6.245282651313772249, 3.222889655586078206 ) ) ;
#6015 = CARTESIAN_POINT ( 'NONE',  ( 82.31572251369546223, 62.52525979466043538, -1.394285451510165474 ) ) ;
#6016 = CARTESIAN_POINT ( 'NONE',  ( 78.89771339490204127, 65.85133954292349756, 2.202709653501103482 ) ) ;
#6018 = ADVANCED_FACE ( 'NONE', ( #31252 ), #40480, .F. ) ;
#6017 = CARTESIAN_POINT ( 'NONE',  ( -0.1753662704952551610, -32.40569076283811256, 6.929923840112063083 ) ) ;
#6019 = VERTEX_POINT ( 'NONE', #34964 ) ;
#6020 = CARTESIAN_POINT ( 'NONE',  ( 78.03839322897103159, 60.52053993360666340, -3.012346708730617717 ) ) ;
#6021 = CARTESIAN_POINT ( 'NONE',  ( 14.61151433092574159, 13.01680870242209487, -2.486878210787180965 ) ) ;
#6023 = DIRECTION ( 'NONE',  ( -0.000000000000000000, 1.000000000000000000, -0.000000000000000000 ) ) ;
#6022 = CARTESIAN_POINT ( 'NONE',  ( 3.855327937537480487, -32.32757912347058493, 7.754798119455333705 ) ) ;
#6024 = CARTESIAN_POINT ( 'NONE',  ( 0.6134941550689647638, -26.34832452513749956, 7.782034975670476307 ) ) ;
#6025 = CARTESIAN_POINT ( 'NONE',  ( 80.32731820218204177, 65.01876230294878667, -3.279590910092191169 ) ) ;
#6026 = CARTESIAN_POINT ( 'NONE',  ( 77.45380151126714452, 63.20247531706578314, 3.748203062644110073 ) ) ;
#6027 = ORIENTED_EDGE ( 'NONE', *, *, #15336, .T. ) ;
#6028 = ORIENTED_EDGE ( 'NONE', *, *, #12864, .F. ) ;
#6029 = DIRECTION ( 'NONE',  ( -0.000000000000000000, -1.000000000000000000, -0.000000000000000000 ) ) ;
#6030 = CARTESIAN_POINT ( 'NONE',  ( -57.80939613976639180, 32.30609257358648279, 4.182684676774399257 ) ) ;
#6031 = CARTESIAN_POINT ( 'NONE',  ( 82.07520363809508979, 62.17599436785813793, 1.599335268229120199 ) ) ;
#6033 = CYLINDRICAL_SURFACE ( 'NONE', #3222, 0.09010775117052929883 ) ;
#6032 = CARTESIAN_POINT ( 'NONE',  ( -64.08758708074094557, 43.28886537626787145, 1.984762276592526353 ) ) ;
#6034 = CARTESIAN_POINT ( 'NONE',  ( 32.02627343617642453, -1.895034194620857315, -5.999511542327915947 ) ) ;
#6035 = DIRECTION ( 'NONE',  ( -0.000000000000000000, 0.000000000000000000, 1.000000000000000000 ) ) ;
#6036 = CARTESIAN_POINT ( 'NONE',  ( 30.76573472615519833, -3.583077396579174234, 4.803740791053209058 ) ) ;
#6037 = CARTESIAN_POINT ( 'NONE',  ( -64.20341131561859527, 34.94420666461579117, 4.877756629158603197 ) ) ;
#6038 = CARTESIAN_POINT ( 'NONE',  ( 22.63464106450162916, 0.3019483094031678028, -6.468809234137039788 ) ) ;
#6039 = CARTESIAN_POINT ( 'NONE',  ( 0.03672680498656953618, -25.15737950931636036, 7.695279973900954751 ) ) ;
#6040 = DIRECTION ( 'NONE',  ( -0.7394003126383950075, 0.1303762246624157739, 0.6605219282605377940 ) ) ;
#6041 = LINE ( 'NONE', #37712, #22348 ) ;
#6042 = CARTESIAN_POINT ( 'NONE',  ( -14.24874870218063450, -25.49307895267003587, 6.800000000000000711 ) ) ;
#6043 = CARTESIAN_POINT ( 'NONE',  ( 2.138864189560986340, -33.04235649097854832, 7.011627023500183853 ) ) ;
#6044 = CARTESIAN_POINT ( 'NONE',  ( 36.63484890502185465, -2.000711152530542325, -5.847404196664919951 ) ) ;
#6045 = CARTESIAN_POINT ( 'NONE',  ( 80.30472701757432219, 60.99336015429530278, -1.909150740780570121 ) ) ;
#6046 = CARTESIAN_POINT ( 'NONE',  ( -12.99139449055068596, 10.37661300689600097, -2.500000000000000444 ) ) ;
#6047 = CARTESIAN_POINT ( 'NONE',  ( 5.042323503313180133, -28.94424569214364240, 7.691066658568946224 ) ) ;
#6048 = DIRECTION ( 'NONE',  ( 0.9848077530122080203, 0.1736481776669307198, -0.000000000000000000 ) ) ;
#6049 = FACE_OUTER_BOUND ( 'NONE', #23211, .T. ) ;
#6050 = CARTESIAN_POINT ( 'NONE',  ( 2.093335990219729936, -32.94715174935227964, 6.911401339314957148 ) ) ;
#6051 = EDGE_CURVE ( 'NONE', #37345, #3549, #3158, .T. ) ;
#6052 = CARTESIAN_POINT ( 'NONE',  ( -64.08758708074093136, 37.42960919638308326, -3.182465448034689892 ) ) ;
#6053 = CARTESIAN_POINT ( 'NONE',  ( 0.000000000000000000, 4.851177947605531887E-16, 3.961287410364449979 ) ) ;
#6054 = VERTEX_POINT ( 'NONE', #22194 ) ;
#6055 = EDGE_CURVE ( 'NONE', #30629, #40311, #24864, .T. ) ;
#6056 = PLANE ( 'NONE',  #33753 ) ;
#6057 = CARTESIAN_POINT ( 'NONE',  ( 70.04419837359742473, 58.36171959603688464, -3.883859131414874710 ) ) ;
#6058 = ADVANCED_FACE ( 'NONE', ( #40697 ), #2857, .F. ) ;
#6059 = EDGE_CURVE ( 'NONE', #31323, #3657, #24652, .T. ) ;
#6060 = EDGE_LOOP ( 'NONE', ( #26625, #260, #3503, #36638, #29501 ) ) ;
#6061 = CARTESIAN_POINT ( 'NONE',  ( -20.34874870218063947, -26.64985754041175525, 6.700000000000000178 ) ) ;
#6062 = VECTOR ( 'NONE', #17032, 1000.000000000000000 ) ;
#6063 = CARTESIAN_POINT ( 'NONE',  ( 21.85643539959776760, -15.25441669702287939, -1.357504026734941416 ) ) ;
#6064 = CARTESIAN_POINT ( 'NONE',  ( 1.158056475448751454, -26.21346265829786049, 6.894806418505346812 ) ) ;
#6065 = AXIS2_PLACEMENT_3D ( 'NONE', #16273, #10095, #12988 ) ;
#6066 = DIRECTION ( 'NONE',  ( 1.000000000000000000, -0.000000000000000000, -0.000000000000000000 ) ) ;
#6067 = ORIENTED_EDGE ( 'NONE', *, *, #1096, .F. ) ;
#6068 = CARTESIAN_POINT ( 'NONE',  ( 22.18581564090588643, 5.276225145155845730, 3.069190463584780204 ) ) ;
#6069 = CARTESIAN_POINT ( 'NONE',  ( -1.489921458977837565, -30.74547780039133116, 7.635761828346577573 ) ) ;
#6070 = ADVANCED_FACE ( 'NONE', ( #25274 ), #8993, .F. ) ;
#6071 = ORIENTED_EDGE ( 'NONE', *, *, #7592, .T. ) ;
#6072 = CARTESIAN_POINT ( 'NONE',  ( 78.73387159939801450, 65.21990392541003700, -2.961936469198042321 ) ) ;
#6073 = LINE ( 'NONE', #28292, #15127 ) ;
#6074 = CARTESIAN_POINT ( 'NONE',  ( 80.87888400807966605, 65.31646575666023580, -2.869341960395656699 ) ) ;
#6075 = CARTESIAN_POINT ( 'NONE',  ( 78.69113869042872977, 65.45098002628645872, 2.699019001080982250 ) ) ;
#6076 = DIRECTION ( 'NONE',  ( 1.000000000000000000, 0.000000000000000000, 0.000000000000000000 ) ) ;
#6078 = ORIENTED_EDGE ( 'NONE', *, *, #32287, .F. ) ;
#6077 = CARTESIAN_POINT ( 'NONE',  ( -1.181303964486304814, -27.76553572604635534, 7.754798119455333705 ) ) ;
#6079 = CARTESIAN_POINT ( 'NONE',  ( 21.85643539959775694, 4.180186707270823199, 11.06385087694989799 ) ) ;
#6080 = DIRECTION ( 'NONE',  ( -0.000000000000000000, -0.000000000000000000, 1.000000000000000000 ) ) ;
#6081 = ORIENTED_EDGE ( 'NONE', *, *, #10335, .F. ) ;
#6082 = CARTESIAN_POINT ( 'NONE',  ( -73.27055294303096389, 7.677084106314387313, 9.725186251795168602 ) ) ;
#6083 = CARTESIAN_POINT ( 'NONE',  ( -1.799437424176533185, -29.60468789766325415, 7.677493265592890914 ) ) ;
#6084 = EDGE_CURVE ( 'NONE', #20746, #14452, #16946, .T. ) ;
#6085 = CARTESIAN_POINT ( 'NONE',  ( -1.322875202110333603, -31.33341290337725837, 7.638132480492518361 ) ) ;
#6086 = CARTESIAN_POINT ( 'NONE',  ( -80.90823458386326195, 10.55951580149532809, 0.6344085041158121774 ) ) ;
#6087 = CARTESIAN_POINT ( 'NONE',  ( 32.91903012308263499, -3.045910662517542722, -5.344208819095712215 ) ) ;
#6088 = CARTESIAN_POINT ( 'NONE',  ( 21.74038104888381895, 4.236694489823714882, -2.795633211743734581 ) ) ;
#6089 = APPLICATION_CONTEXT ( 'automotive_design' ) ;
#6090 = CARTESIAN_POINT ( 'NONE',  ( 3.721384798075928035, -32.30408232086368514, 6.939395833800444890 ) ) ;
#6091 = CARTESIAN_POINT ( 'NONE',  ( 14.62323830247504119, 13.01685296470267517, 2.488708020092772699 ) ) ;
#6092 = CARTESIAN_POINT ( 'NONE',  ( -0.06129048428309483154, -26.54561512989744188, 7.635761828346575797 ) ) ;
#6093 = CARTESIAN_POINT ( 'NONE',  ( 30.07655335801453234, -3.716434046306707373, 4.568522214145315452 ) ) ;
#6094 = DIRECTION ( 'NONE',  ( -0.000000000000000000, -1.000000000000000000, -0.000000000000000000 ) ) ;
#6095 = CIRCLE ( 'NONE', #34385, 95.38357402481355507 ) ;
#6096 = CARTESIAN_POINT ( 'NONE',  ( 18.41743161276554019, 13.31819020379082197, -2.500000000000000000 ) ) ;
#6097 = CARTESIAN_POINT ( 'NONE',  ( 25.33510812559238801, 0.7739518545062052945, -4.607785389428086020 ) ) ;
#6098 = CARTESIAN_POINT ( 'NONE',  ( 36.48031136538276087, -1.766077765691559831, -5.744066426338735099 ) ) ;
#6099 = CARTESIAN_POINT ( 'NONE',  ( 24.35746132025820287, 2.925223658202782406, -3.744337438357647319 ) ) ;
#6100 = ORIENTED_EDGE ( 'NONE', *, *, #15103, .T. ) ;
#6102 = EDGE_CURVE ( 'NONE', #36975, #15644, #7951, .T. ) ;
#6101 = CARTESIAN_POINT ( 'NONE',  ( 66.95378024648879034, 58.14766406364808660, 3.994852852620100592 ) ) ;
#6103 = CARTESIAN_POINT ( 'NONE',  ( 30.55148721072670881, -0.03398917485607633182, 4.974696488381029624 ) ) ;
#6104 = CARTESIAN_POINT ( 'NONE',  ( 1.700390093233090871, -29.56993018339339940, 7.800000000000000711 ) ) ;
#6105 = ADVANCED_FACE ( 'NONE', ( #12289 ), #9611, .F. ) ;
#6106 = DIRECTION ( 'NONE',  ( 0.000000000000000000, 0.000000000000000000, 1.000000000000000000 ) ) ;
#6107 = CARTESIAN_POINT ( 'NONE',  ( 84.68420644151177612, 2.996072101527111453, 1.894685230139086851 ) ) ;
#6109 = CARTESIAN_POINT ( 'NONE',  ( 2.290977028701361107, -26.12011756940199447, 7.750000000000000888 ) ) ;
#6108 = LINE ( 'NONE', #147, #26129 ) ;
#6110 = VERTEX_POINT ( 'NONE', #30848 ) ;
#6111 = CARTESIAN_POINT ( 'NONE',  ( 24.71577694999333374, 3.003426287302215947, 3.428006812919407231 ) ) ;
#6112 = VECTOR ( 'NONE', #28962, 1000.000000000000000 ) ;
#6113 = DIRECTION ( 'NONE',  ( 1.000000000000000000, 0.000000000000000000, 0.000000000000000000 ) ) ;
#6114 = CARTESIAN_POINT ( 'NONE',  ( 0.9075698686646886948, -32.88344056124241632, 7.386948897581447682 ) ) ;
#6115 = VERTEX_POINT ( 'NONE', #19087 ) ;
#6116 = CARTESIAN_POINT ( 'NONE',  ( -70.81922763566456069, -21.77701682883130019, 6.011051262898291725 ) ) ;
#6117 = PRODUCT_DEFINITION_CONTEXT ( 'detailed design', #21603, 'design' ) ;
#6118 = ORIENTED_EDGE ( 'NONE', *, *, #11465, .F. ) ;
#6119 = CARTESIAN_POINT ( 'NONE',  ( 79.67348887277924518, 64.26584687736622925, -3.653685850874240248 ) ) ;
#6120 = CARTESIAN_POINT ( 'NONE',  ( -1.698424725305372363, -29.48016477088195231, 7.778050822775633755 ) ) ;
#6121 = CARTESIAN_POINT ( 'NONE',  ( 78.54140637431730454, 65.95282500403628489, 1.409197735201547674 ) ) ;
#6124 = EDGE_LOOP ( 'NONE', ( #40131, #15007, #3733, #16778 ) ) ;
#6123 = CARTESIAN_POINT ( 'NONE',  ( -26.24874870218063450, -25.49307895267003587, 6.800000000000000711 ) ) ;
#6122 = AXIS2_PLACEMENT_3D ( 'NONE', #20569, #33156, #7623 ) ;
#6125 = CARTESIAN_POINT ( 'NONE',  ( -58.83478692283225087, 28.75339845897402924, 5.944647730637774075 ) ) ;
#6126 =( BOUNDED_CURVE ( )  B_SPLINE_CURVE ( 3, ( #18104, #5976, #27380, #18516 ),
 .UNSPECIFIED., .F., .F. ) 
 B_SPLINE_CURVE_WITH_KNOTS ( ( 4, 4 ),
 ( 1.347909859412852907, 1.534781240595297636 ),
 .UNSPECIFIED. ) 
 CURVE ( )  GEOMETRIC_REPRESENTATION_ITEM ( )  RATIONAL_B_SPLINE_CURVE ( ( 1.000000000000000000, 0.9970920404276226723, 0.9970920404276226723, 1.000000000000000000 ) ) 
 REPRESENTATION_ITEM ( '' )  );
#6128 = CARTESIAN_POINT ( 'NONE',  ( -64.08758708074093136, 38.55592700272130458, -3.000000000000462297 ) ) ;
#6127 = CARTESIAN_POINT ( 'NONE',  ( 4.966824528213045653, -30.82710434516975795, 6.870737987065015595 ) ) ;
#6129 = CARTESIAN_POINT ( 'NONE',  ( 3.419158195859356653, -26.52102280379090971, 7.695279973900954751 ) ) ;
#6130 = CARTESIAN_POINT ( 'NONE',  ( -0.01129010125266571157, -26.63221833370405633, 7.635761828346577573 ) ) ;
#6131 = CARTESIAN_POINT ( 'NONE',  ( 21.87171821392831461, 5.720550014221652546, -3.238356660519563501 ) ) ;
#6132 = ORIENTED_EDGE ( 'NONE', *, *, #33263, .F. ) ;
#6133 = CARTESIAN_POINT ( 'NONE',  ( 24.68629359590044459, -1.668547755296895696, 6.687296101055469677 ) ) ;
#6134 = CARTESIAN_POINT ( 'NONE',  ( -76.78746716544362982, -5.933295494910943546, -8.113055081387594569 ) ) ;
#6135 = CARTESIAN_POINT ( 'NONE',  ( -4.348748702180639469, -26.64985754041175525, 6.700000000000000178 ) ) ;
#6136 = CARTESIAN_POINT ( 'NONE',  ( 78.95529765307296088, 66.08830754916627370, 1.741375869723574166 ) ) ;
#6137 = CARTESIAN_POINT ( 'NONE',  ( 84.47734884986269321, 2.726878650076010491, -2.900369371603537694 ) ) ;
#6138 = CARTESIAN_POINT ( 'NONE',  ( 0.6636879034114320230, -26.22699007480350986, 7.013842709614101167 ) ) ;
#6139 = EDGE_LOOP ( 'NONE', ( #28431, #9454, #31126, #36309 ) ) ;
#6140 = CARTESIAN_POINT ( 'NONE',  ( -64.85784325972055342, 34.81586596186931359, -6.466735817496061856 ) ) ;
#6141 = CARTESIAN_POINT ( 'NONE',  ( -0.8786759135921904385, -26.64985754041175525, 6.700000000000000178 ) ) ;
#6142 = EDGE_CURVE ( 'NONE', #4923, #5702, #21778, .T. ) ;
#6143 = CARTESIAN_POINT ( 'NONE',  ( 3.985343101274590794, -26.91869073241397103, 6.880608371227950215 ) ) ;
#6144 = EDGE_CURVE ( 'NONE', #29030, #24859, #17791, .T. ) ;
#6145 = CARTESIAN_POINT ( 'NONE',  ( 16.08354769902080506, -3.539635827824002767, -2.696278765112280151 ) ) ;
#6146 = CARTESIAN_POINT ( 'NONE',  ( -64.55204904898397444, 36.12561474966231856, -8.218049716820861050 ) ) ;
#6147 = PLANE ( 'NONE',  #39109 ) ;
#6148 = CARTESIAN_POINT ( 'NONE',  ( 1.907370182495600641, -26.17623391135161626, 6.979335674598003969 ) ) ;
#6149 = ORIENTED_EDGE ( 'NONE', *, *, #12827, .T. ) ;
#6150 = CARTESIAN_POINT ( 'NONE',  ( 36.19339270046786794, -2.233506198504079610, 5.855252290054989928 ) ) ;
#6151 = PRESENTATION_LAYER_ASSIGNMENT (  '', '', ( #34437 ) ) ;
#6152 = EDGE_CURVE ( 'NONE', #29514, #3715, #10420, .T. ) ;
#6153 = EDGE_CURVE ( 'NONE', #33795, #1662, #9074, .T. ) ;
#6154 = CARTESIAN_POINT ( 'NONE',  ( 85.70831578087668845, 2.086076349557777654, 3.711011680213312403 ) ) ;
#6155 = ORIENTED_EDGE ( 'NONE', *, *, #35181, .F. ) ;
#6157 = LINE ( 'NONE', #31279, #12541 ) ;
#6156 = CARTESIAN_POINT ( 'NONE',  ( 80.94524665917968775, 63.44345826879091277, -3.487490852634244742 ) ) ;
#6158 = CARTESIAN_POINT ( 'NONE',  ( -69.73576780118902718, -46.20203278094625432, 9.928780194719321273 ) ) ;
#6159 = CARTESIAN_POINT ( 'NONE',  ( 14.67067689388392360, 13.26234298596911287, -2.496111959588981133 ) ) ;
#6160 = ORIENTED_EDGE ( 'NONE', *, *, #34843, .F. ) ;
#6161 = DIRECTION ( 'NONE',  ( 0.000000000000000000, 0.000000000000000000, 1.000000000000000000 ) ) ;
#6162 = CARTESIAN_POINT ( 'NONE',  ( -0.4545477510665002496, -26.81228124332190532, 7.754798119455333705 ) ) ;
#6163 = ORIENTED_EDGE ( 'NONE', *, *, #33342, .T. ) ;
#6164 = AXIS2_PLACEMENT_3D ( 'NONE', #17557, #14677, #26652 ) ;
#6165 = ORIENTED_EDGE ( 'NONE', *, *, #30007, .F. ) ;
#6166 = CARTESIAN_POINT ( 'NONE',  ( 79.14683388637743633, 65.58698894143067548, -2.758686562281584376 ) ) ;
#6167 = CARTESIAN_POINT ( 'NONE',  ( 5.153279172109080264, -30.14225614731511982, 7.701614758090453705 ) ) ;
#6168 = ORIENTED_EDGE ( 'NONE', *, *, #11372, .T. ) ;
#6170 = CARTESIAN_POINT ( 'NONE',  ( 36.09228681445222264, -1.514627514507355333, 5.635688615691564429 ) ) ;
#6169 = CARTESIAN_POINT ( 'NONE',  ( 24.81493965045673633, 2.585987335596099168, 3.949178272049961969 ) ) ;
#6171 = ORIENTED_EDGE ( 'NONE', *, *, #13948, .T. ) ;
#6172 = CARTESIAN_POINT ( 'NONE',  ( 82.01382571621886086, 63.62535219989227642, -2.645340681430279339 ) ) ;
#6173 = CIRCLE ( 'NONE', #37675, 2.500000000000000000 ) ;
#6174 = CARTESIAN_POINT ( 'NONE',  ( 4.749297472835600331, -31.28869828601962766, 7.695279973900954751 ) ) ;
#6176 = CARTESIAN_POINT ( 'NONE',  ( -2.697268050091675118E-17, 3.729367930467589076, 6.000000000000000000 ) ) ;
#6175 = DIRECTION ( 'NONE',  ( 1.000000000000000000, 0.000000000000000000, 0.000000000000000000 ) ) ;
#6177 = CARTESIAN_POINT ( 'NONE',  ( 1.043334534275603742, -26.12523165986777585, 7.255881584735162093 ) ) ;
#6178 = CARTESIAN_POINT ( 'NONE',  ( -64.08758708074093136, 41.04287353446839148, -4.000000000000000000 ) ) ;
#6179 = CARTESIAN_POINT ( 'NONE',  ( 72.80781396401921768, 61.43345056764702861, 3.736020861133335647 ) ) ;
#6180 = CARTESIAN_POINT ( 'NONE',  ( 21.85662909133909082, 3.729105680040489812, -4.537925847320513739 ) ) ;
#6181 = ORIENTED_EDGE ( 'NONE', *, *, #21170, .T. ) ;
#6182 = CARTESIAN_POINT ( 'NONE',  ( 0.5037982502477853508, -26.38745190989316214, 7.695279973900954751 ) ) ;
#6183 = CARTESIAN_POINT ( 'NONE',  ( 21.85643539959774628, 7.825395393543534972, -11.66269361450695108 ) ) ;
#6184 = CARTESIAN_POINT ( 'NONE',  ( 3.527976676500487851, -26.59338346714900680, 7.776484688137387025 ) ) ;
#6185 = ORIENTED_EDGE ( 'NONE', *, *, #38506, .T. ) ;
#6186 = LINE ( 'NONE', #31310, #14249 ) ;
#6187 = CARTESIAN_POINT ( 'NONE',  ( 80.14906791408223796, 65.90796394341653297, 2.445541897054074987 ) ) ;
#6188 = CARTESIAN_POINT ( 'NONE',  ( 85.42332570945818304, 2.406190724219733568, -3.391956346677281076 ) ) ;
#6189 = ORIENTED_EDGE ( 'NONE', *, *, #32745, .F. ) ;
#6190 = DIRECTION ( 'NONE',  ( -1.188227527617580984E-16, -0.9905719730871677120, 0.1369933068956136479 ) ) ;
#6191 = ORIENTED_EDGE ( 'NONE', *, *, #528, .F. ) ;
#6192 = CARTESIAN_POINT ( 'NONE',  ( 31.36247516317754247, -3.421439689148831231, 5.043473584804893939 ) ) ;
#6193 = AXIS2_PLACEMENT_3D ( 'NONE', #11837, #39644, #36563 ) ;
#6194 = VECTOR ( 'NONE', #19336, 1000.000000000000000 ) ;
#6195 = CARTESIAN_POINT ( 'NONE',  ( -2.697268050091675118E-17, 3.729367930467589076, -2.500000000000000000 ) ) ;
#6196 = CARTESIAN_POINT ( 'NONE',  ( 25.29915376873320199, 1.743595656015987538, -4.154942826593681637 ) ) ;
#6197 = CARTESIAN_POINT ( 'NONE',  ( 5.098690994628564788, -29.67766195414260366, 7.768425012602595103 ) ) ;
#6198 = LINE ( 'NONE', #12765, #25954 ) ;
#6199 = EDGE_CURVE ( 'NONE', #28383, #14367, #14170, .T. ) ;
#6200 = EDGE_CURVE ( 'NONE', #35146, #23027, #35755, .T. ) ;
#6201 = CIRCLE ( 'NONE', #29844, 3.499999999999999556 ) ;
#6202 = CARTESIAN_POINT ( 'NONE',  ( -16.97867591359219475, -26.64985754041175525, 6.700000000000000178 ) ) ;
#6203 = ADVANCED_FACE ( 'NONE', ( #16198 ), #7531, .F. ) ;
#6204 = VERTEX_POINT ( 'NONE', #35161 ) ;
#6205 = ORIENTED_EDGE ( 'NONE', *, *, #12515, .F. ) ;
#6206 = CARTESIAN_POINT ( 'NONE',  ( 37.10374867307626801, -3.125519533824888452, 5.976337534025341292 ) ) ;
#6207 = FACE_OUTER_BOUND ( 'NONE', #32119, .T. ) ;
#6208 = CARTESIAN_POINT ( 'NONE',  ( 66.43286826475046780, 57.76021747899716985, -4.000000000000007105 ) ) ;
#6209 = CARTESIAN_POINT ( 'NONE',  ( 87.67710904054415266, -2.211298689107902504, -2.754471170594727791 ) ) ;
#6210 = ORIENTED_EDGE ( 'NONE', *, *, #22675, .T. ) ;
#6211 = CARTESIAN_POINT ( 'NONE',  ( -56.31571917568491870, 30.58480147475563626, 3.912689169536869738 ) ) ;
#6212 = CARTESIAN_POINT ( 'NONE',  ( 2.388817387744127441, -25.35382237095210201, 7.695279973900954751 ) ) ;
#6213 = CARTESIAN_POINT ( 'NONE',  ( 66.41543808532628645, 57.82433660857527258, 4.000000000000015987 ) ) ;
#6214 = CARTESIAN_POINT ( 'NONE',  ( -0.9449608208177665558, -27.27818007888150120, 6.875671892026063325 ) ) ;
#6215 = FACE_BOUND ( 'NONE', #8974, .T. ) ;
#6216 = DIRECTION ( 'NONE',  ( -1.000000000000000000, 0.000000000000000000, 0.000000000000000000 ) ) ;
#6217 = VERTEX_POINT ( 'NONE', #4068 ) ;
#6218 = CARTESIAN_POINT ( 'NONE',  ( 22.62405152208049941, 4.580528983382354369, 3.090851274182689679 ) ) ;
#6219 = CARTESIAN_POINT ( 'NONE',  ( 82.15576060805985037, 62.21674973124318342, -1.325417871280742066 ) ) ;
#6221 = VECTOR ( 'NONE', #36089, 1000.000000000000000 ) ;
#6220 = CARTESIAN_POINT ( 'NONE',  ( 78.78378587176689507, 65.95784816145936702, 1.911132874451720864 ) ) ;
#6222 = CARTESIAN_POINT ( 'NONE',  ( 2.947205120345838480, -26.40679055824786303, 7.778050822775630202 ) ) ;
#6223 = ORIENTED_EDGE ( 'NONE', *, *, #15906, .T. ) ;
#6224 = CARTESIAN_POINT ( 'NONE',  ( 76.19461364182978969, 62.94386820200831067, -3.683100983535286588 ) ) ;
#6226 = LINE ( 'NONE', #18358, #16451 ) ;
#6225 = CARTESIAN_POINT ( 'NONE',  ( -72.37992470321633220, -46.72631451928356228, 5.821804174376780772 ) ) ;
#6227 = CARTESIAN_POINT ( 'NONE',  ( 18.39501626872469231, 7.834513951104746354, -3.077385192520857071 ) ) ;
#6228 = CARTESIAN_POINT ( 'NONE',  ( 81.37039951255469816, 61.83949519909545245, -2.349509806045110949 ) ) ;
#6229 = CARTESIAN_POINT ( 'NONE',  ( 79.35831483666107999, 61.48221340643413413, 3.218236826935628070 ) ) ;
#6230 = ORIENTED_EDGE ( 'NONE', *, *, #17686, .T. ) ;
#6231 = AXIS2_PLACEMENT_3D ( 'NONE', #40551, #28835, #3740 ) ;
#6232 = CARTESIAN_POINT ( 'NONE',  ( -6.978675913592191193, -26.64985754041175525, 6.700000000000000178 ) ) ;
#6233 = CARTESIAN_POINT ( 'NONE',  ( 0.5241206729324208169, -32.86635431953688169, 7.743886751744252450 ) ) ;
#6234 = CARTESIAN_POINT ( 'NONE',  ( 82.31242756469306698, 63.41700585080328523, 2.192618372226454504 ) ) ;
#6236 = CARTESIAN_POINT ( 'NONE',  ( -1.694095407703923861, -29.37624715910394002, 7.006423389747790331 ) ) ;
#6235 = CARTESIAN_POINT ( 'NONE',  ( 4.269670580072574495, -31.94665014585129725, 7.013842709614101167 ) ) ;
#6237 = CARTESIAN_POINT ( 'NONE',  ( 29.95345716813442749, -1.222334143750352764, -6.038643835265099291 ) ) ;
#6238 = CARTESIAN_POINT ( 'NONE',  ( -1.411741797515851271, -31.17137799540083876, 7.013842709614101167 ) ) ;
#6239 = CARTESIAN_POINT ( 'NONE',  ( -62.73984912080872789, 35.89138081568317062, -5.261690063483860591 ) ) ;
#6240 = CARTESIAN_POINT ( 'NONE',  ( 1.518277080292407044, -33.06519117755393466, 6.912143950357348743 ) ) ;
#6241 = CARTESIAN_POINT ( 'NONE',  ( 22.62321569360657136, 0.2992175222827407333, -6.483806668115875027 ) ) ;
#6242 = DIRECTION ( 'NONE',  ( 0.7877517966954343809, -0.6159927814537400348, 0.000000000000000000 ) ) ;
#6243 = CARTESIAN_POINT ( 'NONE',  ( -0.6421092404456101299, -32.03421449887897410, 6.949473656533215582 ) ) ;
#6244 = CARTESIAN_POINT ( 'NONE',  ( 1.700390093233090871, -29.56993018339339940, -15.49999999999999822 ) ) ;
#6245 = DIRECTION ( 'NONE',  ( -1.000000000000000000, 0.000000000000000000, 0.000000000000000000 ) ) ;
#6246 = CARTESIAN_POINT ( 'NONE',  ( 23.34994961758268062, 3.524620780518698204, -3.233128968679401360 ) ) ;
#6247 = DIRECTION ( 'NONE',  ( -0.000000000000000000, -0.000000000000000000, 1.000000000000000000 ) ) ;
#6248 = CARTESIAN_POINT ( 'NONE',  ( -0.9297026075730506767, -31.72462434039837476, 7.784838882742139532 ) ) ;
#6249 = FACE_OUTER_BOUND ( 'NONE', #18452, .T. ) ;
#6250 = PRODUCT_DEFINITION_SHAPE ( 'NONE', 'NONE',  #40727 ) ;
#6251 = LINE ( 'NONE', #9125, #29264 ) ;
#6252 = CARTESIAN_POINT ( 'NONE',  ( 2.104653383086854124, -32.94581586666951978, 6.895222827070023541 ) ) ;
#6253 = DIRECTION ( 'NONE',  ( -1.000000000000000000, 0.000000000000000000, 0.000000000000000000 ) ) ;
#6254 = COLOUR_RGB ( '',0.7921568627450980005, 0.8196078431372548767, 0.9333333333333333481 ) ;
#6255 = CARTESIAN_POINT ( 'NONE',  ( -4.448748702180642667, -26.64985754041175525, 6.800000000000000711 ) ) ;
#6256 = AXIS2_PLACEMENT_3D ( 'NONE', #2464, #21586, #27545 ) ;
#6257 = EDGE_CURVE ( 'NONE', #14282, #7409, #3674, .T. ) ;
#6258 = EDGE_LOOP ( 'NONE', ( #35709, #15630, #24145, #13795 ) ) ;
#6259 = CARTESIAN_POINT ( 'NONE',  ( -2.640659097302433533, -29.59008065498625939, 7.013842709614101167 ) ) ;
#6260 = CARTESIAN_POINT ( 'NONE',  ( 68.56660431458814742, 58.72100381882076192, -3.990501929453217134 ) ) ;
#6261 = CIRCLE ( 'NONE', #7536, 79.54614097552274643 ) ;
#6262 = ORIENTED_EDGE ( 'NONE', *, *, #25995, .F. ) ;
#6263 = LINE ( 'NONE', #9330, #3572 ) ;
#6264 = DIRECTION ( 'NONE',  ( 1.000000000000000000, 0.000000000000000000, 0.000000000000000000 ) ) ;
#6265 = CARTESIAN_POINT ( 'NONE',  ( 1.314916516662855361, -26.19185006800425342, 6.979335674598003081 ) ) ;
#6266 = DIRECTION ( 'NONE',  ( 0.000000000000000000, 0.000000000000000000, 1.000000000000000000 ) ) ;
#6267 = ORIENTED_EDGE ( 'NONE', *, *, #16721, .T. ) ;
#6268 = CARTESIAN_POINT ( 'NONE',  ( 24.75999223784396719, 3.019925347883366307, 3.347241732953214477 ) ) ;
#6269 = CARTESIAN_POINT ( 'NONE',  ( -30.24874870218063450, -26.64985754041175525, 6.700000000000000178 ) ) ;
#6270 = CARTESIAN_POINT ( 'NONE',  ( -1.749422520758312505, -28.97934324792513294, 7.750000000000000000 ) ) ;
#6271 = ORIENTED_EDGE ( 'NONE', *, *, #11072, .T. ) ;
#6272 = CARTESIAN_POINT ( 'NONE',  ( 78.97528327045988306, 64.81351720955758822, -3.340572457511928661 ) ) ;
#6274 = CARTESIAN_POINT ( 'NONE',  ( -1.674636587911282781, -29.98134230076460227, 6.887945620086122211 ) ) ;
#6273 = CARTESIAN_POINT ( 'NONE',  ( 21.73607458324352137, 0.2916839156606184091, 8.911482056295868759 ) ) ;
#6275 = CARTESIAN_POINT ( 'NONE',  ( 80.50371486736973736, 65.47929316355251217, -2.914706979937543796 ) ) ;
#6276 = ADVANCED_FACE ( 'NONE', ( #22794 ), #35561, .F. ) ;
#6277 = CARTESIAN_POINT ( 'NONE',  ( 80.23208661909926320, 62.50324886901235999, 3.482780605906225624 ) ) ;
#6278 = AXIS2_PLACEMENT_3D ( 'NONE', #5187, #11949, #8867 ) ;
#6279 = CYLINDRICAL_SURFACE ( 'NONE', #37894, 0.09010775117052560734 ) ;
#6280 = CARTESIAN_POINT ( 'NONE',  ( 79.34209122208885390, 66.30884595491197331, 1.000000000000000000 ) ) ;
#6282 = ORIENTED_EDGE ( 'NONE', *, *, #10053, .T. ) ;
#6281 = CARTESIAN_POINT ( 'NONE',  ( 2.852772058385760534, -32.76869315680232830, 7.775108481317161591 ) ) ;
#6283 = CARTESIAN_POINT ( 'NONE',  ( 22.59998850301547790, -2.767621054697568361, -8.672491381162554802 ) ) ;
#6284 = CARTESIAN_POINT ( 'NONE',  ( 4.938390203311415748E-15, -42.37473357531882101, -2.500000000000000000 ) ) ;
#6285 = VERTEX_POINT ( 'NONE', #38214 ) ;
#6286 = CARTESIAN_POINT ( 'NONE',  ( -72.02191131938369040, 0.007829945179003310052, 9.944423546733684560 ) ) ;
#6287 = CARTESIAN_POINT ( 'NONE',  ( 33.45749450797183044, -3.829747548865578555, 5.093667367007288505 ) ) ;
#6288 = AXIS2_PLACEMENT_3D ( 'NONE', #12706, #23001, #6341 ) ;
#6289 = EDGE_CURVE ( 'NONE', #19079, #5789, #38414, .T. ) ;
#6290 = CARTESIAN_POINT ( 'NONE',  ( -1.519086612902572631, -28.17966245796219127, 7.387053503561888945 ) ) ;
#6291 = ORIENTED_EDGE ( 'NONE', *, *, #16389, .F. ) ;
#6292 = CARTESIAN_POINT ( 'NONE',  ( 5.401390093233090717, -29.44812577374269580, 7.754798119455333705 ) ) ;
#6293 = CARTESIAN_POINT ( 'NONE',  ( -4.444218661349752963, -35.94265729135299381, 6.000000000000000000 ) ) ;
#6294 = CARTESIAN_POINT ( 'NONE',  ( 33.11411321054668377, -0.1504196223776565200, -4.940960329838760323 ) ) ;
#6295 = CARTESIAN_POINT ( 'NONE',  ( 3.423404917024849059, -32.61643964784510530, 6.894806418505347700 ) ) ;
#6296 = CARTESIAN_POINT ( 'NONE',  ( 21.28478389403105098, 5.337957506763612692, 3.528403319744038313 ) ) ;
#6297 = DIRECTION ( 'NONE',  ( 1.000000000000000000, 0.000000000000000000, 0.000000000000000000 ) ) ;
#6298 = LINE ( 'NONE', #34322, #12825 ) ;
#6299 = FACE_OUTER_BOUND ( 'NONE', #20512, .T. ) ;
#6300 = DIRECTION ( 'NONE',  ( -1.000000000000000000, 0.000000000000000000, 0.000000000000000000 ) ) ;
#6301 = CARTESIAN_POINT ( 'NONE',  ( 21.84750790989929570, 0.3413277259319377754, -8.043973749180381105 ) ) ;
#6302 = CARTESIAN_POINT ( 'NONE',  ( 31.19141131379476306, -3.759815128464405021, -4.641892418952871857 ) ) ;
#6303 = CARTESIAN_POINT ( 'NONE',  ( 24.45511755102040752, 2.961865972188622020, -3.664620675852518161 ) ) ;
#6304 = ADVANCED_FACE ( 'NONE', ( #38819 ), #20090, .F. ) ;
#6305 = EDGE_LOOP ( 'NONE', ( #17678, #13196, #16388, #15364 ) ) ;
#6306 = CARTESIAN_POINT ( 'NONE',  ( 67.03255446809592399, 57.93006272621622088, 3.998453671246410934 ) ) ;
#6307 = CARTESIAN_POINT ( 'NONE',  ( 33.43848875257462083, -3.435003965559634942, 5.407914039447962118 ) ) ;
#6308 = AXIS2_PLACEMENT_3D ( 'NONE', #30399, #20499, #27295 ) ;
#6309 = DIRECTION ( 'NONE',  ( 1.000000000000000000, 0.000000000000000000, 0.000000000000000000 ) ) ;
#6310 = AXIS2_PLACEMENT_3D ( 'NONE', #23528, #7468, #36485 ) ;
#6311 = CARTESIAN_POINT ( 'NONE',  ( 86.59537683758360060, -0.3992097724244685342, -5.811584838773467432 ) ) ;
#6312 = CARTESIAN_POINT ( 'NONE',  ( 35.93014311948857653, -3.156885213570711723, -5.814165826228037126 ) ) ;
#6313 = DIRECTION ( 'NONE',  ( 1.000000000000000000, 0.000000000000000000, 0.000000000000000000 ) ) ;
#6314 = ORIENTED_EDGE ( 'NONE', *, *, #37553, .F. ) ;
#6315 = CARTESIAN_POINT ( 'NONE',  ( 24.43316465493469636, 2.958069255867872727, 3.679139778253121662 ) ) ;
#6316 = VECTOR ( 'NONE', #24301, 1000.000000000000000 ) ;
#6317 = CARTESIAN_POINT ( 'NONE',  ( -20.44874870218064444, -25.49307895267003587, 6.700000000000000178 ) ) ;
#6318 = EDGE_CURVE ( 'NONE', #446, #29043, #19618, .T. ) ;
#6319 = ORIENTED_EDGE ( 'NONE', *, *, #18792, .T. ) ;
#6320 = CARTESIAN_POINT ( 'NONE',  ( 5.150390093233091271, -29.56993018339339940, 7.800000000000000711 ) ) ;
#6321 = CYLINDRICAL_SURFACE ( 'NONE', #39952, 21.28220113893567245 ) ;
#6322 = ORIENTED_EDGE ( 'NONE', *, *, #1161, .F. ) ;
#6323 = ORIENTED_EDGE ( 'NONE', *, *, #34334, .F. ) ;
#6324 = CARTESIAN_POINT ( 'NONE',  ( 80.98019550867142868, 61.28820853408534219, -1.743126864185862601 ) ) ;
#6325 = CARTESIAN_POINT ( 'NONE',  ( -1.739421677191636872, -28.95442883120933786, 7.773839561854632763 ) ) ;
#6326 = CARTESIAN_POINT ( 'NONE',  ( 79.85475324883658743, 64.00275885990842539, 3.706996517075250797 ) ) ;
#6329 = VERTEX_POINT ( 'NONE', #974 ) ;
#6328 = ORIENTED_EDGE ( 'NONE', *, *, #20916, .T. ) ;
#6327 = FACE_OUTER_BOUND ( 'NONE', #1221, .T. ) ;
#6330 = CARTESIAN_POINT ( 'NONE',  ( 0.002375005847796004751, -26.52616241155169874, 7.785344483711591934 ) ) ;
#6331 = CARTESIAN_POINT ( 'NONE',  ( 25.13391170364226923, -5.621210998728720654, 2.945584106497509236 ) ) ;
#6332 = DIRECTION ( 'NONE',  ( -0.000000000000000000, -0.000000000000000000, -1.000000000000000000 ) ) ;
#6333 = EDGE_CURVE ( 'NONE', #26136, #19316, #32070, .T. ) ;
#6334 = ADVANCED_FACE ( 'NONE', ( #16989 ), #26081, .F. ) ;
#6335 = FACE_OUTER_BOUND ( 'NONE', #1880, .T. ) ;
#6336 = CARTESIAN_POINT ( 'NONE',  ( 22.88263960910827777, 4.299920287885681702, -3.109403903331433128 ) ) ;
#6337 = ORIENTED_EDGE ( 'NONE', *, *, #7818, .T. ) ;
#6338 = CARTESIAN_POINT ( 'NONE',  ( 4.826555071938813946, -30.90675198375193844, 7.013842709614101167 ) ) ;
#6339 = EDGE_CURVE ( 'NONE', #33687, #24034, #113, .T. ) ;
#6340 = ORIENTED_EDGE ( 'NONE', *, *, #33635, .F. ) ;
#6341 = DIRECTION ( 'NONE',  ( 1.000000000000000000, 0.000000000000000000, -0.000000000000000000 ) ) ;
#6342 = DIRECTION ( 'NONE',  ( -1.682730792515357087E-16, 1.000000000000000000, 0.000000000000000000 ) ) ;
#6343 = B_SPLINE_CURVE_WITH_KNOTS ( 'NONE', 3,
 ( #29220, #10267, #22847, #7586, #1030, #23633, #7978, #33118, #23048, #10862 ),
 .UNSPECIFIED., .F., .F.,
 ( 4, 3, 3, 4 ),
 ( 0.0001585009270395720371, 0.0001815657551981848989, 0.0002118214035944141318, 0.0002170292169044764612 ),
 .UNSPECIFIED. ) ;
#6344 = CARTESIAN_POINT ( 'NONE',  ( -77.62820146566370738, -4.987354577580212833, -7.432037137499030166 ) ) ;
#6345 = DIRECTION ( 'NONE',  ( 0.000000000000000000, 0.000000000000000000, -1.000000000000000000 ) ) ;
#6346 = CARTESIAN_POINT ( 'NONE',  ( 78.67891909395969208, 66.05044883183084892, 1.113695828830612022 ) ) ;
#6347 = CARTESIAN_POINT ( 'NONE',  ( 86.22674662394152278, 0.2046669357502599595, -6.014203425234573963 ) ) ;
#6348 = CARTESIAN_POINT ( 'NONE',  ( -0.01851169824090236754, -32.61876219438834568, 7.700536657684222241 ) ) ;
#6349 = ORIENTED_EDGE ( 'NONE', *, *, #5523, .T. ) ;
#6350 = DIRECTION ( 'NONE',  ( -0.000000000000000000, -0.000000000000000000, -1.000000000000000000 ) ) ;
#6351 = CARTESIAN_POINT ( 'NONE',  ( -69.08758708074093136, 36.88538962427716683, 9.800414904976364028 ) ) ;
#6352 = AXIS2_PLACEMENT_3D ( 'NONE', #34950, #10408, #38808 ) ;
#6353 = CIRCLE ( 'NONE', #37890, 3.000000000000003997 ) ;
#6354 = VERTEX_POINT ( 'NONE', #22996 ) ;
#6355 = PLANE ( 'NONE',  #683 ) ;
#6356 = CARTESIAN_POINT ( 'NONE',  ( 0.3454438073187346969, 0.5999999999999995337, 3.946157045896963034 ) ) ;
#6357 = CARTESIAN_POINT ( 'NONE',  ( -72.46964309959683703, 39.11862660440054640, 15.50000000000000000 ) ) ;
#6358 = DIRECTION ( 'NONE',  ( 0.000000000000000000, 0.000000000000000000, -1.000000000000000000 ) ) ;
#6359 = ORIENTED_EDGE ( 'NONE', *, *, #12832, .F. ) ;
#6360 = CARTESIAN_POINT ( 'NONE',  ( 35.86856226912744461, -2.087698133915266929, 5.804554645190663997 ) ) ;
#6361 = CARTESIAN_POINT ( 'NONE',  ( 87.66750401967712492, -0.1145768689462967616, 4.387407120178886899 ) ) ;
#6362 = ORIENTED_EDGE ( 'NONE', *, *, #3882, .T. ) ;
#6364 = CARTESIAN_POINT ( 'NONE',  ( 14.70526687707813629, -5.034966368804535186, 2.499999999999956035 ) ) ;
#6363 = CARTESIAN_POINT ( 'NONE',  ( 80.03809576917892343, 64.85583152007153274, -3.406228740995818516 ) ) ;
#6365 = DIRECTION ( 'NONE',  ( 1.000000000000000000, 8.966158204770716457E-16, 0.000000000000000000 ) ) ;
#6366 = VERTEX_POINT ( 'NONE', #769 ) ;
#6367 = CARTESIAN_POINT ( 'NONE',  ( 24.97507460369484278, -5.746002789830511936, -2.897263417418799669 ) ) ;
#6368 = ADVANCED_FACE ( 'NONE', ( #7136 ), #1183, .T. ) ;
#6369 = ORIENTED_EDGE ( 'NONE', *, *, #36472, .T. ) ;
#6370 = CARTESIAN_POINT ( 'NONE',  ( -71.81426791222166628, 3.509262911811426022, 9.960721438266951111 ) ) ;
#6372 = ORIENTED_EDGE ( 'NONE', *, *, #18388, .T. ) ;
#6371 = ORIENTED_EDGE ( 'NONE', *, *, #38462, .F. ) ;
#6373 = CARTESIAN_POINT ( 'NONE',  ( 78.78378587176688086, 65.95784816145936702, -1.911132874451719754 ) ) ;
#6374 =( BOUNDED_CURVE ( )  B_SPLINE_CURVE ( 3, ( #2357, #31160, #11774, #40398 ),
 .UNSPECIFIED., .F., .T. ) 
 B_SPLINE_CURVE_WITH_KNOTS ( ( 4, 4 ),
 ( 4.748221474220558846, 4.941946782021393147 ),
 .UNSPECIFIED. ) 
 CURVE ( )  GEOMETRIC_REPRESENTATION_ITEM ( )  RATIONAL_B_SPLINE_CURVE ( ( 1.000000000000000000, 0.9968749865767494445, 0.9968749865767494445, 1.000000000000000000 ) ) 
 REPRESENTATION_ITEM ( '' )  );
#6375 = AXIS2_PLACEMENT_3D ( 'NONE', #35302, #28904, #9549 ) ;
#6376 = CARTESIAN_POINT ( 'NONE',  ( 35.97003858198674209, -3.154676479323113458, 5.820392478026279903 ) ) ;
#6377 = VECTOR ( 'NONE', #4372, 1000.000000000000000 ) ;
#6379 = CARTESIAN_POINT ( 'NONE',  ( 20.94977919345308948, 9.634852852900486653, -2.522469388968830994 ) ) ;
#6378 = CARTESIAN_POINT ( 'NONE',  ( 23.38749234610577687, 2.689796015418254083, 4.224764990934100517 ) ) ;
#6380 = ORIENTED_EDGE ( 'NONE', *, *, #3078, .F. ) ;
#6381 = EDGE_CURVE ( 'NONE', #19379, #16251, #11612, .T. ) ;
#6382 = AXIS2_PLACEMENT_3D ( 'NONE', #21703, #18801, #31577 ) ;
#6383 = EDGE_CURVE ( 'NONE', #18497, #20724, #32866, .T. ) ;
#6384 = LINE ( 'NONE', #31497, #19992 ) ;
#6386 = PLANE ( 'NONE',  #18323 ) ;
#6385 = PLANE ( 'NONE',  #39715 ) ;
#6387 = LINE ( 'NONE', #9451, #15895 ) ;
#6388 = CARTESIAN_POINT ( 'NONE',  ( -63.23384002544804616, 41.81976959235312563, -3.940701001627876288 ) ) ;
#6389 = CARTESIAN_POINT ( 'NONE',  ( 73.33417617461327609, 60.23131181272744072, 3.934110468510651604 ) ) ;
#6390 = CARTESIAN_POINT ( 'NONE',  ( 22.02121393394833149, 4.117315833306967932, -4.097082391610725516 ) ) ;
#6391 = ADVANCED_FACE ( 'NONE', ( #29757 ), #7931, .F. ) ;
#6392 = CARTESIAN_POINT ( 'NONE',  ( 21.85643539959775694, 0.6980322203039187601, 15.81276153107902616 ) ) ;
#6393 = CARTESIAN_POINT ( 'NONE',  ( 3.509071552096934443, -26.58788102988029323, 7.782861076432732617 ) ) ;
#6394 = CARTESIAN_POINT ( 'NONE',  ( 1.057972185589858727, -26.12939249603516245, 7.710604733652629328 ) ) ;
#6395 = CARTESIAN_POINT ( 'NONE',  ( 81.36533387373953019, 61.41589781867489251, 1.313329331391811960 ) ) ;
#6396 = CARTESIAN_POINT ( 'NONE',  ( 85.93841924537714760, 1.827613216861550205, 4.619486236290579306 ) ) ;
#6397 = EDGE_LOOP ( 'NONE', ( #6262, #32989, #37823, #39991, #31309, #30804 ) ) ;
#6398 = EDGE_CURVE ( 'NONE', #530, #35439, #2401, .T. ) ;
#6399 = CARTESIAN_POINT ( 'NONE',  ( 14.65885757255257893, 12.91887598177978624, 2.499999999999996891 ) ) ;
#6400 = CARTESIAN_POINT ( 'NONE',  ( 28.88870942992270940, -3.138682824899541313, 4.706547700740843609 ) ) ;
#6401 = AXIS2_PLACEMENT_3D ( 'NONE', #4474, #7541, #20289 ) ;
#6402 = CARTESIAN_POINT ( 'NONE',  ( 37.04571469918683135, -2.801042461011243212, -5.988277751440494789 ) ) ;
#6403 = CARTESIAN_POINT ( 'NONE',  ( -1.341696911977036555, -27.83911289459152627, 7.743886751744255115 ) ) ;
#6404 = CARTESIAN_POINT ( 'NONE',  ( 4.404419331614843003, -31.79214211702542769, 7.700536657684215136 ) ) ;
#6405 = ORIENTED_EDGE ( 'NONE', *, *, #40286, .T. ) ;
#6406 = AXIS2_PLACEMENT_3D ( 'NONE', #37633, #33618, #36887 ) ;
#6407 = CARTESIAN_POINT ( 'NONE',  ( -1.249667454803414124, -31.26026423822809974, 7.775108481317162479 ) ) ;
#6408 = VERTEX_POINT ( 'NONE', #11209 ) ;
#6409 = ORIENTED_EDGE ( 'NONE', *, *, #17137, .T. ) ;
#6410 = CARTESIAN_POINT ( 'NONE',  ( 35.72972106090838906, -1.305514564919402432, 5.539022487619330803 ) ) ;
#6411 = FACE_OUTER_BOUND ( 'NONE', #5357, .T. ) ;
#6412 = EDGE_LOOP ( 'NONE', ( #6894, #22846, #12491, #36115 ) ) ;
#6413 = CARTESIAN_POINT ( 'NONE',  ( 66.41802798480571823, 57.80214248194123172, -4.000000000000020428 ) ) ;
#6414 = EDGE_CURVE ( 'NONE', #19825, #36582, #14796, .T. ) ;
#6415 = VERTEX_POINT ( 'NONE', #14103 ) ;
#6416 = CARTESIAN_POINT ( 'NONE',  ( 87.04213330793400871, 0.5878691963681514920, -4.891134986362597914 ) ) ;
#6417 = CARTESIAN_POINT ( 'NONE',  ( -80.91065676098010329, -6.597313057213482601, -0.5950503846463383040 ) ) ;
#6418 = CARTESIAN_POINT ( 'NONE',  ( -1.652426028059061025, -33.50972191341452344, 7.695279973900954751 ) ) ;
#6419 = CARTESIAN_POINT ( 'NONE',  ( -17.27251170661583402, 0.7293679304675921848, -6.000000000000000000 ) ) ;
#6420 = FACE_BOUND ( 'NONE', #19084, .T. ) ;
#6421 = DIRECTION ( 'NONE',  ( -0.000000000000000000, -0.000000000000000000, -1.000000000000000000 ) ) ;
#6422 = ORIENTED_EDGE ( 'NONE', *, *, #37378, .F. ) ;
#6423 = B_SPLINE_CURVE_WITH_KNOTS ( 'NONE', 3,
 ( #25994, #35675, #13833, #1295, #29082, #10334, #22907, #29282, #13631, #20004 ),
 .UNSPECIFIED., .F., .F.,
 ( 4, 3, 3, 4 ),
 ( 0.0002170292169044812859, 0.0002420761345915979352, 0.0002723302478207015580, 0.0002816811360866826016 ),
 .UNSPECIFIED. ) ;
#6424 = CARTESIAN_POINT ( 'NONE',  ( 80.67264098608434608, 66.18930038384912962, -1.451695327222927157 ) ) ;
#6425 = CARTESIAN_POINT ( 'NONE',  ( 78.91303925368887917, 65.86465164089241853, 2.189516896894255549 ) ) ;
#6426 = AXIS2_PLACEMENT_3D ( 'NONE', #5931, #15182, #2866 ) ;
#6427 = CARTESIAN_POINT ( 'NONE',  ( -70.31344945295795412, -21.58221595790078950, 3.969121680884525105 ) ) ;
#6428 = ORIENTED_EDGE ( 'NONE', *, *, #15119, .F. ) ;
#6429 = CARTESIAN_POINT ( 'NONE',  ( 76.81831744871801959, 63.08285468194212342, -3.722835383484654592 ) ) ;
#6431 = DIRECTION ( 'NONE',  ( 0.000000000000000000, 0.000000000000000000, 1.000000000000000000 ) ) ;
#6430 = CARTESIAN_POINT ( 'NONE',  ( 3.939802142412995423, -32.25249995964913552, 7.773839561854632763 ) ) ;
#6432 = CARTESIAN_POINT ( 'NONE',  ( 16.93405020700152264, 9.102874499958653942, -2.849366104991231996 ) ) ;
#6433 = AXIS2_PLACEMENT_3D ( 'NONE', #7120, #19683, #38994 ) ;
#6434 = CARTESIAN_POINT ( 'NONE',  ( 78.79418933159148253, 66.09338072887959470, -1.439474762807432695 ) ) ;
#6435 = DIRECTION ( 'NONE',  ( 0.000000000000000000, 0.000000000000000000, 1.000000000000000000 ) ) ;
#6436 = CARTESIAN_POINT ( 'NONE',  ( 79.66869450427635968, 60.77384974161341091, 2.178915381671341578 ) ) ;
#6437 = AXIS2_PLACEMENT_3D ( 'NONE', #10485, #14181, #23065 ) ;
#6438 = EDGE_LOOP ( 'NONE', ( #22855, #38440, #10052, #14557, #25400 ) ) ;
#6439 = AXIS2_PLACEMENT_3D ( 'NONE', #5046, #29747, #36339 ) ;
#6440 = EDGE_CURVE ( 'NONE', #30761, #29356, #38641, .T. ) ;
#6441 = EDGE_CURVE ( 'NONE', #25138, #15211, #28813, .T. ) ;
#6442 = DIRECTION ( 'NONE',  ( 1.000000000000000000, 0.000000000000000000, 0.000000000000000000 ) ) ;
#6443 = EDGE_CURVE ( 'NONE', #614, #3701, #24158, .T. ) ;
#6444 = CARTESIAN_POINT ( 'NONE',  ( 0.5364714774190757485, -32.87073217714502249, 7.710604733652624887 ) ) ;
#6445 = CARTESIAN_POINT ( 'NONE',  ( 80.79165360588685019, 65.97001311340693519, 2.094266784918907831 ) ) ;
#6447 = CARTESIAN_POINT ( 'NONE',  ( -1.698039391944944576, -29.46606476191993096, 6.864651958020303368 ) ) ;
#6446 = CARTESIAN_POINT ( 'NONE',  ( -0.3385372945680173995, -26.84912605459717838, 7.013842709614101167 ) ) ;
#6448 = CARTESIAN_POINT ( 'NONE',  ( 26.86540377008237357, 1.668949755151340586, -4.708546860826485769 ) ) ;
#6449 = CARTESIAN_POINT ( 'NONE',  ( -1.432293644835494373, -27.47664038617742577, 1.000000000000000000 ) ) ;
#6450 = PLANE ( 'NONE',  #356 ) ;
#6451 = CARTESIAN_POINT ( 'NONE',  ( 1.529222282396958787, -33.06574276064830542, 7.011627023500184741 ) ) ;
#6452 = CARTESIAN_POINT ( 'NONE',  ( 1.700390093233090871, -29.56993018339339940, 7.750000000000000888 ) ) ;
#6453 = VERTEX_POINT ( 'NONE', #40041 ) ;
#6454 = DIRECTION ( 'NONE',  ( 1.000000000000000000, 0.000000000000000000, 0.000000000000000000 ) ) ;
#6455 = CARTESIAN_POINT ( 'NONE',  ( -36.44874870218064444, -26.64985754041175525, 6.700000000000000178 ) ) ;
#6456 = CARTESIAN_POINT ( 'NONE',  ( -71.90176653367559823, -0.5198039855910460139, 3.920732911925276287 ) ) ;
#6457 = CARTESIAN_POINT ( 'NONE',  ( 36.98471844170311584, -3.196209668142826921, -5.957689647507654840 ) ) ;
#6458 = PLANE ( 'NONE',  #18725 ) ;
#6459 = CARTESIAN_POINT ( 'NONE',  ( 4.364743062397921314, -27.30029760200210731, 7.737115613922533441 ) ) ;
#6460 = CARTESIAN_POINT ( 'NONE',  ( 0.3896649785617538608, -32.81498557016907114, 7.754798119455333705 ) ) ;
#6461 = CARTESIAN_POINT ( 'NONE',  ( -20.87867591359218977, -26.64985754041175525, 6.800000000000000711 ) ) ;
#6462 = CARTESIAN_POINT ( 'NONE',  ( 2.147015419475138298, -32.94046809565001865, 6.868387053540521592 ) ) ;
#6463 = CARTESIAN_POINT ( 'NONE',  ( -24.87867591359218977, -24.55319635012989110, 6.700000000000000178 ) ) ;
#6464 = VECTOR ( 'NONE', #33645, 1000.000000000000227 ) ;
#6465 = CARTESIAN_POINT ( 'NONE',  ( -1.484082617398029491, -28.37865626222930260, 7.782167645815904145 ) ) ;
#6466 = CARTESIAN_POINT ( 'NONE',  ( -1.511717022306371616, -30.68454846542563175, 6.892063359921933419 ) ) ;
#6467 = ORIENTED_EDGE ( 'NONE', *, *, #35682, .T. ) ;
#6468 = ORIENTED_EDGE ( 'NONE', *, *, #11786, .T. ) ;
#6469 = DIRECTION ( 'NONE',  ( 0.000000000000000000, 0.000000000000000000, 1.000000000000000000 ) ) ;
#6470 = AXIS2_PLACEMENT_3D ( 'NONE', #8776, #37197, #24860 ) ;
#6471 = CARTESIAN_POINT ( 'NONE',  ( 68.79143787039059532, 58.12720587843082853, -3.950303728398663949 ) ) ;
#6472 = VERTEX_POINT ( 'NONE', #36750 ) ;
#6473 = CARTESIAN_POINT ( 'NONE',  ( -0.9135791104145147834, -27.25323683387426144, 7.776484688137384360 ) ) ;
#6474 = FACE_OUTER_BOUND ( 'NONE', #25608, .T. ) ;
#6475 = CARTESIAN_POINT ( 'NONE',  ( 21.84156485433835471, 4.525468657295988351, 4.021517308586185280 ) ) ;
#6476 = DIRECTION ( 'NONE',  ( -0.000000000000000000, -0.000000000000000000, -1.000000000000000000 ) ) ;
#6477 = DIRECTION ( 'NONE',  ( -0.000000000000000000, -1.000000000000000000, -0.000000000000000000 ) ) ;
#6478 = ORIENTED_EDGE ( 'NONE', *, *, #3719, .F. ) ;
#6479 = CARTESIAN_POINT ( 'NONE',  ( 24.40779208807497369, 3.164677091567920542, 3.266067496624623256 ) ) ;
#6480 = DIRECTION ( 'NONE',  ( 0.6427876096865379196, 0.7660444431189792347, -0.000000000000000000 ) ) ;
#6481 = ORIENTED_EDGE ( 'NONE', *, *, #27065, .F. ) ;
#6482 = FACE_OUTER_BOUND ( 'NONE', #38538, .T. ) ;
#6483 = ORIENTED_EDGE ( 'NONE', *, *, #24625, .F. ) ;
#6484 = CARTESIAN_POINT ( 'NONE',  ( 78.40723131619293440, 65.41550730244513545, -2.551437666014013672 ) ) ;
#6485 = CIRCLE ( 'NONE', #29491, 0.1000000000000028644 ) ;
#6487 = CARTESIAN_POINT ( 'NONE',  ( -1.003736583562490070, -27.34783681995376270, 7.695279973900954751 ) ) ;
#6486 = CARTESIAN_POINT ( 'NONE',  ( 21.73675671614552485, 0.3116768600389830390, 8.862532426860488144 ) ) ;
#6488 = CARTESIAN_POINT ( 'NONE',  ( 81.52287143523912505, 61.74508502528950515, -1.930361577749144519 ) ) ;
#6489 = CARTESIAN_POINT ( 'NONE',  ( 80.75587274821523920, 61.22306450394816579, 1.910479420724444433 ) ) ;
#6490 = ORIENTED_EDGE ( 'NONE', *, *, #4660, .F. ) ;
#6491 = EDGE_CURVE ( 'NONE', #26477, #9234, #30592, .T. ) ;
#6492 = ADVANCED_FACE ( 'NONE', ( #39216 ), #17383, .F. ) ;
#6493 = CARTESIAN_POINT ( 'NONE',  ( -1.612909802052744812, -30.67534724370283783, 7.776484688137385248 ) ) ;
#6494 = CARTESIAN_POINT ( 'NONE',  ( 1.887380280259158383, -26.17507603778478753, 7.013842709614101167 ) ) ;
#6495 = CARTESIAN_POINT ( 'NONE',  ( 22.34899403049013245, 4.475801132629629642, -6.347516269785208998 ) ) ;
#6496 = CARTESIAN_POINT ( 'NONE',  ( 1.574364539997139767, -33.06766052747819629, 7.750000000000000888 ) ) ;
#6497 = VERTEX_POINT ( 'NONE', #31200 ) ;
#6498 = CARTESIAN_POINT ( 'NONE',  ( -73.25168990586664108, 4.982336816971301374, 10.91515532190027571 ) ) ;
#6499 = ORIENTED_EDGE ( 'NONE', *, *, #12745, .T. ) ;
#6500 = VECTOR ( 'NONE', #37368, 1000.000000000000000 ) ;
#6501 = CARTESIAN_POINT ( 'NONE',  ( -0.1082913656307287614, -32.55197933690651979, 7.782861076432731728 ) ) ;
#6502 = ORIENTED_EDGE ( 'NONE', *, *, #7442, .T. ) ;
#6503 = CARTESIAN_POINT ( 'NONE',  ( 1.705817689846350405, -32.96993596345505750, 7.763628509615286610 ) ) ;
#6504 = CARTESIAN_POINT ( 'NONE',  ( 33.45777346496446825, -3.169730459255029054, -5.428292747153331099 ) ) ;
#6505 = CARTESIAN_POINT ( 'NONE',  ( 25.73534323679438174, 2.638937876048334630, -3.514020203366912121 ) ) ;
#6506 = CARTESIAN_POINT ( 'NONE',  ( -1.558322435399049244, -30.53987484972025612, 6.988553391373226731 ) ) ;
#6507 = FACE_OUTER_BOUND ( 'NONE', #3570, .T. ) ;
#6508 = CARTESIAN_POINT ( 'NONE',  ( 22.17103036364695257, 4.944193875442659980, 3.666723515279467271 ) ) ;
#6509 = CARTESIAN_POINT ( 'NONE',  ( -0.06636395565068713143, -26.54857616064916570, 7.643192810543817828 ) ) ;
#6510 = CARTESIAN_POINT ( 'NONE',  ( -65.15514661499977933, 34.97220226750606997, -6.888442104241536690 ) ) ;
#6511 = DIRECTION ( 'NONE',  ( 1.000000000000000000, 0.000000000000000000, 0.000000000000000000 ) ) ;
#6512 = DIRECTION ( 'NONE',  ( -0.000000000000000000, -0.000000000000000000, -1.000000000000000000 ) ) ;
#6513 = CARTESIAN_POINT ( 'NONE',  ( 22.52933421130244795, 0.9543590913064874393, -6.221134177511584262 ) ) ;
#6514 = CARTESIAN_POINT ( 'NONE',  ( 1.277170166547874075, -33.05113105426861608, 7.139344958878411695 ) ) ;
#6515 = CIRCLE ( 'NONE', #7144, 0.1000000000000028644 ) ;
#6516 = DIRECTION ( 'NONE',  ( 0.000000000000000000, 1.000000000000000000, 0.000000000000000000 ) ) ;
#6517 = ORIENTED_EDGE ( 'NONE', *, *, #20967, .F. ) ;
#6518 = CARTESIAN_POINT ( 'NONE',  ( 67.46313568882432321, 58.11475875142180314, 3.998123450764770048 ) ) ;
#6519 = CARTESIAN_POINT ( 'NONE',  ( 36.24022540957366090, -2.130119347149664222, 5.862561666964295704 ) ) ;
#6520 = EDGE_CURVE ( 'NONE', #32354, #12694, #40432, .T. ) ;
#6521 = CARTESIAN_POINT ( 'NONE',  ( 2.199298596665589134, -33.03157230968192692, 7.766640943994644886 ) ) ;
#6522 = CARTESIAN_POINT ( 'NONE',  ( 86.69339609521894374, -0.1977197225095213562, 5.906572220802119411 ) ) ;
#6523 = LINE ( 'NONE', #34134, #19133 ) ;
#6524 = VERTEX_POINT ( 'NONE', #3020 ) ;
#6525 = CARTESIAN_POINT ( 'NONE',  ( 25.44052111716949582, 2.260287636792247756, 4.091035459148633535 ) ) ;
#6526 = CARTESIAN_POINT ( 'NONE',  ( 5.200390093233089317, -29.56542930052595608, 7.625529684960262067 ) ) ;
#6527 = DIRECTION ( 'NONE',  ( 0.000000000000000000, -0.7541618601367562347, -0.6566885781822823231 ) ) ;
#6528 = ORIENTED_EDGE ( 'NONE', *, *, #11372, .F. ) ;
#6529 =( LENGTH_UNIT ( ) NAMED_UNIT ( * ) SI_UNIT ( .MILLI., .METRE. ) );
#6530 = EDGE_CURVE ( 'NONE', #3202, #18044, #15746, .T. ) ;
#6531 = UNCERTAINTY_MEASURE_WITH_UNIT (LENGTH_MEASURE( 1.000000000000000082E-05 ), #39307, 'distance_accuracy_value', 'NONE');
#6532 = VERTEX_POINT ( 'NONE', #12450 ) ;
#6533 = CARTESIAN_POINT ( 'NONE',  ( 79.07938959848800664, 65.20837507400351285, -3.070011659370644796 ) ) ;
#6534 = LINE ( 'NONE', #27927, #32594 ) ;
#6535 = CARTESIAN_POINT ( 'NONE',  ( 80.65652637675404435, 62.34602738889181950, 3.260928702718590699 ) ) ;
#6538 = ORIENTED_EDGE ( 'NONE', *, *, #32161, .F. ) ;
#6537 = ORIENTED_EDGE ( 'NONE', *, *, #25890, .F. ) ;
#6536 = CARTESIAN_POINT ( 'NONE',  ( -1.338646324113869968, -31.09448676743746631, 6.997764925645180156 ) ) ;
#6539 = CARTESIAN_POINT ( 'NONE',  ( -58.98413297244930931, 28.20303297481065385, 6.383932851085149629 ) ) ;
#6540 = EDGE_CURVE ( 'NONE', #19833, #32450, #29546, .T. ) ;
#6541 = CARTESIAN_POINT ( 'NONE',  ( -0.5222764122352709926, -32.27358584779708650, 7.710604733652632881 ) ) ;
#6542 = DIRECTION ( 'NONE',  ( 0.6662082868431823401, 0.000000000000000000, -0.7457657263118706581 ) ) ;
#6543 = CARTESIAN_POINT ( 'NONE',  ( 14.61802081865033820, -4.461849342347350422, 2.500000000000000000 ) ) ;
#6544 = CARTESIAN_POINT ( 'NONE',  ( 24.03936073869400403, 3.329292850658597036, -3.281681657426043675 ) ) ;
#6545 = ORIENTED_EDGE ( 'NONE', *, *, #32505, .F. ) ;
#6546 = LINE ( 'NONE', #31258, #26177 ) ;
#6547 = VERTEX_POINT ( 'NONE', #6494 ) ;
#6548 = CARTESIAN_POINT ( 'NONE',  ( -1.027740059687268559, -31.59904846300154446, 6.997764925645181933 ) ) ;
#6549 = CARTESIAN_POINT ( 'NONE',  ( -1.652310497857324201, -29.00476380710052382, 7.652160403243381204 ) ) ;
#6550 = CARTESIAN_POINT ( 'NONE',  ( -80.59239215695774305, -6.629469220045966615, -2.601833008578107620 ) ) ;
#6551 = DIRECTION ( 'NONE',  ( 1.000000000000000000, 0.000000000000000000, 0.000000000000000000 ) ) ;
#6552 = DIRECTION ( 'NONE',  ( 0.000000000000000000, 0.000000000000000000, -1.000000000000000000 ) ) ;
#6553 = CARTESIAN_POINT ( 'NONE',  ( 81.15350626233055209, 61.29809656771022475, 1.122020883098631350 ) ) ;
#6554 = CARTESIAN_POINT ( 'NONE',  ( 86.84125380892929513, -1.134812445414097981, 5.244953511127716794 ) ) ;
#6555 = CARTESIAN_POINT ( 'NONE',  ( -0.02444159985243907554, -32.61541136549380582, 7.730015791551954507 ) ) ;
#6556 = VERTEX_POINT ( 'NONE', #34715 ) ;
#6557 = CARTESIAN_POINT ( 'NONE',  ( -9.741734729663692249, 54.65020406074287251, -4.000000000000000000 ) ) ;
#6558 = CARTESIAN_POINT ( 'NONE',  ( 22.07282434680287153, 4.440933931123326239, -0.7814465169830903113 ) ) ;
#6559 = VECTOR ( 'NONE', #16747, 1000.000000000000000 ) ;
#6560 = CARTESIAN_POINT ( 'NONE',  ( 1.760763344459050472, -26.17046624469124083, 7.785172627573962778 ) ) ;
#6561 = LINE ( 'NONE', #390, #37033 ) ;
#6562 = CARTESIAN_POINT ( 'NONE',  ( 4.627388605110565933, -27.83999205693219636, 7.712764235869106422 ) ) ;
#6563 = CARTESIAN_POINT ( 'NONE',  ( 85.76727974192220927, 0.6799405750822806738, 5.934655056445743426 ) ) ;
#6564 = VERTEX_POINT ( 'NONE', #15330 ) ;
#6565 = CARTESIAN_POINT ( 'NONE',  ( 36.99247513494067618, -2.719144141632455103, 5.979968429836247878 ) ) ;
#6566 = CARTESIAN_POINT ( 'NONE',  ( 86.99908277331161344, 0.6362256001576577225, -5.325422653610870860 ) ) ;
#6567 = AXIS2_PLACEMENT_3D ( 'NONE', #27592, #37054, #25123 ) ;
#6568 = ORIENTED_EDGE ( 'NONE', *, *, #6574, .F. ) ;
#6570 = CARTESIAN_POINT ( 'NONE',  ( 29.49009503893727313, 1.222200888372551253, 4.216489851707110326 ) ) ;
#6569 = CARTESIAN_POINT ( 'NONE',  ( 79.47520324823359772, 65.51774519012143116, -2.899379378185757528 ) ) ;
#6571 = ADVANCED_FACE ( 'NONE', ( #37556 ), #36956, .T. ) ;
#6572 = CARTESIAN_POINT ( 'NONE',  ( 5.199086758562380339, -29.56349144210750168, 7.762460296495606649 ) ) ;
#6573 = ORIENTED_EDGE ( 'NONE', *, *, #1367, .T. ) ;
#6574 = EDGE_CURVE ( 'NONE', #3561, #3356, #40673, .T. ) ;
#6575 = CARTESIAN_POINT ( 'NONE',  ( -1.654012860102806570, -29.01496998062980381, 7.695279973900954751 ) ) ;
#6576 = CARTESIAN_POINT ( 'NONE',  ( -0.4624984080477824722, -26.82151441493339306, 7.766640943994646662 ) ) ;
#6577 = ORIENTED_EDGE ( 'NONE', *, *, #23602, .T. ) ;
#6578 = CARTESIAN_POINT ( 'NONE',  ( -72.02865492783033119, 4.746890789902021623, 9.939612967181826519 ) ) ;
#6579 = ORIENTED_EDGE ( 'NONE', *, *, #10559, .T. ) ;
#6580 = CARTESIAN_POINT ( 'NONE',  ( 79.95371652093496095, 64.44169929929478258, -3.600689860192760605 ) ) ;
#6581 = DIRECTION ( 'NONE',  ( 0.000000000000000000, 0.000000000000000000, 1.000000000000000000 ) ) ;
#6583 = CARTESIAN_POINT ( 'NONE',  ( 37.17836410518969359, -2.593987027605573203, 5.983491823951893274 ) ) ;
#6582 = CARTESIAN_POINT ( 'NONE',  ( 22.52364110764304428, 1.987705025956313598, 5.323102857299951474 ) ) ;
#6585 = ORIENTED_EDGE ( 'NONE', *, *, #24126, .F. ) ;
#6584 = VERTEX_POINT ( 'NONE', #9562 ) ;
#6586 = CARTESIAN_POINT ( 'NONE',  ( 81.88652354500518982, 62.08144837224592294, -1.918505602738485027 ) ) ;
#6587 = DIRECTION ( 'NONE',  ( -0.8660254037844415942, 0.4999999999999950040, -0.000000000000000000 ) ) ;
#6588 = CARTESIAN_POINT ( 'NONE',  ( -77.95330471031414277, 33.71485196875532608, -46.17089178453873188 ) ) ;
#6589 = ADVANCED_FACE ( 'NONE', ( #9351 ), #33893, .F. ) ;
#6591 = CARTESIAN_POINT ( 'NONE',  ( 86.34446901633954496, 1.371518841831834701, -4.801737237486140231 ) ) ;
#6590 = CARTESIAN_POINT ( 'NONE',  ( -72.42837670882107659, -47.11702805680359063, 9.886859966642603581 ) ) ;
#6592 = DIRECTION ( 'NONE',  ( -0.9848077530122067991, -0.1736481776669374644, -0.000000000000000000 ) ) ;
#6593 = CARTESIAN_POINT ( 'NONE',  ( 5.200390093233090205, -29.36153111629380774, 7.162856560672870465 ) ) ;
#6594 = CARTESIAN_POINT ( 'NONE',  ( 71.29558780583862188, 58.60460498947428931, 3.808711916423244581 ) ) ;
#6595 = CARTESIAN_POINT ( 'NONE',  ( 24.11329568594008421, 3.020242353435997895, -3.707757905648319419 ) ) ;
#6596 = ORIENTED_EDGE ( 'NONE', *, *, #37720, .T. ) ;
#6597 = VERTEX_POINT ( 'NONE', #21318 ) ;
#6598 = CARTESIAN_POINT ( 'NONE',  ( 21.85643539959774273, -6.795129563591141064, 12.90182208710982259 ) ) ;
#6599 = AXIS2_PLACEMENT_3D ( 'NONE', #23451, #2416, #20347 ) ;
#6600 = CARTESIAN_POINT ( 'NONE',  ( -58.67278899370590040, 29.89537120981031393, -5.422835840279424779 ) ) ;
#6601 = CARTESIAN_POINT ( 'NONE',  ( 1.057393818175778932, -26.12950058953997612, 7.700536657684216912 ) ) ;
#6602 = CARTESIAN_POINT ( 'NONE',  ( 81.73261497063184322, 63.12224843555917886, 2.914706979937429665 ) ) ;
#6603 = CARTESIAN_POINT ( 'NONE',  ( 85.57721755140556752, 2.175474006149249018, 4.430974418963669059 ) ) ;
#6604 = VERTEX_POINT ( 'NONE', #37753 ) ;
#6605 = CARTESIAN_POINT ( 'NONE',  ( 0.4903620891694951966, -32.74734004133340903, 7.785868773668302545 ) ) ;
#6606 = CARTESIAN_POINT ( 'NONE',  ( 18.26218337247781420, -3.004532202463449764, 3.045102850035385611 ) ) ;
#6607 = CARTESIAN_POINT ( 'NONE',  ( 34.77297214516959656, -3.162885276882883900, -5.633561309399683914 ) ) ;
#6608 = CARTESIAN_POINT ( 'NONE',  ( 5.100305588748021535, -29.54523758825880364, 7.740055089680398126 ) ) ;
#6609 = CARTESIAN_POINT ( 'NONE',  ( 1.653914865439267912, -33.89923146551851829, 6.954324564059724878 ) ) ;
#6610 = CARTESIAN_POINT ( 'NONE',  ( -42.83131703149249603, -27.06993018339339585, 6.800000000000000711 ) ) ;
#6611 = AXIS2_PLACEMENT_3D ( 'NONE', #15556, #6300, #14940 ) ;
#6612 = CYLINDRICAL_SURFACE ( 'NONE', #15856, 0.1000000000000028644 ) ;
#6613 = CARTESIAN_POINT ( 'NONE',  ( 28.28279320485486181, -3.656816081275314545, 4.586715715233614432 ) ) ;
#6614 = EDGE_LOOP ( 'NONE', ( #12890, #1464, #34820, #26927 ) ) ;
#6615 = CARTESIAN_POINT ( 'NONE',  ( 34.79219435089648016, -3.832416447686303851, 5.379528067116686074 ) ) ;
#6616 =( BOUNDED_CURVE ( )  B_SPLINE_CURVE ( 3, ( #1918, #8055, #20614, #33200 ),
 .UNSPECIFIED., .F., .T. ) 
 B_SPLINE_CURVE_WITH_KNOTS ( ( 4, 4 ),
 ( 4.748221474220559735, 4.941946782021394036 ),
 .UNSPECIFIED. ) 
 CURVE ( )  GEOMETRIC_REPRESENTATION_ITEM ( )  RATIONAL_B_SPLINE_CURVE ( ( 1.000000000000000000, 0.9968749865767494445, 0.9968749865767494445, 1.000000000000000000 ) ) 
 REPRESENTATION_ITEM ( '' )  );
#6617 = LINE ( 'NONE', #653, #16564 ) ;
#6618 = ORIENTED_EDGE ( 'NONE', *, *, #7134, .F. ) ;
#6619 = CARTESIAN_POINT ( 'NONE',  ( 66.42594280077625513, 57.77978248037106823, -4.000000000000013323 ) ) ;
#6620 = EDGE_CURVE ( 'NONE', #34388, #8430, #36470, .T. ) ;
#6621 = ORIENTED_EDGE ( 'NONE', *, *, #12745, .F. ) ;
#6622 = CARTESIAN_POINT ( 'NONE',  ( -55.97227462678463183, 30.94442605972621507, 3.900682954687266779 ) ) ;
#6623 = CIRCLE ( 'NONE', #15154, 0.1000000000000028644 ) ;
#6624 = CARTESIAN_POINT ( 'NONE',  ( -71.92837670882106238, -36.87473357531881391, -1.732050807568860318 ) ) ;
#6625 = CARTESIAN_POINT ( 'NONE',  ( 4.956406565555597332, -28.59095027454233673, 7.006423389747790331 ) ) ;
#6626 = DIRECTION ( 'NONE',  ( -0.1303762246624179666, -0.7394003126383923430, -0.6605219282605402364 ) ) ;
#6627 = B_SPLINE_CURVE_WITH_KNOTS ( 'NONE', 3,
 ( #21647, #11944, #36875, #11734, #2108, #18124, #30921, #5586, #30718, #30294, #31119, #5997, #15046, #24311 ),
 .UNSPECIFIED., .F., .F.,
 ( 4, 2, 2, 2, 2, 2, 4 ),
 ( 0.004708422389589472963, 0.005296932628068655100, 0.005591187747308264816, 0.005885442866547874533, 0.006179697985787484249, 0.006473953105027094833, 0.007062463343506314266 ),
 .UNSPECIFIED. ) ;
#6628 = ORIENTED_EDGE ( 'NONE', *, *, #1590, .T. ) ;
#6629 = FACE_BOUND ( 'NONE', #40683, .T. ) ;
#6630 = EDGE_CURVE ( 'NONE', #38785, #5538, #36078, .T. ) ;
#6631 = CARTESIAN_POINT ( 'NONE',  ( 3.800390874224334858, -32.36993114662322313, 6.971170733404102648 ) ) ;
#6632 = ORIENTED_EDGE ( 'NONE', *, *, #19877, .T. ) ;
#6633 = CARTESIAN_POINT ( 'NONE',  ( 80.02802368947523348, 66.35789156557524393, -1.168532795814369418 ) ) ;
#6634 = CARTESIAN_POINT ( 'NONE',  ( 79.25227124789796562, 65.35518565838746952, 2.996423812020188038 ) ) ;
#6635 = DIRECTION ( 'NONE',  ( -1.000000000000000000, 0.000000000000000000, 0.000000000000000000 ) ) ;
#6636 = VERTEX_POINT ( 'NONE', #19848 ) ;
#6637 = CARTESIAN_POINT ( 'NONE',  ( 77.48272095992952302, 61.71466691532025806, -3.776276000690703682 ) ) ;
#6639 = DIRECTION ( 'NONE',  ( -0.6427876096865430267, 0.7660444431189749048, -0.000000000000000000 ) ) ;
#6638 = CARTESIAN_POINT ( 'NONE',  ( 21.73378977745097629, 0.2086431185004669342, 9.125156574515591146 ) ) ;
#6640 = CARTESIAN_POINT ( 'NONE',  ( 17.53208774037409867, 9.003388688526223760, -2.875468385787739667 ) ) ;
#6641 = CARTESIAN_POINT ( 'NONE',  ( 81.19366756170077792, 63.21158026472416225, -3.307636073424136569 ) ) ;
#6642 = CARTESIAN_POINT ( 'NONE',  ( 76.15169681074907260, 61.58848496619823010, 3.887901781369003551 ) ) ;
#6643 = ORIENTED_EDGE ( 'NONE', *, *, #13623, .T. ) ;
#6644 = CARTESIAN_POINT ( 'NONE',  ( -2.652992490026568007, -32.06776532245774547, 7.635761828346577573 ) ) ;
#6645 = CARTESIAN_POINT ( 'NONE',  ( -58.96512565301119224, 28.81081997859032739, 6.496329578498431623 ) ) ;
#6646 = CARTESIAN_POINT ( 'NONE',  ( 82.43319509988612026, 63.84109541104528063, 1.838010297257003156 ) ) ;
#6648 = CARTESIAN_POINT ( 'NONE',  ( 2.945629123076408007, -32.84819949571223674, 7.255881584735162093 ) ) ;
#6647 = CARTESIAN_POINT ( 'NONE',  ( 3.977572546501454642, -32.22783162523180067, 7.695279973900954751 ) ) ;
#6649 = CARTESIAN_POINT ( 'NONE',  ( 30.56085893896448269, -1.894852608703655017, -5.974852047816421319 ) ) ;
#6650 = CARTESIAN_POINT ( 'NONE',  ( -1.362284770087026642, -31.26406815671434813, 6.870737987065013819 ) ) ;
#6651 = FACE_OUTER_BOUND ( 'NONE', #31287, .T. ) ;
#6652 = PLANE ( 'NONE',  #9688 ) ;
#6653 = ORIENTED_EDGE ( 'NONE', *, *, #13729, .F. ) ;
#6654 = CARTESIAN_POINT ( 'NONE',  ( -0.6146738250898187150, -32.06000629750705855, 6.882085323592685100 ) ) ;
#6655 = CARTESIAN_POINT ( 'NONE',  ( 76.65176712096844369, 59.82760137992013227, 3.005358148697153453 ) ) ;
#6656 = VECTOR ( 'NONE', #21075, 1000.000000000000000 ) ;
#6657 = CARTESIAN_POINT ( 'NONE',  ( 36.54096646249387703, -2.167736877196097645, -5.903366266952701835 ) ) ;
#6658 = CARTESIAN_POINT ( 'NONE',  ( 78.69038500580363404, 66.05859403932464602, 1.000000000000000000 ) ) ;
#6659 = CARTESIAN_POINT ( 'NONE',  ( -0.9807834779648342272, -31.66069757387703731, 7.754798119455333705 ) ) ;
#6660 = CARTESIAN_POINT ( 'NONE',  ( 14.62224959569264371, -5.050472350199410876, -2.488553708487371008 ) ) ;
#6661 = CARTESIAN_POINT ( 'NONE',  ( 1.551251297819356001, -25.49307895267003587, 6.700000000000000178 ) ) ;
#6662 = CARTESIAN_POINT ( 'NONE',  ( -76.88335714230863971, 9.426892421563488611, 9.554449558844057222 ) ) ;
#6663 = EDGE_CURVE ( 'NONE', #32500, #15332, #14351, .T. ) ;
#6664 = CARTESIAN_POINT ( 'NONE',  ( 21.88155215452677282, -13.30971194246768619, -2.500000000000000444 ) ) ;
#6665 = DIRECTION ( 'NONE',  ( 0.1736481776669273336, 0.9848077530122085754, -0.000000000000000000 ) ) ;
#6666 = EDGE_CURVE ( 'NONE', #2937, #18869, #36703, .T. ) ;
#6667 = CARTESIAN_POINT ( 'NONE',  ( 31.81893016007982666, -2.964826676376706160, 5.172511613851138890 ) ) ;
#6668 = ORIENTED_EDGE ( 'NONE', *, *, #3660, .T. ) ;
#6669 = CARTESIAN_POINT ( 'NONE',  ( 2.326171464738295835, -32.91184545387483951, 7.695279973900954751 ) ) ;
#6670 = CARTESIAN_POINT ( 'NONE',  ( 67.84886183593677345, 57.97047572268562021, -3.979762160777300828 ) ) ;
#6671 = AXIS2_PLACEMENT_3D ( 'NONE', #31559, #3382, #24763 ) ;
#6672 = ADVANCED_FACE ( 'NONE', ( #7285 ), #4460, .T. ) ;
#6673 = VERTEX_POINT ( 'NONE', #22951 ) ;
#6674 = CARTESIAN_POINT ( 'NONE',  ( -0.9708236080994220307, -27.31698449112596805, 7.773839561854632763 ) ) ;
#6675 = ADVANCED_FACE ( 'NONE', ( #32627 ), #35514, .F. ) ;
#6676 = DIRECTION ( 'NONE',  ( 0.8888117386314182689, 0.4582725098355732163, 0.000000000000000000 ) ) ;
#6677 = CARTESIAN_POINT ( 'NONE',  ( 23.28355779755547772, 3.054638135287742973, 3.997861808092709079 ) ) ;
#6678 = CARTESIAN_POINT ( 'NONE',  ( 3.595293925934929025, -26.62725462111816199, 6.895394898881670009 ) ) ;
#6679 = DIRECTION ( 'NONE',  ( 1.000000000000000000, 0.000000000000000000, 0.000000000000000000 ) ) ;
#6680 = ORIENTED_EDGE ( 'NONE', *, *, #39750, .F. ) ;
#6681 = DIRECTION ( 'NONE',  ( 0.7055275666422156089, 0.2567910337120342668, 0.6605219282605377940 ) ) ;
#6682 = CARTESIAN_POINT ( 'NONE',  ( 78.74533340381492508, 66.05753824468469304, 1.508787936435526111 ) ) ;
#6683 = VERTEX_POINT ( 'NONE', #22753 ) ;
#6684 = CIRCLE ( 'NONE', #21811, 10.00000000000000888 ) ;
#6685 = CARTESIAN_POINT ( 'NONE',  ( -24.87867591359218977, -26.64985754041175525, 6.700000000000000178 ) ) ;
#6686 = ORIENTED_EDGE ( 'NONE', *, *, #14897, .F. ) ;
#6687 = CARTESIAN_POINT ( 'NONE',  ( 79.49720564641141607, 63.45635150964716331, -3.756013696796376866 ) ) ;
#6688 = B_SPLINE_CURVE_WITH_KNOTS ( 'NONE', 3,
 ( #24113, #26614, #8460, #29692, #20417, #35891, #39556, #33420, #5190, #1505, #36480, #30513, #10944, #36677, #21044, #17722, #26418, #38946, #23524, #30306, #36280, #39352, #2118, #14636, #32998 ),
 .UNSPECIFIED., .F., .F.,
 ( 4, 3, 3, 3, 3, 3, 3, 3, 4 ),
 ( 6.468151674593654050E-05, 9.076621574722243315E-05, 0.0001210204262067992133, 0.0001512763324577413697, 0.0001815301820994213761, 0.0002117781465860721964, 0.0002420274594459754516, 0.0002722905548971139996, 0.0002816827545175585711 ),
 .UNSPECIFIED. ) ;
#6690 = DIRECTION ( 'NONE',  ( -0.000000000000000000, -1.000000000000000000, -0.000000000000000000 ) ) ;
#6689 = CARTESIAN_POINT ( 'NONE',  ( 23.08452066313556728, 0.3618351664096016718, 5.927938974875374356 ) ) ;
#6691 = CARTESIAN_POINT ( 'NONE',  ( 79.31479573854757348, 66.13045663638729366, -1.878604182848723214 ) ) ;
#6692 = CARTESIAN_POINT ( 'NONE',  ( 79.56639652130381535, 63.83553059081831549, 3.738478073092012632 ) ) ;
#6693 = ORIENTED_EDGE ( 'NONE', *, *, #9864, .T. ) ;
#6694 = CARTESIAN_POINT ( 'NONE',  ( 78.69038500580381879, 66.05859403932473128, 1.002944004955704349 ) ) ;
#6696 = ORIENTED_EDGE ( 'NONE', *, *, #31062, .T. ) ;
#6695 = CARTESIAN_POINT ( 'NONE',  ( -64.08758708074093136, 42.49042454705804772, 3.493279343125383019 ) ) ;
#6697 = CARTESIAN_POINT ( 'NONE',  ( 22.79820677575384380, -6.119817767430131283, -4.702819652331462486 ) ) ;
#6698 = CARTESIAN_POINT ( 'NONE',  ( -11.07867591359219794, -26.64985754041175525, 6.700000000000000178 ) ) ;
#6699 = CARTESIAN_POINT ( 'NONE',  ( -75.59643797491145278, 8.517404848297713826, 8.876789325663764885 ) ) ;
#6700 = CARTESIAN_POINT ( 'NONE',  ( 24.74478317148397366, 0.5639450319252965471, -4.778967461423221152 ) ) ;
#6701 = VERTEX_POINT ( 'NONE', #26241 ) ;
#6702 = CARTESIAN_POINT ( 'NONE',  ( -1.544283425328523141, -28.25784841267573810, 7.753200566781599079 ) ) ;
#6703 = ORIENTED_EDGE ( 'NONE', *, *, #30710, .F. ) ;
#6704 = CARTESIAN_POINT ( 'NONE',  ( 1.713233352393388031, -32.96991108853358554, 7.756377446753163873 ) ) ;
#6705 = CARTESIAN_POINT ( 'NONE',  ( 28.39194851430366029, -3.973459996416360163, -4.268407213906094455 ) ) ;
#6706 = CARTESIAN_POINT ( 'NONE',  ( 30.88299797002222746, 0.6986532466800533525, -4.492965408520093185 ) ) ;
#6707 = CARTESIAN_POINT ( 'NONE',  ( 3.788778725684116999, -32.25297732395376471, 6.863904403958576594 ) ) ;
#6708 = CARTESIAN_POINT ( 'NONE',  ( 16.69500445109213160, 9.542985874932153223, 2.812057233438115755 ) ) ;
#6709 = CARTESIAN_POINT ( 'NONE',  ( 78.69038500580363404, 66.05859403932464602, 4.000000000000000000 ) ) ;
#6710 = B_SPLINE_CURVE_WITH_KNOTS ( 'NONE', 3,
 ( #16033, #199, #16238, #25107, #31902, #28390 ),
 .UNSPECIFIED., .F., .F.,
 ( 4, 2, 4 ),
 ( 0.000000000000000000, 0.5000000000000001110, 1.000000000000000000 ),
 .UNSPECIFIED. ) ;
#6711 = CARTESIAN_POINT ( 'NONE',  ( 4.927610109650206738, -30.92457071343696384, 7.013842709614101167 ) ) ;
#6712 = CARTESIAN_POINT ( 'NONE',  ( -6.248748702180631831, -25.49307895267003587, 6.700000000000000178 ) ) ;
#6713 = DIRECTION ( 'NONE',  ( 1.000000000000000000, 0.000000000000000000, 0.000000000000000000 ) ) ;
#6714 = AXIS2_PLACEMENT_3D ( 'NONE', #38265, #38664, #32717 ) ;
#6715 = CARTESIAN_POINT ( 'NONE',  ( 33.24375687178804384, -0.2091650819081217472, -4.975944415730187309 ) ) ;
#6716 = DIRECTION ( 'NONE',  ( 1.000000000000000000, 0.000000000000000000, 0.000000000000000000 ) ) ;
#6717 = ORIENTED_EDGE ( 'NONE', *, *, #11321, .F. ) ;
#6718 = CARTESIAN_POINT ( 'NONE',  ( 66.72638704319571445, 57.85960203741856134, 3.999543855871245945 ) ) ;
#6719 = EDGE_CURVE ( 'NONE', #39731, #33142, #10570, .T. ) ;
#6720 = CARTESIAN_POINT ( 'NONE',  ( -4.224659823956008253, -51.67615071827237472, 6.000000000000000000 ) ) ;
#6721 = CARTESIAN_POINT ( 'NONE',  ( 88.27260010123318068, -2.240648412321151639, -1.886171102315310266 ) ) ;
#6722 = ADVANCED_FACE ( 'NONE', ( #4422 ), #33605, .T. ) ;
#6723 = CARTESIAN_POINT ( 'NONE',  ( -0.4645989045071012846, -32.20074343675116069, 7.257242401810563237 ) ) ;
#6724 = ORIENTED_EDGE ( 'NONE', *, *, #14679, .F. ) ;
#6725 = CARTESIAN_POINT ( 'NONE',  ( 24.53930908985638482, 2.973372590794613135, 3.607145940306804466 ) ) ;
#6726 = DIRECTION ( 'NONE',  ( 1.000000000000000000, 0.000000000000000000, 0.000000000000000000 ) ) ;
#6727 = DIRECTION ( 'NONE',  ( -0.000000000000000000, -0.000000000000000000, 1.000000000000000000 ) ) ;
#6728 = DIRECTION ( 'NONE',  ( 0.000000000000000000, 0.000000000000000000, -1.000000000000000000 ) ) ;
#6729 = EDGE_LOOP ( 'NONE', ( #31427, #607, #8420, #24274 ) ) ;
#6730 = ORIENTED_EDGE ( 'NONE', *, *, #6846, .F. ) ;
#6731 = CARTESIAN_POINT ( 'NONE',  ( 80.65652637675404435, 62.34602738889181950, -3.260928702718591587 ) ) ;
#6732 = CARTESIAN_POINT ( 'NONE',  ( -1.743143437565867870, -28.96217217187591686, 7.767720160662274331 ) ) ;
#6733 = CARTESIAN_POINT ( 'NONE',  ( 79.43051736299561583, 64.82585401503284572, 3.419027627190938556 ) ) ;
#6734 = B_SPLINE_CURVE_WITH_KNOTS ( 'NONE', 3,
 ( #39826, #24176, #36730, #28896, #6674, #28075, #294, #19426, #31382, #703, #31997, #22330, #3803, #34898, #6473, #22122, #12432, #28486, #505 ),
 .UNSPECIFIED., .F., .F.,
 ( 4, 3, 3, 3, 3, 3, 4 ),
 ( 0.000000000000000000, 2.546128104244838633E-05, 5.711050680484096683E-05, 8.113074941676158883E-05, 0.0001053129305727108458, 0.0001360598016347157812, 0.0001612931755702065552 ),
 .UNSPECIFIED. ) ;
#6736 = ORIENTED_EDGE ( 'NONE', *, *, #5456, .F. ) ;
#6735 = LINE ( 'NONE', #13506, #11803 ) ;
#6737 = CARTESIAN_POINT ( 'NONE',  ( -30.34874870218063947, -26.64985754041175525, 6.700000000000000178 ) ) ;
#6738 = CARTESIAN_POINT ( 'NONE',  ( 1.034849034344471397, -33.00608048689603891, 6.873189335546979528 ) ) ;
#6739 = CARTESIAN_POINT ( 'NONE',  ( -71.92837670882107659, -20.78299143688747819, 9.949874371066202983 ) ) ;
#6740 = CARTESIAN_POINT ( 'NONE',  ( 33.78539320900111420, -4.844129098076136231, -3.475568256863553529 ) ) ;
#6741 = CARTESIAN_POINT ( 'NONE',  ( 24.72484072709785252, 3.007097173862428363, -3.410376447172846159 ) ) ;
#6742 = CARTESIAN_POINT ( 'NONE',  ( -64.75098741874504071, 36.24760096809371390, -6.319851154868031173 ) ) ;
#6743 = CIRCLE ( 'NONE', #29736, 3.499999999999999556 ) ;
#6744 = ORIENTED_EDGE ( 'NONE', *, *, #34109, .F. ) ;
#6745 = CARTESIAN_POINT ( 'NONE',  ( -1.016762692402616741, -31.61373686903379365, 6.887945620086122211 ) ) ;
#6746 = DIRECTION ( 'NONE',  ( 1.000000000000000000, 9.912705577010326536E-16, 0.000000000000000000 ) ) ;
#6747 = CARTESIAN_POINT ( 'NONE',  ( -78.65221700006590311, -5.324689618735268581, -8.103210926880651144 ) ) ;
#6748 = CIRCLE ( 'NONE', #31730, 8.080217238368755162 ) ;
#6749 = CARTESIAN_POINT ( 'NONE',  ( 1.751251297819361730, -25.49307895267003587, 6.700000000000000178 ) ) ;
#6750 = FACE_OUTER_BOUND ( 'NONE', #36729, .T. ) ;
#6751 = CARTESIAN_POINT ( 'NONE',  ( 81.15131294690949915, 61.29729393613784083, 1.130345937366645126 ) ) ;
#6752 = PLANE ( 'NONE',  #38681 ) ;
#6753 = CARTESIAN_POINT ( 'NONE',  ( 25.06944232269932016, 3.214832799815183328, -2.439993125860743017 ) ) ;
#6754 = ORIENTED_EDGE ( 'NONE', *, *, #3069, .T. ) ;
#6755 = CARTESIAN_POINT ( 'NONE',  ( -0.8812738228061313128, -31.78239750451386669, 7.680992449362123331 ) ) ;
#6756 = FACE_OUTER_BOUND ( 'NONE', #38190, .T. ) ;
#6757 = ORIENTED_EDGE ( 'NONE', *, *, #36845, .T. ) ;
#6758 = DIRECTION ( 'NONE',  ( -0.000000000000000000, -0.000000000000000000, 1.000000000000000000 ) ) ;
#6759 = CARTESIAN_POINT ( 'NONE',  ( -59.93345510331042902, 24.73247967741478703, -9.800414904976365804 ) ) ;
#6760 = CARTESIAN_POINT ( 'NONE',  ( 4.642167673473801770, -27.86522685681402578, 7.763628509615289275 ) ) ;
#6761 = DIRECTION ( 'NONE',  ( 0.000000000000000000, 0.000000000000000000, 1.000000000000000000 ) ) ;
#6762 = CARTESIAN_POINT ( 'NONE',  ( 34.77305544684841010, -3.164287952476340315, 5.633574310641240146 ) ) ;
#6763 = CARTESIAN_POINT ( 'NONE',  ( 86.17935586795600500, 1.556981766839054426, 4.792924669753763744 ) ) ;
#6764 = EDGE_CURVE ( 'NONE', #8980, #12694, #1869, .T. ) ;
#6765 = ORIENTED_EDGE ( 'NONE', *, *, #30608, .T. ) ;
#6767 = CARTESIAN_POINT ( 'NONE',  ( 14.73380738849293792, -5.106256559584044119, 2.499999999999999556 ) ) ;
#6766 = CARTESIAN_POINT ( 'NONE',  ( 80.54433603269384889, 64.00140174820366212, -3.588566286536284178 ) ) ;
#6768 = CARTESIAN_POINT ( 'NONE',  ( -1.336977274318315922, -31.28272478379368238, 7.783750581861601070 ) ) ;
#6769 = CARTESIAN_POINT ( 'NONE',  ( 2.925322604187870379, -32.84858052415668794, 7.660770905198782010 ) ) ;
#6770 = AXIS2_PLACEMENT_3D ( 'NONE', #15362, #15975, #21760 ) ;
#6771 = LINE ( 'NONE', #5951, #38864 ) ;
#6772 = VERTEX_POINT ( 'NONE', #26635 ) ;
#6773 = CARTESIAN_POINT ( 'NONE',  ( -1.629351933014555165, -28.88225008802736582, 7.774064877406531515 ) ) ;
#6774 = VERTEX_POINT ( 'NONE', #2140 ) ;
#6775 = CARTESIAN_POINT ( 'NONE',  ( -74.92283640148291113, 18.87330372387140187, -9.800414904976365804 ) ) ;
#6776 = ORIENTED_EDGE ( 'NONE', *, *, #404, .F. ) ;
#6777 = CARTESIAN_POINT ( 'NONE',  ( 79.31717123896757471, 65.40625759565881481, -2.968223699503262480 ) ) ;
#6778 = CARTESIAN_POINT ( 'NONE',  ( -1.501411291908892665, -28.42602797326624398, 7.643333865083954848 ) ) ;
#6779 = CARTESIAN_POINT ( 'NONE',  ( 21.78575280733538122, 1.236091024911973202, 7.097413734593241763 ) ) ;
#6781 = VERTEX_POINT ( 'NONE', #26439 ) ;
#6780 = ORIENTED_EDGE ( 'NONE', *, *, #17592, .F. ) ;
#6782 = CARTESIAN_POINT ( 'NONE',  ( 81.92450911876609609, 64.33049094056623574, -2.665107514501070085 ) ) ;
#6783 = DIRECTION ( 'NONE',  ( 1.000000000000000000, 0.000000000000000000, 0.000000000000000000 ) ) ;
#6785 = CARTESIAN_POINT ( 'NONE',  ( 85.13283666514081460, 2.732481806238816535, 0.06822753118436197806 ) ) ;
#6784 = CARTESIAN_POINT ( 'NONE',  ( -57.66409387480749871, 30.21301454600294178, -4.063144412293765662 ) ) ;
#6786 = LINE ( 'NONE', #207, #20487 ) ;
#6787 = CARTESIAN_POINT ( 'NONE',  ( 0.8807958757747548217, -0.6000000000000004219, 3.993526596136941720 ) ) ;
#6788 = CARTESIAN_POINT ( 'NONE',  ( 71.16717283274410022, 58.92450812456241493, 3.908768822720079417 ) ) ;
#6789 = ADVANCED_FACE ( 'NONE', ( #39170 ), #27035, .F. ) ;
#6790 = VERTEX_POINT ( 'NONE', #8276 ) ;
#6791 = CARTESIAN_POINT ( 'NONE',  ( 22.21123912593981231, 3.886607422916119159, -4.083038617570321271 ) ) ;
#6792 = ORIENTED_EDGE ( 'NONE', *, *, #9558, .T. ) ;
#6793 = ORIENTED_EDGE ( 'NONE', *, *, #39351, .T. ) ;
#6794 = CARTESIAN_POINT ( 'NONE',  ( 21.85643539959772497, -11.05315871940826078, 3.104450560420165317 ) ) ;
#6795 = CARTESIAN_POINT ( 'NONE',  ( 21.86697325016263349, 4.291357277889674471, -2.119771864009106999 ) ) ;
#6796 = CARTESIAN_POINT ( 'NONE',  ( -54.93030506612853969, 31.40261711588176397, -1.217302950687081831 ) ) ;
#6797 = CARTESIAN_POINT ( 'NONE',  ( 81.57279438772143010, 63.75980975930807659, 3.125232205748817105 ) ) ;
#6798 = CARTESIAN_POINT ( 'NONE',  ( 86.38515361113813640, 1.239318396469950123, 5.566871328843018496 ) ) ;
#6799 = ORIENTED_EDGE ( 'NONE', *, *, #22707, .T. ) ;
#6800 = MECHANICAL_DESIGN_GEOMETRIC_PRESENTATION_REPRESENTATION (  '', ( #2880 ), #15985 ) ;
#6801 = CARTESIAN_POINT ( 'NONE',  ( 2.726104662367788034, -32.91626305826840593, 6.998987538705434552 ) ) ;
#6802 = VERTEX_POINT ( 'NONE', #20850 ) ;
#6803 = CARTESIAN_POINT ( 'NONE',  ( 17.10999649532181976, -3.067137622865070412, 2.876826778560678033 ) ) ;
#6804 = EDGE_CURVE ( 'NONE', #22388, #33136, #32823, .T. ) ;
#6805 = DIRECTION ( 'NONE',  ( -3.491481338843133750E-15, 1.000000000000000000, -0.000000000000000000 ) ) ;
#6806 = CARTESIAN_POINT ( 'NONE',  ( 20.42490770359840369, 3.667757226666287007, -3.394198844042774166 ) ) ;
#6807 = CARTESIAN_POINT ( 'NONE',  ( 4.938390203311415748E-15, -42.37473357531882101, -6.000000000000000000 ) ) ;
#6808 = CARTESIAN_POINT ( 'NONE',  ( 4.999814617694763541, -28.40211264311544070, 6.894806418505347700 ) ) ;
#6809 = CARTESIAN_POINT ( 'NONE',  ( -72.85689734034554021, 1.996344439234811086, 10.96066712856931602 ) ) ;
#6810 = DIRECTION ( 'NONE',  ( -1.000000000000000000, 0.000000000000000000, 0.000000000000000000 ) ) ;
#6811 = CARTESIAN_POINT ( 'NONE',  ( -1.234667376850867138, -31.28615792099245141, 7.748216051605120391 ) ) ;
#6812 = VECTOR ( 'NONE', #3640, 1000.000000000000000 ) ;
#6813 = DIRECTION ( 'NONE',  ( -0.000000000000000000, -0.000000000000000000, 1.000000000000000000 ) ) ;
#6814 = EDGE_CURVE ( 'NONE', #38692, #24999, #38965, .T. ) ;
#6815 = ORIENTED_EDGE ( 'NONE', *, *, #3855, .F. ) ;
#6816 = EDGE_CURVE ( 'NONE', #17865, #6217, #20641, .T. ) ;
#6817 = ORIENTED_EDGE ( 'NONE', *, *, #10084, .F. ) ;
#6818 = CARTESIAN_POINT ( 'NONE',  ( 33.68493938990636849, -3.838059396421490188, 5.140109112596683794 ) ) ;
#6819 = DIRECTION ( 'NONE',  ( 0.000000000000000000, 0.000000000000000000, 1.000000000000000000 ) ) ;
#6820 = CARTESIAN_POINT ( 'NONE',  ( 66.57962043698374544, 57.80678959376348303, -3.999745625240549440 ) ) ;
#6821 = ORIENTED_EDGE ( 'NONE', *, *, #19078, .F. ) ;
#6822 = DIRECTION ( 'NONE',  ( -0.000000000000000000, 1.000000000000000000, -0.000000000000000000 ) ) ;
#6823 = CARTESIAN_POINT ( 'NONE',  ( 4.961036936964867472, -28.60650807421071917, 6.959317978105165281 ) ) ;
#6824 = LINE ( 'NONE', #28223, #12976 ) ;
#6825 = ORIENTED_EDGE ( 'NONE', *, *, #38525, .T. ) ;
#6826 = FACE_BOUND ( 'NONE', #6412, .T. ) ;
#6827 = ORIENTED_EDGE ( 'NONE', *, *, #30174, .F. ) ;
#6828 = CARTESIAN_POINT ( 'NONE',  ( 79.33205627562968232, 66.30342423254379014, -1.132734665583632117 ) ) ;
#6829 = EDGE_CURVE ( 'NONE', #31687, #38060, #27230, .T. ) ;
#6830 = CARTESIAN_POINT ( 'NONE',  ( -80.90861860399088812, 11.45717611192839591, 0.6283086135788885640 ) ) ;
#6831 = ORIENTED_EDGE ( 'NONE', *, *, #336, .F. ) ;
#6832 = CARTESIAN_POINT ( 'NONE',  ( 74.58877118170933329, 61.99488014651142009, -3.786335567263263702 ) ) ;
#6834 = CARTESIAN_POINT ( 'NONE',  ( 0.5083189215984414977, 0.5999999999999995337, -3.960569937088434411 ) ) ;
#6833 = CARTESIAN_POINT ( 'NONE',  ( 2.496059417767232169, -26.16157129296014716, 6.945385021654666424 ) ) ;
#6835 = CARTESIAN_POINT ( 'NONE',  ( 20.81692704467059585, 6.281028057870155834, -3.335911822296410811 ) ) ;
#6836 = CARTESIAN_POINT ( 'NONE',  ( 80.26863108949493153, 64.98620546077044935, -3.307636073424134349 ) ) ;
#6837 = CARTESIAN_POINT ( 'NONE',  ( 75.74268929893182190, 62.45338499886813111, 3.784676997166864343 ) ) ;
#6838 = EDGE_LOOP ( 'NONE', ( #1041, #39712, #17076, #6323 ) ) ;
#6839 = VECTOR ( 'NONE', #4400, 1000.000000000000000 ) ;
#6840 = DIRECTION ( 'NONE',  ( -0.000000000000000000, -0.000000000000000000, 1.000000000000000000 ) ) ;
#6841 = CARTESIAN_POINT ( 'NONE',  ( -75.45330471031414277, 33.71485196875532608, 15.50000000000000000 ) ) ;
#6842 = CARTESIAN_POINT ( 'NONE',  ( 82.23158145857243539, 63.37565065107725104, 2.326649614737513527 ) ) ;
#6844 = CARTESIAN_POINT ( 'NONE',  ( 15.80745327116133936, 8.002139867661446360, 3.484773800359248774 ) ) ;
#6843 = CARTESIAN_POINT ( 'NONE',  ( -0.1398724371309366943, -32.54709977595698689, 6.863784140767622333 ) ) ;
#6845 = CARTESIAN_POINT ( 'NONE',  ( 29.34753533916922308, -2.431376398363487734, 5.582488461359439214 ) ) ;
#6846 = EDGE_CURVE ( 'NONE', #3701, #18601, #7692, .T. ) ;
#6847 = EDGE_CURVE ( 'NONE', #8362, #37942, #24141, .T. ) ;
#6848 = CYLINDRICAL_SURFACE ( 'NONE', #18800, 0.09010775117052789718 ) ;
#6849 = DIRECTION ( 'NONE',  ( 0.000000000000000000, -0.000000000000000000, -1.000000000000000000 ) ) ;
#6850 = EDGE_CURVE ( 'NONE', #8480, #28895, #20440, .T. ) ;
#6851 = AXIS2_PLACEMENT_3D ( 'NONE', #19276, #16183, #15784 ) ;
#6852 = CARTESIAN_POINT ( 'NONE',  ( 0.1277747208011560942, -26.43548358150071920, 7.387053503561885393 ) ) ;
#6853 = VERTEX_POINT ( 'NONE', #1732 ) ;
#6854 = CARTESIAN_POINT ( 'NONE',  ( 1.679286629257385588, -26.06999342767483796, 7.744938106820261403 ) ) ;
#6855 = DIRECTION ( 'NONE',  ( 1.000000000000000000, 0.000000000000000000, -0.000000000000000000 ) ) ;
#6856 = CARTESIAN_POINT ( 'NONE',  ( 33.44745999691134131, -3.711946420718001516, -5.220912322284510410 ) ) ;
#6857 = CARTESIAN_POINT ( 'NONE',  ( 36.92452998447934931, -2.367281692537941407, -5.951679316537522801 ) ) ;
#6858 = CARTESIAN_POINT ( 'NONE',  ( 4.761529427573594653, -31.28080595366133920, 7.255881584735163869 ) ) ;
#6859 = CARTESIAN_POINT ( 'NONE',  ( 1.713892699967802136, -33.06990413752668445, 7.635761828346576685 ) ) ;
#6860 =( BOUNDED_CURVE ( )  B_SPLINE_CURVE ( 3, ( #33856, #5844, #21283, #30768 ),
 .UNSPECIFIED., .F., .T. ) 
 B_SPLINE_CURVE_WITH_KNOTS ( ( 4, 4 ),
 ( 4.886921905584122428, 4.895802057644188743 ),
 .UNSPECIFIED. ) 
 CURVE ( )  GEOMETRIC_REPRESENTATION_ITEM ( )  RATIONAL_B_SPLINE_CURVE ( ( 1.000000000000000000, 0.9999934285857451366, 0.9999934285857451366, 1.000000000000000000 ) ) 
 REPRESENTATION_ITEM ( '' )  );
#6861 = CARTESIAN_POINT ( 'NONE',  ( 1.736346942945643512, -32.96974004645320377, 7.695279973900954751 ) ) ;
#6862 = CARTESIAN_POINT ( 'NONE',  ( -77.03546220438488490, 9.512508967889075961, 9.454972000433079060 ) ) ;
#6863 = CARTESIAN_POINT ( 'NONE',  ( 21.88182916724444382, -13.30283805793968277, -2.499999999999999112 ) ) ;
#6864 = CARTESIAN_POINT ( 'NONE',  ( 21.88116416870838066, -13.31970824832912825, 2.499999999999999112 ) ) ;
#6865 = CARTESIAN_POINT ( 'NONE',  ( 31.79659951825298947, -2.963653280094607823, 5.169026377125449656 ) ) ;
#6866 = ORIENTED_EDGE ( 'NONE', *, *, #36209, .F. ) ;
#6867 = EDGE_LOOP ( 'NONE', ( #10647, #31968 ) ) ;
#6868 = CARTESIAN_POINT ( 'NONE',  ( -12.99139449055068241, -10.90558813203967148, 6.000000000000000000 ) ) ;
#6869 = CARTESIAN_POINT ( 'NONE',  ( 68.74365607523500898, 58.25355655637604713, -3.970924506823472644 ) ) ;
#6870 = EDGE_LOOP ( 'NONE', ( #27558, #14894, #28426, #31324 ) ) ;
#6871 = CARTESIAN_POINT ( 'NONE',  ( -2.285626871745154887, -32.86765721485689795, 7.695279973900954751 ) ) ;
#6872 = CARTESIAN_POINT ( 'NONE',  ( -1.598337266838639970, -28.40014481679224545, 7.730015791551951843 ) ) ;
#6873 = CARTESIAN_POINT ( 'NONE',  ( 21.84694118651422201, 4.320250114505405747, 4.147421643609518149 ) ) ;
#6874 = CARTESIAN_POINT ( 'NONE',  ( 1.169535421114899387, -26.21162803541887598, 7.785172627573962778 ) ) ;
#6875 = CARTESIAN_POINT ( 'NONE',  ( 1.155917636822889838, -26.11252790201630347, 6.870737987065012931 ) ) ;
#6876 = ORIENTED_EDGE ( 'NONE', *, *, #10404, .F. ) ;
#6877 = CARTESIAN_POINT ( 'NONE',  ( 22.38249921582006507, 4.935340343470858926, 3.052593005165685991 ) ) ;
#6878 = CARTESIAN_POINT ( 'NONE',  ( 1.700390093233090871, -29.56993018339339940, 7.800000000000000711 ) ) ;
#6879 = AXIS2_PLACEMENT_3D ( 'NONE', #17255, #29828, #35234 ) ;
#6880 = EDGE_CURVE ( 'NONE', #5651, #25105, #35480, .T. ) ;
#6881 = CARTESIAN_POINT ( 'NONE',  ( 80.65352406091056991, 63.67746643299658160, 3.602832836245132953 ) ) ;
#6882 = CARTESIAN_POINT ( 'NONE',  ( -10.34874870218063769, -25.49307895267003587, 6.800000000000000711 ) ) ;
#6883 = ORIENTED_EDGE ( 'NONE', *, *, #28721, .F. ) ;
#6884 = CARTESIAN_POINT ( 'NONE',  ( 79.19917379928831735, 63.30335940139927686, -3.774260586041106258 ) ) ;
#6886 = CARTESIAN_POINT ( 'NONE',  ( -1.677690022156054450, -29.95540375996364446, 6.979335674598007522 ) ) ;
#6885 = CARTESIAN_POINT ( 'NONE',  ( 27.41509945826695471, 1.020312500805418132, 4.485089514595300919 ) ) ;
#6887 = CARTESIAN_POINT ( 'NONE',  ( 81.69418451912821411, 62.49370361018091558, -2.611089443229507534 ) ) ;
#6888 = CARTESIAN_POINT ( 'NONE',  ( 79.49720564641141607, 63.45635150964716331, 3.756013696796376422 ) ) ;
#6889 = ADVANCED_FACE ( 'NONE', ( #2349, #9107 ), #27440, .F. ) ;
#6890 = ADVANCED_FACE ( 'NONE', ( #11766 ), #24764, .F. ) ;
#6891 = CARTESIAN_POINT ( 'NONE',  ( 82.55792188592127445, 63.20960171500894376, 1.133121492189030244 ) ) ;
#6892 = CARTESIAN_POINT ( 'NONE',  ( -64.08758708074093136, 43.44410442252532079, 1.728127057092140317 ) ) ;
#6893 = FACE_OUTER_BOUND ( 'NONE', #6870, .T. ) ;
#6894 = ORIENTED_EDGE ( 'NONE', *, *, #12422, .F. ) ;
#6895 = CARTESIAN_POINT ( 'NONE',  ( -73.50257855008051422, -0.7799437568714130409, 9.721213065138739395 ) ) ;
#6896 = ORIENTED_EDGE ( 'NONE', *, *, #33451, .T. ) ;
#6897 = ADVANCED_FACE ( 'NONE', ( #28047 ), #21684, .F. ) ;
#6898 = LINE ( 'NONE', #16549, #8340 ) ;
#6899 = AXIS2_PLACEMENT_3D ( 'NONE', #14024, #25997, #36075 ) ;
#6900 = VECTOR ( 'NONE', #5934, 1000.000000000000114 ) ;
#6901 = CARTESIAN_POINT ( 'NONE',  ( -0.9786402413886234886, -31.81717058986465574, 7.767720160662274331 ) ) ;
#6902 = CARTESIAN_POINT ( 'NONE',  ( 32.00493796099151922, -3.634882110226827390, -4.956983323664922558 ) ) ;
#6903 = CARTESIAN_POINT ( 'NONE',  ( 33.94631716816222422, -0.4876237784438076095, -5.120956352787560562 ) ) ;
#6904 = DIRECTION ( 'NONE',  ( -1.000000000000000000, 0.000000000000000000, 0.000000000000000000 ) ) ;
#6905 = CARTESIAN_POINT ( 'NONE',  ( 16.86343556102044872, 9.686623936461598916, 2.782464905949770362 ) ) ;
#6906 = CARTESIAN_POINT ( 'NONE',  ( 5.197380002583291692, -29.71505624550104940, 6.875780273367528395 ) ) ;
#6907 = CARTESIAN_POINT ( 'NONE',  ( -0.5767923600352571345, -26.91202874155497682, 7.686927408461907696 ) ) ;
#6908 = CARTESIAN_POINT ( 'NONE',  ( 1.651251297819358754, -26.64985754041175525, 6.800000000000000711 ) ) ;
#6909 = VECTOR ( 'NONE', #18088, 1000.000000000000114 ) ;
#6910 = DIRECTION ( 'NONE',  ( 1.000000000000000000, -1.061555284671232059E-15, 0.000000000000000000 ) ) ;
#6911 = CARTESIAN_POINT ( 'NONE',  ( 29.63503081302897968, 1.162161518828512152, -4.256401061717856926 ) ) ;
#6912 = CARTESIAN_POINT ( 'NONE',  ( -27.07867591359219972, -26.64985754041175525, 6.700000000000000178 ) ) ;
#6913 = ORIENTED_EDGE ( 'NONE', *, *, #13069, .F. ) ;
#6914 = CARTESIAN_POINT ( 'NONE',  ( 66.88099813915303571, 57.89052526007606758, 3.999029912548879739 ) ) ;
#6915 = CARTESIAN_POINT ( 'NONE',  ( 2.280574181144366275, -26.11834879376533536, 7.733670252284491120 ) ) ;
#6916 = CARTESIAN_POINT ( 'NONE',  ( 88.80100535589549793, -2.068446212231642711, -0.8863989573356614304 ) ) ;
#6917 = ORIENTED_EDGE ( 'NONE', *, *, #24253, .T. ) ;
#6918 = CARTESIAN_POINT ( 'NONE',  ( 26.58413863979593827, 1.645201016816646877, 4.327475460437605115 ) ) ;
#6919 = CARTESIAN_POINT ( 'NONE',  ( -4.266520354791871306, -48.67644278316300444, 6.000000000000000000 ) ) ;
#6920 = CARTESIAN_POINT ( 'NONE',  ( 1.212983646527633130, -26.10426722441512837, 7.754798119455333705 ) ) ;
#6921 = ORIENTED_EDGE ( 'NONE', *, *, #39836, .F. ) ;
#6922 = CARTESIAN_POINT ( 'NONE',  ( 3.940724359950557698, -26.88089151923329112, 7.756742906098588186 ) ) ;
#6923 = AXIS2_PLACEMENT_3D ( 'NONE', #10483, #19761, #16650 ) ;
#6924 = B_SPLINE_CURVE_WITH_KNOTS ( 'NONE', 3,
 ( #11153, #39363, #23723, #32615, #4997, #35900, #4795, #4205, #4410, #36290 ),
 .UNSPECIFIED., .F., .F.,
 ( 4, 3, 3, 4 ),
 ( 0.0002170292169044816383, 0.0002420761345915974473, 0.0002723302478207005281, 0.0002816811360866845531 ),
 .UNSPECIFIED. ) ;
#6925 = VERTEX_POINT ( 'NONE', #34262 ) ;
#6926 = CARTESIAN_POINT ( 'NONE',  ( 78.96934220494343037, 65.43027598480369988, -2.854164747638217481 ) ) ;
#6927 = CIRCLE ( 'NONE', #17381, 0.1000000000000028644 ) ;
#6928 = CARTESIAN_POINT ( 'NONE',  ( -1.720424982935133906, -28.89024644203550807, 7.782861076432730840 ) ) ;
#6929 = CARTESIAN_POINT ( 'NONE',  ( 78.65528874306569662, 65.84149099381083658, 2.048264032867442630 ) ) ;
#6931 = ORIENTED_EDGE ( 'NONE', *, *, #33578, .F. ) ;
#6930 = LINE ( 'NONE', #11967, #25648 ) ;
#6932 = DIRECTION ( 'NONE',  ( 0.000000000000000000, 0.000000000000000000, 1.000000000000000000 ) ) ;
#6933 = CARTESIAN_POINT ( 'NONE',  ( -22.34874870218063947, -25.49307895267003587, 6.800000000000000711 ) ) ;
#6934 = CARTESIAN_POINT ( 'NONE',  ( 0.000000000000000000, 0.5999999999999995337, 4.250000000000000000 ) ) ;
#6935 = CARTESIAN_POINT ( 'NONE',  ( 21.85643539959775339, -7.728916438363212293, -14.50668795789714771 ) ) ;
#6936 = CARTESIAN_POINT ( 'NONE',  ( 24.74506495819852248, 3.013726380158780582, -3.376567986019525680 ) ) ;
#6937 = VERTEX_POINT ( 'NONE', #39996 ) ;
#6938 = DIRECTION ( 'NONE',  ( 0.000000000000000000, -1.000000000000000000, 0.000000000000000000 ) ) ;
#6939 = ADVANCED_FACE ( 'NONE', ( #40196 ), #6033, .F. ) ;
#6940 = EDGE_CURVE ( 'NONE', #2116, #9668, #28611, .T. ) ;
#6941 = DIRECTION ( 'NONE',  ( -0.000000000000000000, -0.000000000000000000, 1.000000000000000000 ) ) ;
#6942 = CARTESIAN_POINT ( 'NONE',  ( -18.27651686900387418, -64.04014080848075707, -2.500000000000000000 ) ) ;
#6943 = EDGE_CURVE ( 'NONE', #6524, #34445, #31974, .T. ) ;
#6944 = CARTESIAN_POINT ( 'NONE',  ( -73.25156588610681752, -0.1223437846077502639, -10.91517253786405028 ) ) ;
#6945 = CARTESIAN_POINT ( 'NONE',  ( -0.03056955003493260978, -26.64353671815714719, 7.691066658568943559 ) ) ;
#6946 = CARTESIAN_POINT ( 'NONE',  ( -7.078675913592194391, -26.64985754041175525, 6.800000000000000711 ) ) ;
#6947 = CARTESIAN_POINT ( 'NONE',  ( 80.80706632665069833, 63.75484916101672894, 3.549391953833845204 ) ) ;
#6948 = CARTESIAN_POINT ( 'NONE',  ( 84.14932678670007249, 2.958124188176427083, -1.306863746360770184 ) ) ;
#6949 = LINE ( 'NONE', #9623, #35849 ) ;
#6950 = CARTESIAN_POINT ( 'NONE',  ( -17.69482985384422236, -39.37473357531881391, 6.000000000000000000 ) ) ;
#6951 = CARTESIAN_POINT ( 'NONE',  ( 23.06591706423118637, -8.086835649431872497, -2.500000000000005773 ) ) ;
#6952 = CARTESIAN_POINT ( 'NONE',  ( 34.81584145744843539, -1.659602413401581211, 5.640252102379137433 ) ) ;
#6953 = ORIENTED_EDGE ( 'NONE', *, *, #35080, .F. ) ;
#6954 = CIRCLE ( 'NONE', #39834, 10.00000000000000888 ) ;
#6955 = VECTOR ( 'NONE', #7268, 1000.000000000000227 ) ;
#6956 = DIRECTION ( 'NONE',  ( 0.000000000000000000, -0.000000000000000000, -1.000000000000000000 ) ) ;
#6957 = CARTESIAN_POINT ( 'NONE',  ( 4.628654959960774917, -27.84213827743704428, 7.721096864323906850 ) ) ;
#6958 = LINE ( 'NONE', #594, #27331 ) ;
#6959 = CARTESIAN_POINT ( 'NONE',  ( 68.55047844998404116, 58.76352648041117277, 3.988324671431286106 ) ) ;
#6960 = CARTESIAN_POINT ( 'NONE',  ( 33.68706075914577269, -3.105129560293249380, 5.464078574745403927 ) ) ;
#6961 = AXIS2_PLACEMENT_3D ( 'NONE', #36372, #33300, #20926 ) ;
#6962 = PLANE ( 'NONE',  #37833 ) ;
#6963 = CARTESIAN_POINT ( 'NONE',  ( 86.81546468666313388, 0.8424741501213859340, -5.177899619954967392 ) ) ;
#6964 = EDGE_LOOP ( 'NONE', ( #26060, #5151, #18093, #13155 ) ) ;
#6966 = CARTESIAN_POINT ( 'NONE',  ( 1.749140210850987920, -26.17027969752984973, 6.894806418505346812 ) ) ;
#6965 = CARTESIAN_POINT ( 'NONE',  ( 79.30685661404397990, 65.70718262327383741, -2.676159939830900392 ) ) ;
#6967 =( BOUNDED_CURVE ( )  B_SPLINE_CURVE ( 3, ( #29552, #1370, #13903, #10795 ),
 .UNSPECIFIED., .F., .F. ) 
 B_SPLINE_CURVE_WITH_KNOTS ( ( 4, 4 ),
 ( 4.748221474220559735, 4.941946782021394036 ),
 .UNSPECIFIED. ) 
 CURVE ( )  GEOMETRIC_REPRESENTATION_ITEM ( )  RATIONAL_B_SPLINE_CURVE ( ( 1.000000000000000000, 0.9968749865767494445, 0.9968749865767494445, 1.000000000000000000 ) ) 
 REPRESENTATION_ITEM ( '' )  );
#6968 = CARTESIAN_POINT ( 'NONE',  ( -69.93649553638499583, -48.24651348640838222, 9.950929893704707041 ) ) ;
#6969 = CARTESIAN_POINT ( 'NONE',  ( -1.260458514972081501, -27.70352715432887436, 6.870724624169666228 ) ) ;
#6970 = ORIENTED_EDGE ( 'NONE', *, *, #10830, .T. ) ;
#6971 = DIRECTION ( 'NONE',  ( 0.000000000000000000, 0.000000000000000000, -1.000000000000000000 ) ) ;
#6972 = EDGE_LOOP ( 'NONE', ( #16882, #33945, #29542, #10257 ) ) ;
#6973 = CARTESIAN_POINT ( 'NONE',  ( -72.13633209003711499, 5.157242105139857813, 9.927673127863286595 ) ) ;
#6974 = ORIENTED_EDGE ( 'NONE', *, *, #40112, .T. ) ;
#6975 = CARTESIAN_POINT ( 'NONE',  ( 78.91303925368886496, 65.86465164089241853, -2.189516896894254216 ) ) ;
#6976 = CARTESIAN_POINT ( 'NONE',  ( -1.504497326213975361, -28.43472243647219599, 7.661510568013095934 ) ) ;
#6977 = CARTESIAN_POINT ( 'NONE',  ( 22.83085956305526310, 1.197354866361570513, 5.675763816237461512 ) ) ;
#6978 = ORIENTED_EDGE ( 'NONE', *, *, #24100, .F. ) ;
#6979 = AXIS2_PLACEMENT_3D ( 'NONE', #3035, #21539, #27694 ) ;
#6980 = AXIS2_PLACEMENT_3D ( 'NONE', #40127, #11907, #18297 ) ;
#6981 = CARTESIAN_POINT ( 'NONE',  ( -0.07675644365221842569, -32.46850745275099825, 7.778050822775631978 ) ) ;
#6983 = LINE ( 'NONE', #32513, #5885 ) ;
#6982 = CARTESIAN_POINT ( 'NONE',  ( 14.77222812468899349, 12.33286846116284252, -2.511961485181726239 ) ) ;
#6984 = LINE ( 'NONE', #23043, #28387 ) ;
#6985 = CARTESIAN_POINT ( 'NONE',  ( -64.08758708074093136, 44.09647858371768336, -0.9999999999999920064 ) ) ;
#6986 = CARTESIAN_POINT ( 'NONE',  ( 71.87019205445125181, 60.48965333507749165, 3.909340765870004564 ) ) ;
#6987 = CARTESIAN_POINT ( 'NONE',  ( 23.01932435154908418, 3.404353093427882726, -3.868829002755526325 ) ) ;
#6988 = ORIENTED_EDGE ( 'NONE', *, *, #591, .F. ) ;
#6989 = AXIS2_PLACEMENT_3D ( 'NONE', #6232, #34665, #6442 ) ;
#6990 = VERTEX_POINT ( 'NONE', #25378 ) ;
#6991 = CARTESIAN_POINT ( 'NONE',  ( 21.85643539959777470, 7.942361823516107755, 9.319573164223585948 ) ) ;
#6993 = EDGE_CURVE ( 'NONE', #23657, #18554, #20922, .T. ) ;
#6992 = CARTESIAN_POINT ( 'NONE',  ( 21.76122352783369251, 6.560793838969577685, -3.350653129111269113 ) ) ;
#6994 = EDGE_LOOP ( 'NONE', ( #4236, #17218, #13991, #10063, #12793, #1965, #39682, #1469, #20048 ) ) ;
#6995 = CARTESIAN_POINT ( 'NONE',  ( 0.3480583263237562175, -32.68941832084690446, 6.920489980334475710 ) ) ;
#6996 = CARTESIAN_POINT ( 'NONE',  ( 78.68499968550166557, 66.05476829360674174, 1.077711394955748192 ) ) ;
#6997 = CARTESIAN_POINT ( 'NONE',  ( 87.54376689718995408, -0.1385995495200708916, -5.388168202639758597 ) ) ;
#6998 = ORIENTED_EDGE ( 'NONE', *, *, #32982, .F. ) ;
#6999 = CARTESIAN_POINT ( 'NONE',  ( -6.878675913592188884, -26.64985754041175525, 6.700000000000000178 ) ) ;
#7000 = CARTESIAN_POINT ( 'NONE',  ( 33.11529288468890542, -3.093421031358547513, 5.374840369677361451 ) ) ;
#7001 = CARTESIAN_POINT ( 'NONE',  ( 5.078732654515307310, -29.18677349682085520, 6.939395833800441338 ) ) ;
#7002 = CARTESIAN_POINT ( 'NONE',  ( 35.86909678445674388, -2.086596214755629397, -5.804638069235120490 ) ) ;
#7003 = CARTESIAN_POINT ( 'NONE',  ( 6.149982165465896600, -31.13182306662183052, 7.695279973900954751 ) ) ;
#7004 = CARTESIAN_POINT ( 'NONE',  ( 85.57577930415899914, 1.015208198401525541, 5.782835925834406865 ) ) ;
#7005 = CARTESIAN_POINT ( 'NONE',  ( -75.55726679169593751, -3.620980792413103000, 10.26686770233818535 ) ) ;
#7006 = CARTESIAN_POINT ( 'NONE',  ( 1.448106776224391101, -26.17217962422370192, 7.505001789837627335 ) ) ;
#7007 = CARTESIAN_POINT ( 'NONE',  ( -1.287952588635929096, -31.19159846504654610, 7.778050822775631978 ) ) ;
#7008 = CARTESIAN_POINT ( 'NONE',  ( 35.94200923520244828, 151.3264224549853907, 4.000000000000000000 ) ) ;
#7009 = ORIENTED_EDGE ( 'NONE', *, *, #17233, .T. ) ;
#7010 = ORIENTED_EDGE ( 'NONE', *, *, #9148, .T. ) ;
#7011 = CARTESIAN_POINT ( 'NONE',  ( 36.44367144241243039, -1.735187743863684684, 5.732522741015722012 ) ) ;
#7012 = CARTESIAN_POINT ( 'NONE',  ( 1.682289128304578885, -33.06116167229027525, 7.778495531946297170 ) ) ;
#7013 = CIRCLE ( 'NONE', #10295, 0.1000000000000028644 ) ;
#7014 = EDGE_CURVE ( 'NONE', #11999, #22200, #6010, .T. ) ;
#7015 = CARTESIAN_POINT ( 'NONE',  ( 66.42396409678360669, 57.78537248076360555, -4.000000000000015099 ) ) ;
#7016 = AXIS2_PLACEMENT_3D ( 'NONE', #1389, #13311, #13732 ) ;
#7017 = VERTEX_POINT ( 'NONE', #29619 ) ;
#7018 = CYLINDRICAL_SURFACE ( 'NONE', #20031, 10.00000000000000533 ) ;
#7019 = CARTESIAN_POINT ( 'NONE',  ( -0.8688903936063803179, -27.19321022093548734, 7.013842709614101167 ) ) ;
#7020 = FACE_BOUND ( 'NONE', #8160, .T. ) ;
#7021 = FACE_OUTER_BOUND ( 'NONE', #11884, .T. ) ;
#7022 = ORIENTED_EDGE ( 'NONE', *, *, #28607, .T. ) ;
#7023 = CARTESIAN_POINT ( 'NONE',  ( 82.31416527841534503, 64.14174473599668147, -2.134985007310159943 ) ) ;
#7024 = ADVANCED_FACE ( 'NONE', ( #16303 ), #14405, .F. ) ;
#7025 = CARTESIAN_POINT ( 'NONE',  ( 2.845604633296745067, -26.36860488639111111, 7.748216051605122168 ) ) ;
#7026 = ORIENTED_EDGE ( 'NONE', *, *, #28164, .T. ) ;
#7027 = VERTEX_POINT ( 'NONE', #37209 ) ;
#7028 = CARTESIAN_POINT ( 'NONE',  ( 75.35164290873603932, 61.82650661013094862, -3.882889210543306824 ) ) ;
#7030 = LINE ( 'NONE', #13404, #19640 ) ;
#7029 = DIRECTION ( 'NONE',  ( 0.000000000000000000, 0.000000000000000000, 1.000000000000000000 ) ) ;
#7031 = CARTESIAN_POINT ( 'NONE',  ( -70.05520034786580652, -0.2785546670064985575, 5.936342406970505969 ) ) ;
#7032 = CARTESIAN_POINT ( 'NONE',  ( 76.61572510735739172, 60.58450557137933146, 3.562065002338831832 ) ) ;
#7033 = FACE_OUTER_BOUND ( 'NONE', #26275, .T. ) ;
#7034 = AXIS2_PLACEMENT_3D ( 'NONE', #38826, #38224, #583 ) ;
#7035 = PLANE ( 'NONE',  #33988 ) ;
#7037 = EDGE_CURVE ( 'NONE', #6285, #34388, #34024, .T. ) ;
#7036 = DIRECTION ( 'NONE',  ( -0.000000000000000000, -0.000000000000000000, 1.000000000000000000 ) ) ;
#7038 = CARTESIAN_POINT ( 'NONE',  ( 82.09393942629682783, 63.66644892668136890, 2.541832380858824347 ) ) ;
#7039 = CARTESIAN_POINT ( 'NONE',  ( -0.2130646727215941838, -32.50057703731113889, 6.941203072598479906 ) ) ;
#7040 = CARTESIAN_POINT ( 'NONE',  ( 31.90185279284946773, -4.312872639525808793, -3.838359570106229413 ) ) ;
#7041 = CARTESIAN_POINT ( 'NONE',  ( 2.261927316241842956, -26.21662072906820384, 7.730758795053807475 ) ) ;
#7042 = VECTOR ( 'NONE', #36961, 1000.000000000000000 ) ;
#7043 = CARTESIAN_POINT ( 'NONE',  ( 21.85643539959777115, -11.26372485911396737, 0.7475790860009233763 ) ) ;
#7044 = VECTOR ( 'NONE', #22113, 1000.000000000000000 ) ;
#7045 = CARTESIAN_POINT ( 'NONE',  ( 4.714834770645700779, -31.33122182330293981, 7.778495531946298058 ) ) ;
#7046 = CARTESIAN_POINT ( 'NONE',  ( 5.551251297819359110, -26.64985754041175525, 6.700000000000000178 ) ) ;
#7047 = CARTESIAN_POINT ( 'NONE',  ( 2.713312946249484714, -24.92052936065920932, 6.894806418505347700 ) ) ;
#7048 = CARTESIAN_POINT ( 'NONE',  ( 36.82690608461941650, -3.168782876732829656, -5.951696020828944889 ) ) ;
#7049 = CARTESIAN_POINT ( 'NONE',  ( -1.699609906766908818, -29.56993018339339940, 7.800000000000000711 ) ) ;
#7050 = CARTESIAN_POINT ( 'NONE',  ( 14.77222812468949442, 12.59898556833855032, -2.511961485181804843 ) ) ;
#7051 = CARTESIAN_POINT ( 'NONE',  ( 3.347837293313452367, -32.54413893917154610, 7.785172627573962778 ) ) ;
#7052 = CARTESIAN_POINT ( 'NONE',  ( 2.188233707926874327, -32.93476592962348803, 6.864651958020304257 ) ) ;
#7053 = B_SPLINE_CURVE_WITH_KNOTS ( 'NONE', 3,
 ( #28466, #9519, #34468, #274, #12813, #25386, #83, #6243, #18789, #31366, #3189, #15705, #37926, #9731, #34879, #6654, #487, #19204, #13021, #686, #1094, #1294, #10333, #10527, #886, #10722, #25993, #32979, #32786, #39132, #35674 ),
 .UNSPECIFIED., .F., .F.,
 ( 4, 3, 3, 3, 3, 3, 3, 3, 3, 3, 4 ),
 ( 0.000000000000000000, 2.999644130997804130E-05, 6.002588995695083457E-05, 8.960886084588256043E-05, 0.0001190604700446506651, 0.0001489538463052726962, 0.0001796139255493990204, 0.0002109707048517074038, 0.0002426195318110327544, 0.0002740640997889978898, 0.0002849778069099865880 ),
 .UNSPECIFIED. ) ;
#7054 = CARTESIAN_POINT ( 'NONE',  ( -12.99139449055068241, -10.90558813203967148, 6.000000000000000000 ) ) ;
#7055 = EDGE_CURVE ( 'NONE', #21186, #1813, #24243, .T. ) ;
#7056 = CARTESIAN_POINT ( 'NONE',  ( 22.03291717603176636, -11.53685166237917947, 2.500000000000000000 ) ) ;
#7057 = ORIENTED_EDGE ( 'NONE', *, *, #30, .F. ) ;
#7058 = LINE ( 'NONE', #32397, #28422 ) ;
#7059 = CARTESIAN_POINT ( 'NONE',  ( 68.01940210501214779, 58.40717514567135282, -3.996230182412886744 ) ) ;
#7060 = CARTESIAN_POINT ( 'NONE',  ( 5.101232590239002995, -29.77532064849933846, 7.386948897581448570 ) ) ;
#7061 = CIRCLE ( 'NONE', #11648, 5.681288188914806803 ) ;
#7062 = ORIENTED_EDGE ( 'NONE', *, *, #31451, .F. ) ;
#7063 = CARTESIAN_POINT ( 'NONE',  ( 30.57637419526079725, -3.206146428843060114, 4.965636198024955483 ) ) ;
#7064 = CARTESIAN_POINT ( 'NONE',  ( 22.19267663920264511, 4.186142737966082272, 3.887493867850188689 ) ) ;
#7065 = CARTESIAN_POINT ( 'NONE',  ( 2.304086713256504382, -32.91590543598751850, 7.635761828346577573 ) ) ;
#7066 = EDGE_CURVE ( 'NONE', #40076, #29262, #18611, .T. ) ;
#7067 = VERTEX_POINT ( 'NONE', #13391 ) ;
#7068 = EDGE_CURVE ( 'NONE', #24796, #34269, #1230, .T. ) ;
#7069 = DIRECTION ( 'NONE',  ( 0.000000000000000000, 0.000000000000000000, 1.000000000000000000 ) ) ;
#7070 = CIRCLE ( 'NONE', #12321, 6.000000000000002665 ) ;
#7071 = CARTESIAN_POINT ( 'NONE',  ( 1.196425252463139355, -26.10638800769887169, 6.863784140767622333 ) ) ;
#7072 = ORIENTED_EDGE ( 'NONE', *, *, #14605, .T. ) ;
#7073 = EDGE_CURVE ( 'NONE', #24284, #826, #6485, .T. ) ;
#7074 = LINE ( 'NONE', #4599, #28049 ) ;
#7075 = CARTESIAN_POINT ( 'NONE',  ( 80.61377670644297666, 63.65766204751285784, 3.614389211669659208 ) ) ;
#7076 = CARTESIAN_POINT ( 'NONE',  ( -15.07867591359219439, -26.64985754041175525, 6.700000000000000178 ) ) ;
#7077 = ORIENTED_EDGE ( 'NONE', *, *, #2738, .T. ) ;
#7078 = CARTESIAN_POINT ( 'NONE',  ( 78.95339491453125902, 64.13176242216603384, -3.627744115730409558 ) ) ;
#7080 = CARTESIAN_POINT ( 'NONE',  ( -1.740641890886630128, -28.93016385758256348, 6.893199460713416826 ) ) ;
#7079 = CARTESIAN_POINT ( 'NONE',  ( 26.03581818370150103, 0.8240965440397407527, 4.423294059681629697 ) ) ;
#7081 = CARTESIAN_POINT ( 'NONE',  ( 80.63952753655819095, 65.18836132073317913, -3.079343812547462367 ) ) ;
#7082 = CARTESIAN_POINT ( 'NONE',  ( 80.05518365985739138, 61.93129665380740079, 3.228498513792977143 ) ) ;
#7083 = VERTEX_POINT ( 'NONE', #36807 ) ;
#7084 = DIRECTION ( 'NONE',  ( -1.000000000000000000, 0.000000000000000000, 0.000000000000000000 ) ) ;
#7085 = ADVANCED_FACE ( 'NONE', ( #33735, #14556 ), #27541, .F. ) ;
#7086 = CARTESIAN_POINT ( 'NONE',  ( 81.35706873939174955, 65.93413826765582542, 1.145133701562419226 ) ) ;
#7087 =( BOUNDED_CURVE ( )  B_SPLINE_CURVE ( 3, ( #26078, #363, #12900, #16781 ),
 .UNSPECIFIED., .F., .T. ) 
 B_SPLINE_CURVE_WITH_KNOTS ( ( 4, 4 ),
 ( 4.748221474220560623, 4.886921905584129533 ),
 .UNSPECIFIED. ) 
 CURVE ( )  GEOMETRIC_REPRESENTATION_ITEM ( )  RATIONAL_B_SPLINE_CURVE ( ( 1.000000000000000000, 0.9983974916150919476, 0.9983974916150919476, 1.000000000000000000 ) ) 
 REPRESENTATION_ITEM ( '' )  );
#7089 = ORIENTED_EDGE ( 'NONE', *, *, #34804, .T. ) ;
#7088 = CARTESIAN_POINT ( 'NONE',  ( -64.08758708074093136, 43.61223003624221661, 1.151950131395627519 ) ) ;
#7090 = CARTESIAN_POINT ( 'NONE',  ( 24.83717141299267794, -2.182840666565796006, 6.391756413845674167 ) ) ;
#7091 = CARTESIAN_POINT ( 'NONE',  ( -64.47965924086389577, 36.51034344918424068, -5.743161323597451684 ) ) ;
#7092 = ORIENTED_EDGE ( 'NONE', *, *, #25900, .T. ) ;
#7093 = CARTESIAN_POINT ( 'NONE',  ( -80.16996465541035377, -5.617423336303677850, 6.125224573262133099 ) ) ;
#7094 = CARTESIAN_POINT ( 'NONE',  ( 26.06744311131525649, 0.7515804080732310100, -4.421654772982752668 ) ) ;
#7095 = CARTESIAN_POINT ( 'NONE',  ( -70.92837670882107659, 13.87661300689599742, -10.00000000000000533 ) ) ;
#7096 = ORIENTED_EDGE ( 'NONE', *, *, #22935, .T. ) ;
#7097 = VECTOR ( 'NONE', #25278, 1000.000000000000000 ) ;
#7098 = CARTESIAN_POINT ( 'NONE',  ( -1.048025675227300058, -31.73281868467400102, 7.766640943994351787 ) ) ;
#7099 = CARTESIAN_POINT ( 'NONE',  ( 34.79206662659809979, -3.832422124991777146, -5.379499388740839549 ) ) ;
#7100 = CARTESIAN_POINT ( 'NONE',  ( 30.31649042712836817, -3.037113472960369265, -4.938316272775912452 ) ) ;
#7101 = CARTESIAN_POINT ( 'NONE',  ( 3.836079016935684205, -32.21547265350353229, 6.880147297696981745 ) ) ;
#7102 = CARTESIAN_POINT ( 'NONE',  ( 15.70676156960853298, 10.60592294505261357, 2.657818031038195805 ) ) ;
#7103 = CARTESIAN_POINT ( 'NONE',  ( 5.196202670487992670, -29.74109799422956968, 7.011627023500181188 ) ) ;
#7104 = DIRECTION ( 'NONE',  ( -0.000000000000000000, -0.000000000000000000, -1.000000000000000000 ) ) ;
#7105 = PLANE ( 'NONE',  #29589 ) ;
#7106 = VECTOR ( 'NONE', #19544, 1000.000000000000000 ) ;
#7107 = EDGE_CURVE ( 'NONE', #33743, #33448, #8631, .T. ) ;
#7108 = CARTESIAN_POINT ( 'NONE',  ( -21.07867591359219617, -26.64985754041175525, 6.700000000000000178 ) ) ;
#7109 = CARTESIAN_POINT ( 'NONE',  ( 23.18429543757034139, 0.8410905956396856897, -5.610387443514746053 ) ) ;
#7110 = CARTESIAN_POINT ( 'NONE',  ( 33.93434842054367095, -0.4888659768199489219, -5.123735918607922990 ) ) ;
#7111 = CARTESIAN_POINT ( 'NONE',  ( -70.92837670882107659, 28.72470171467712063, 6.000000000000005329 ) ) ;
#7112 = ORIENTED_EDGE ( 'NONE', *, *, #40454, .F. ) ;
#7113 = CARTESIAN_POINT ( 'NONE',  ( 66.84561829912908593, 57.98873651192412382, 3.999241724016629362 ) ) ;
#7114 = EDGE_CURVE ( 'NONE', #40564, #3554, #30586, .T. ) ;
#7116 = EDGE_CURVE ( 'NONE', #6990, #34705, #20268, .T. ) ;
#7115 = CARTESIAN_POINT ( 'NONE',  ( 86.69422455818764206, -0.1941184515037400471, -5.886102099071623073 ) ) ;
#7117 = CARTESIAN_POINT ( 'NONE',  ( -1.142130670890778799, -27.69163557441362755, 7.386948897581450346 ) ) ;
#7118 = ORIENTED_EDGE ( 'NONE', *, *, #18334, .T. ) ;
#7119 = CARTESIAN_POINT ( 'NONE',  ( -81.78216522710987135, 10.46482146603914209, -1.037938286043770253 ) ) ;
#7120 = CARTESIAN_POINT ( 'NONE',  ( 0.000000000000000000, 0.000000000000000000, 0.000000000000000000 ) ) ;
#7121 = CARTESIAN_POINT ( 'NONE',  ( -73.79226524390077202, -1.360417495813321054, 12.50000000000000000 ) ) ;
#7122 = ADVANCED_FACE ( 'NONE', ( #1839 ), #34780, .T. ) ;
#7123 = LINE ( 'NONE', #35350, #39777 ) ;
#7124 = ORIENTED_EDGE ( 'NONE', *, *, #14327, .F. ) ;
#7125 = CARTESIAN_POINT ( 'NONE',  ( 3.936759689487521641, -26.87759828911498516, 7.750000000000000888 ) ) ;
#7126 = ORIENTED_EDGE ( 'NONE', *, *, #39294, .T. ) ;
#7127 = CARTESIAN_POINT ( 'NONE',  ( 80.89410497084979568, 61.37834026963087553, -2.095806625474240903 ) ) ;
#7128 = EDGE_CURVE ( 'NONE', #20627, #30874, #39475, .T. ) ;
#7129 = CARTESIAN_POINT ( 'NONE',  ( 79.30508931962911845, 64.72973333162836695, 3.449595662144110175 ) ) ;
#7131 = EDGE_LOOP ( 'NONE', ( #10989, #37339, #19930, #34547 ) ) ;
#7130 = CARTESIAN_POINT ( 'NONE',  ( -1.284931719067040623, -31.19715287159715444, 6.870716933885665512 ) ) ;
#7132 = VECTOR ( 'NONE', #4859, 1000.000000000000000 ) ;
#7133 = CARTESIAN_POINT ( 'NONE',  ( 24.24184507690288015, 2.646254481897600819, 3.989924234126151159 ) ) ;
#7134 = EDGE_CURVE ( 'NONE', #15332, #15750, #25552, .T. ) ;
#7135 = CARTESIAN_POINT ( 'NONE',  ( 27.52856511457626709, -4.375065239674293949, 3.731061453272236150 ) ) ;
#7136 = FACE_OUTER_BOUND ( 'NONE', #27715, .T. ) ;
#7137 = CARTESIAN_POINT ( 'NONE',  ( 21.85643539959774273, -11.65679437655345474, 11.20963770477306554 ) ) ;
#7138 = CARTESIAN_POINT ( 'NONE',  ( 23.14098296504576524, 4.020346899343795855, -3.126915550736968363 ) ) ;
#7139 = ORIENTED_EDGE ( 'NONE', *, *, #23382, .F. ) ;
#7140 = CARTESIAN_POINT ( 'NONE',  ( 11.65737507970504439, -23.60493063168009442, 6.800000000000000711 ) ) ;
#7141 = CARTESIAN_POINT ( 'NONE',  ( -0.9952687000786839544, -31.64198801802082528, 6.868387053540522480 ) ) ;
#7142 = CARTESIAN_POINT ( 'NONE',  ( -2.271193562574106650, -32.88485816291451869, 7.635761828346577573 ) ) ;
#7143 = CARTESIAN_POINT ( 'NONE',  ( -71.75682404118637692, 2.644744199176562560, -9.965669106298006952 ) ) ;
#7144 = AXIS2_PLACEMENT_3D ( 'NONE', #15089, #33650, #20863 ) ;
#7145 = CARTESIAN_POINT ( 'NONE',  ( 4.722721840544713778, -27.80484921947353527, 7.750000000000000888 ) ) ;
#7146 = CARTESIAN_POINT ( 'NONE',  ( -26.24874870218063450, -26.64985754041175525, 6.800000000000000711 ) ) ;
#7147 = CARTESIAN_POINT ( 'NONE',  ( 78.92617879813646198, 66.06909554768881776, 1.766895996212466402 ) ) ;
#7148 = CARTESIAN_POINT ( 'NONE',  ( 86.43572624768424362, -0.5192074800720991590, -5.777013305174518720 ) ) ;
#7149 = DIRECTION ( 'NONE',  ( -0.4582725098355735494, 0.8888117386314181578, 0.000000000000000000 ) ) ;
#7150 = CARTESIAN_POINT ( 'NONE',  ( 2.921884697477863835, -32.84986306847065407, 7.737115613922532553 ) ) ;
#7151 = CYLINDRICAL_SURFACE ( 'NONE', #18633, 0.09010775117053204664 ) ;
#7152 = ORIENTED_EDGE ( 'NONE', *, *, #7837, .T. ) ;
#7153 = EDGE_CURVE ( 'NONE', #12332, #4935, #19095, .T. ) ;
#7154 = CARTESIAN_POINT ( 'NONE',  ( -64.85784325972053921, 34.81586596186931359, 6.466735817496049421 ) ) ;
#7155 = CARTESIAN_POINT ( 'NONE',  ( -0.3564456010502966565, -26.86262611937285172, 6.876076431790004939 ) ) ;
#7156 = DIRECTION ( 'NONE',  ( -0.000000000000000000, -0.000000000000000000, -1.000000000000000000 ) ) ;
#7157 = ORIENTED_EDGE ( 'NONE', *, *, #36678, .F. ) ;
#7158 = CARTESIAN_POINT ( 'NONE',  ( 69.01369661159887414, 59.28919897632942337, 3.943722715026729109 ) ) ;
#7159 = CARTESIAN_POINT ( 'NONE',  ( 36.91107007784989236, -2.639074378160587209, 5.967263201888431290 ) ) ;
#7160 = ADVANCED_FACE ( 'NONE', ( #3284 ), #12855, .F. ) ;
#7161 = CARTESIAN_POINT ( 'NONE',  ( -64.08758708074093136, 42.61892514642057961, -2.587732764668352115 ) ) ;
#7163 = ADVANCED_FACE ( 'NONE', ( #21535 ), #15338, .F. ) ;
#7162 = CARTESIAN_POINT ( 'NONE',  ( 85.88453125851971492, 1.888142761377891832, -4.329341218647970280 ) ) ;
#7164 = ORIENTED_EDGE ( 'NONE', *, *, #30019, .T. ) ;
#7166 = DIRECTION ( 'NONE',  ( 0.9396926207859082059, 0.3420201433256695456, -0.000000000000000000 ) ) ;
#7165 = CARTESIAN_POINT ( 'NONE',  ( 79.14790672806260829, 65.85151465993942566, -2.407735119910378696 ) ) ;
#7167 = CARTESIAN_POINT ( 'NONE',  ( -1.235538214096436826, -27.66458519074676303, 6.912143950357346966 ) ) ;
#7168 = ORIENTED_EDGE ( 'NONE', *, *, #5758, .F. ) ;
#7169 = ADVANCED_FACE ( 'NONE', ( #12248 ), #16380, .T. ) ;
#7170 = VERTEX_POINT ( 'NONE', #28309 ) ;
#7171 = CARTESIAN_POINT ( 'NONE',  ( -77.60377033239008426, -6.254646173284871935, 7.448572753700554827 ) ) ;
#7172 = ADVANCED_FACE ( 'NONE', ( #12658 ), #22152, .F. ) ;
#7173 = ORIENTED_EDGE ( 'NONE', *, *, #8684, .F. ) ;
#7174 = AXIS2_PLACEMENT_3D ( 'NONE', #10856, #13958, #36193 ) ;
#7175 = ORIENTED_EDGE ( 'NONE', *, *, #13158, .F. ) ;
#7176 = CARTESIAN_POINT ( 'NONE',  ( 78.85680892556273136, 65.81502797165197194, -2.238287240292680558 ) ) ;
#7177 = DIRECTION ( 'NONE',  ( -0.000000000000000000, -1.000000000000000000, -0.000000000000000000 ) ) ;
#7178 = CARTESIAN_POINT ( 'NONE',  ( 25.03740577281743285, 1.729533793843111678, 4.338254701037809191 ) ) ;
#7179 = ORIENTED_EDGE ( 'NONE', *, *, #21238, .F. ) ;
#7180 = CARTESIAN_POINT ( 'NONE',  ( 5.026745426458600896, -30.27374936809274786, 6.864236717600932458 ) ) ;
#7182 = DIRECTION ( 'NONE',  ( -0.000000000000000000, -0.000000000000000000, 1.000000000000000000 ) ) ;
#7181 = CARTESIAN_POINT ( 'NONE',  ( 4.618939889237452689, -31.31408416873490097, 6.892063359921934307 ) ) ;
#7183 = CARTESIAN_POINT ( 'NONE',  ( -70.92837670882107659, -56.35932253828836025, 7.538952224936807056 ) ) ;
#7184 = CARTESIAN_POINT ( 'NONE',  ( 72.38109545502503295, 59.26788356430734694, 3.856543183738433189 ) ) ;
#7185 = CARTESIAN_POINT ( 'NONE',  ( 23.67583169985504910, 3.109125002522015624, -3.791247457039441660 ) ) ;
#7186 = VERTEX_POINT ( 'NONE', #37564 ) ;
#7187 = CARTESIAN_POINT ( 'NONE',  ( -6.978675913592191193, -24.55319635012989110, 6.700000000000000178 ) ) ;
#7188 = ORIENTED_EDGE ( 'NONE', *, *, #11233, .T. ) ;
#7189 = VECTOR ( 'NONE', #31982, 1000.000000000000114 ) ;
#7190 = CARTESIAN_POINT ( 'NONE',  ( 21.85643539959776760, 6.468309080218945795, -8.875946301973074881 ) ) ;
#7191 = CARTESIAN_POINT ( 'NONE',  ( 21.89426278105499435, 4.196054223286251883, 2.573115994139398661E-12 ) ) ;
#7192 = ORIENTED_EDGE ( 'NONE', *, *, #21960, .F. ) ;
#7193 = FACE_OUTER_BOUND ( 'NONE', #17869, .T. ) ;
#7194 = CARTESIAN_POINT ( 'NONE',  ( 81.44856608406136900, 64.08396523683258295, 3.179853676208926672 ) ) ;
#7195 = CARTESIAN_POINT ( 'NONE',  ( 88.02721697999687933, -0.6980542412123691420, -4.669518943469966210 ) ) ;
#7196 = CARTESIAN_POINT ( 'NONE',  ( -1.790841395663789193, -29.55182921846484945, 7.778495531946296282 ) ) ;
#7197 = ORIENTED_EDGE ( 'NONE', *, *, #40270, .T. ) ;
#7198 = CARTESIAN_POINT ( 'NONE',  ( -67.83000114521873058, 27.33924089054923101, 12.50000000000000000 ) ) ;
#7199 = CARTESIAN_POINT ( 'NONE',  ( 5.069616211753222856, -29.11340517107872472, 6.865312560952602894 ) ) ;
#7200 = AXIS2_PLACEMENT_3D ( 'NONE', #19695, #26080, #1182 ) ;
#7201 = CARTESIAN_POINT ( 'NONE',  ( 30.51645556077223631, -0.1367088690802835960, -4.969228952161986790 ) ) ;
#7202 = CARTESIAN_POINT ( 'NONE',  ( 0.5713750229309367823, -32.77700439067807281, 7.695279973900954751 ) ) ;
#7203 = CARTESIAN_POINT ( 'NONE',  ( -70.92837670882107659, -60.53509472482660669, -7.538952224936807056 ) ) ;
#7204 =( BOUNDED_CURVE ( )  B_SPLINE_CURVE ( 3, ( #13384, #36227, #26366, #38493 ),
 .UNSPECIFIED., .F., .F. ) 
 B_SPLINE_CURVE_WITH_KNOTS ( ( 4, 4 ),
 ( 1.347909859412853351, 1.534781240595297636 ),
 .UNSPECIFIED. ) 
 CURVE ( )  GEOMETRIC_REPRESENTATION_ITEM ( )  RATIONAL_B_SPLINE_CURVE ( ( 1.000000000000000000, 0.9970920404276226723, 0.9970920404276226723, 1.000000000000000000 ) ) 
 REPRESENTATION_ITEM ( '' )  );
#7205 = EDGE_LOOP ( 'NONE', ( #1169, #39297, #2018, #37281 ) ) ;
#7206 = CARTESIAN_POINT ( 'NONE',  ( -75.45330471031414277, 33.71485196875532608, 8.800414904976364028 ) ) ;
#7207 = DIRECTION ( 'NONE',  ( 1.000000000000000000, 0.000000000000000000, 0.000000000000000000 ) ) ;
#7208 = CARTESIAN_POINT ( 'NONE',  ( 28.62762293107049416, -3.097373597580966642, 4.674430938707033967 ) ) ;
#7209 = ORIENTED_EDGE ( 'NONE', *, *, #18438, .T. ) ;
#7210 = ORIENTED_EDGE ( 'NONE', *, *, #38857, .F. ) ;
#7211 = CARTESIAN_POINT ( 'NONE',  ( 33.94565407617458419, -0.4887086158907474887, 5.122328562820444908 ) ) ;
#7212 = CARTESIAN_POINT ( 'NONE',  ( 1.640982164150366795, -33.05455003082661136, 7.785593909369613819 ) ) ;
#7213 = DIRECTION ( 'NONE',  ( -0.000000000000000000, 0.000000000000000000, 1.000000000000000000 ) ) ;
#7214 = CARTESIAN_POINT ( 'NONE',  ( 87.70554304502432785, -2.246019397594158473, 2.665219128644956914 ) ) ;
#7215 = VERTEX_POINT ( 'NONE', #27892 ) ;
#7216 = AXIS2_PLACEMENT_3D ( 'NONE', #13784, #6805, #2986 ) ;
#7217 = EDGE_CURVE ( 'NONE', #24455, #4723, #26637, .T. ) ;
#7218 = VERTEX_POINT ( 'NONE', #27689 ) ;
#7219 = EDGE_CURVE ( 'NONE', #34912, #7860, #3029, .T. ) ;
#7220 = CARTESIAN_POINT ( 'NONE',  ( -18.97867591359219475, -26.64985754041175525, 6.800000000000000711 ) ) ;
#7221 = DIRECTION ( 'NONE',  ( -0.000000000000000000, -1.000000000000000000, -0.000000000000000000 ) ) ;
#7222 = VERTEX_POINT ( 'NONE', #729 ) ;
#7223 = CARTESIAN_POINT ( 'NONE',  ( -57.59497484894375674, 32.71166363405644262, -4.078840986107554301 ) ) ;
#7224 = CARTESIAN_POINT ( 'NONE',  ( 2.586165941411596947, -24.87425163552211416, 7.013842709614101167 ) ) ;
#7225 = ORIENTED_EDGE ( 'NONE', *, *, #31175, .T. ) ;
#7226 = CARTESIAN_POINT ( 'NONE',  ( 79.96508732583350820, 66.32411498806374084, -1.465650077276903218 ) ) ;
#7227 = VECTOR ( 'NONE', #19059, 1000.000000000000000 ) ;
#7228 = CYLINDRICAL_SURFACE ( 'NONE', #35135, 2.500000000000000444 ) ;
#7229 = ORIENTED_EDGE ( 'NONE', *, *, #18206, .F. ) ;
#7230 = CARTESIAN_POINT ( 'NONE',  ( 76.39232039721476042, 61.07121484735997541, -3.784676997173953783 ) ) ;
#7232 = CARTESIAN_POINT ( 'NONE',  ( -70.92837670882107659, 28.72470171467712063, -2.000000000000000000 ) ) ;
#7231 = CARTESIAN_POINT ( 'NONE',  ( -1.600658481268678823, -28.40671124064021669, 7.686927408461905920 ) ) ;
#7233 = CARTESIAN_POINT ( 'NONE',  ( -69.92837670882107659, -0.6505659821428084744, 5.916079783099619682 ) ) ;
#7234 = CARTESIAN_POINT ( 'NONE',  ( 75.95345872531818543, 63.43160129075360487, 3.385286751594689836 ) ) ;
#7235 = B_SPLINE_CURVE_WITH_KNOTS ( 'NONE', 3,
 ( #502, #18806, #31379, #3205, #22328, #28278, #25599, #97, #26414, #29096, #26809, #32994, #17312, #4192, #20414, #10138, #22728, #1309, #4589, #10941, #1113, #22922, #4779, #10542, #20217, #19628, #29889, #32800, #1707, #32399, #23520 ),
 .UNSPECIFIED., .F., .F.,
 ( 4, 3, 3, 3, 3, 3, 3, 3, 3, 3, 4 ),
 ( 1.226634733346699349E-18, 3.077658087705631944E-05, 6.152638666998957247E-05, 9.267501192706370972E-05, 0.0001241882240135194695, 0.0001556618703051673421, 0.0001866161554452211652, 0.0002167966385860971171, 0.0002463805737537774895, 0.0002758761370306536285, 0.0002847094172290096569 ),
 .UNSPECIFIED. ) ;
#7236 = CARTESIAN_POINT ( 'NONE',  ( 4.376998081151240783, -27.47332109273945733, 6.864276522220859711 ) ) ;
#7237 = FACE_OUTER_BOUND ( 'NONE', #37435, .T. ) ;
#7238 = CARTESIAN_POINT ( 'NONE',  ( 23.52943196063522535, 3.064722609491274952, -3.878734937556255868 ) ) ;
#7239 = CARTESIAN_POINT ( 'NONE',  ( 1.685055500909720561, -26.06996366628073858, 7.637894019485640840 ) ) ;
#7240 = CARTESIAN_POINT ( 'NONE',  ( 79.46293960946097457, 66.21290357410885008, 1.708467252431127070 ) ) ;
#7241 = CARTESIAN_POINT ( 'NONE',  ( -0.1737877179784135528, -32.52584925061469789, 6.875780273367531947 ) ) ;
#7242 = CARTESIAN_POINT ( 'NONE',  ( 30.13572739226143327, -4.670734905539763560, 0.4584422186006349986 ) ) ;
#7243 = CARTESIAN_POINT ( 'NONE',  ( 2.311026925537185139, -26.22520041558805914, 7.779495906702013741 ) ) ;
#7244 = CARTESIAN_POINT ( 'NONE',  ( 3.569994541659591736, -26.73010724343094324, 6.997764925645180156 ) ) ;
#7245 = DIRECTION ( 'NONE',  ( -1.000000000000000000, 0.000000000000000000, 0.000000000000000000 ) ) ;
#7246 = DIRECTION ( 'NONE',  ( 0.000000000000000000, -0.6834397476448832442, -0.7300069255418734082 ) ) ;
#7247 = CARTESIAN_POINT ( 'NONE',  ( 67.92755604491691201, 57.95366386773438450, 3.974145956335496166 ) ) ;
#7248 = CARTESIAN_POINT ( 'NONE',  ( 20.76538241992246014, 4.421523770943674769, -3.217089656416562082 ) ) ;
#7249 = CARTESIAN_POINT ( 'NONE',  ( 1.080192182740615126, -32.91288614359101672, 7.782167645815904145 ) ) ;
#7250 = FACE_OUTER_BOUND ( 'NONE', #24531, .T. ) ;
#7251 = CARTESIAN_POINT ( 'NONE',  ( 3.306242093667368653, -32.56681097908001732, 7.768425012602591551 ) ) ;
#7252 = CARTESIAN_POINT ( 'NONE',  ( -63.16615724057117376, 41.45860378058512907, -4.000000000000000000 ) ) ;
#7253 = LINE ( 'NONE', #10341, #30052 ) ;
#7254 = DIRECTION ( 'NONE',  ( 0.000000000000000000, 0.000000000000000000, 1.000000000000000000 ) ) ;
#7255 = AXIS2_PLACEMENT_3D ( 'NONE', #23360, #4632, #942 ) ;
#7256 = ORIENTED_EDGE ( 'NONE', *, *, #28030, .F. ) ;
#7257 = CARTESIAN_POINT ( 'NONE',  ( 36.68208917225820187, -3.313352327499882843, 5.912027108166803657 ) ) ;
#7258 = PLANE ( 'NONE',  #4763 ) ;
#7259 = CARTESIAN_POINT ( 'NONE',  ( 67.46313568882432321, 58.11475875142180314, -3.998123450764770048 ) ) ;
#7260 = CARTESIAN_POINT ( 'NONE',  ( 1.713892699967726196, -25.86893018339335271, 7.635761828346577573 ) ) ;
#7261 = ORIENTED_EDGE ( 'NONE', *, *, #12068, .T. ) ;
#7262 = DIRECTION ( 'NONE',  ( -0.000000000000000000, -1.000000000000000000, -0.000000000000000000 ) ) ;
#7264 = EDGE_CURVE ( 'NONE', #2177, #7027, #23350, .T. ) ;
#7263 = CARTESIAN_POINT ( 'NONE',  ( 30.89397235467784597, -3.431564488292946358, 4.935950646977611989 ) ) ;
#7265 = CARTESIAN_POINT ( 'NONE',  ( 22.60554062051026136, 3.598027713168910235, 3.981257213926762795 ) ) ;
#7266 = CARTESIAN_POINT ( 'NONE',  ( 2.326171464738295835, -32.91184545387483951, 7.693875151218753317 ) ) ;
#7267 = CARTESIAN_POINT ( 'NONE',  ( -1.457564949911021479, -28.30999727367718322, 6.864651958020304257 ) ) ;
#7268 = DIRECTION ( 'NONE',  ( -0.4999999999999918954, -0.8660254037844432595, -0.000000000000000000 ) ) ;
#7269 = LINE ( 'NONE', #29104, #28453 ) ;
#7270 = VERTEX_POINT ( 'NONE', #536 ) ;
#7271 = CARTESIAN_POINT ( 'NONE',  ( 24.06785808357873080, 3.349623670569857659, 3.203142401354519553 ) ) ;
#7272 = AXIS2_PLACEMENT_3D ( 'NONE', #38288, #10088, #34425 ) ;
#7273 = CARTESIAN_POINT ( 'NONE',  ( -1.740147594125142749, -30.21234809103664176, 7.710604733652633769 ) ) ;
#7274 = CARTESIAN_POINT ( 'NONE',  ( 80.13254067770888867, 64.54635310605580401, 3.552238747020026732 ) ) ;
#7275 = FACE_OUTER_BOUND ( 'NONE', #10490, .T. ) ;
#7276 = ORIENTED_EDGE ( 'NONE', *, *, #11043, .T. ) ;
#7277 = CARTESIAN_POINT ( 'NONE',  ( 78.00211021922338261, 65.46497694724934036, -2.177161688561012998 ) ) ;
#7279 = CARTESIAN_POINT ( 'NONE',  ( 14.69274635589773581, -4.522481898537247247, -2.499999999999558575 ) ) ;
#7278 = CARTESIAN_POINT ( 'NONE',  ( 22.29898859944773903, 0.2633200660602942333, 7.098944222140404214 ) ) ;
#7280 = CARTESIAN_POINT ( 'NONE',  ( 79.02544788879461635, 66.13175326451417391, -1.679744683809666350 ) ) ;
#7281 = CARTESIAN_POINT ( 'NONE',  ( 78.71580656266537801, 64.90148335848421368, 3.195657361810692709 ) ) ;
#7282 = CARTESIAN_POINT ( 'NONE',  ( 5.118969260771242702, -33.45454016556441701, 7.754798119455333705 ) ) ;
#7283 = VECTOR ( 'NONE', #13224, 1000.000000000000000 ) ;
#7284 = CARTESIAN_POINT ( 'NONE',  ( 81.85052347209639834, 65.46610162458738102, 1.468380750527791268 ) ) ;
#7285 = FACE_OUTER_BOUND ( 'NONE', #26338, .T. ) ;
#7286 = CARTESIAN_POINT ( 'NONE',  ( 22.33594428049882197, 5.124660873843202680, 5.347558210918236909 ) ) ;
#7287 = EDGE_CURVE ( 'NONE', #9413, #8630, #36911, .T. ) ;
#7288 = CARTESIAN_POINT ( 'NONE',  ( -1.599034431228576247, -30.73774772367137942, 6.894806418505347700 ) ) ;
#7289 = ORIENTED_EDGE ( 'NONE', *, *, #15777, .F. ) ;
#7290 = CARTESIAN_POINT ( 'NONE',  ( -79.27250537723340074, -5.532529408078902478, 5.525611224659603415 ) ) ;
#7291 = CARTESIAN_POINT ( 'NONE',  ( 22.28290334446566945, 0.2420565227163372635, -7.135904416810470607 ) ) ;
#7292 = FACE_OUTER_BOUND ( 'NONE', #33331, .T. ) ;
#7293 = ORIENTED_EDGE ( 'NONE', *, *, #20123, .T. ) ;
#7294 = CARTESIAN_POINT ( 'NONE',  ( -2.448748702180640446, -26.64985754041175525, 6.700000000000000178 ) ) ;
#7295 = ORIENTED_EDGE ( 'NONE', *, *, #9204, .T. ) ;
#7296 = CARTESIAN_POINT ( 'NONE',  ( 36.71877240845051205, -3.457495992918012906, -5.861073688215565625 ) ) ;
#7297 = CARTESIAN_POINT ( 'NONE',  ( 30.43983800511932358, -3.117243395012541995, -4.952810734695171746 ) ) ;
#7298 = CARTESIAN_POINT ( 'NONE',  ( 3.281677335269463036, -32.69235404666142841, 6.941203072598471024 ) ) ;
#7299 = CARTESIAN_POINT ( 'NONE',  ( -1.086691373026069884, -31.68704541418143705, 6.895394898881671786 ) ) ;
#7300 = PLANE ( 'NONE',  #17299 ) ;
#7301 = CARTESIAN_POINT ( 'NONE',  ( -0.8998472737371643326, -27.22723292372361570, 7.753200566781576875 ) ) ;
#7302 = ADVANCED_FACE ( 'NONE', ( #29532 ), #29330, .T. ) ;
#7303 = CIRCLE ( 'NONE', #96, 0.1000000000000028644 ) ;
#7304 = EDGE_CURVE ( 'NONE', #10217, #18938, #35523, .T. ) ;
#7305 = DIRECTION ( 'NONE',  ( 0.000000000000000000, 0.000000000000000000, -1.000000000000000000 ) ) ;
#7306 = CARTESIAN_POINT ( 'NONE',  ( 24.08611371057580186, 0.7123248832134593256, -5.071621260587827251 ) ) ;
#7307 = LINE ( 'NONE', #28735, #26249 ) ;
#7308 = B_SPLINE_CURVE_WITH_KNOTS ( 'NONE', 3,
 ( #15158, #17617, #14953, #11852, #36178, #30626, #7959, #27716, #11438, #24428, #20508, #27520, #33304, #14332, #23801, #14734, #24003, #30195, #33091, #2015, #17824, #4875, #5287, #27306, #14532, #36578, #30405, #39868, #17410, #29994, #1808 ),
 .UNSPECIFIED., .F., .F.,
 ( 4, 3, 3, 3, 3, 3, 3, 3, 3, 3, 4 ),
 ( 0.000000000000000000, 2.999644130997589661E-05, 6.002588995694634868E-05, 8.960886084587892835E-05, 0.0001190604700446500010, 0.0001489538463052705820, 0.0001796139255493957678, 0.0002109707048517079188, 0.0002426195318110312908, 0.0002740640997890033651, 0.0002849778069099850159 ),
 .UNSPECIFIED. ) ;
#7309 = CARTESIAN_POINT ( 'NONE',  ( 2.235028438126618333, -33.02886990452594063, 6.867280401193707640 ) ) ;
#7310 = ORIENTED_EDGE ( 'NONE', *, *, #24184, .T. ) ;
#7311 = CARTESIAN_POINT ( 'NONE',  ( 66.90064367344375285, 57.83598502562791310, 3.997265020308770289 ) ) ;
#7312 = CARTESIAN_POINT ( 'NONE',  ( 85.62750488955801131, 0.9367966501063212936, -5.850367371124844063 ) ) ;
#7313 = ADVANCED_FACE ( 'NONE', ( #10772 ), #13072, .F. ) ;
#7314 = ORIENTED_EDGE ( 'NONE', *, *, #32458, .T. ) ;
#7315 = CARTESIAN_POINT ( 'NONE',  ( -75.87812283331165020, 8.749605185975593002, -10.12194526897379099 ) ) ;
#7316 = PRODUCT_CONTEXT ( 'NONE', #8952, 'mechanical' ) ;
#7317 = CARTESIAN_POINT ( 'NONE',  ( 2.251363620182238456, -32.92500435510202550, 7.784838882742139532 ) ) ;
#7318 = CARTESIAN_POINT ( 'NONE',  ( 1.093737980128993037, -26.12620165286623930, 7.767720160662275219 ) ) ;
#7319 = ORIENTED_EDGE ( 'NONE', *, *, #13383, .T. ) ;
#7320 = DIRECTION ( 'NONE',  ( -0.000000000000000000, -1.000000000000000000, -0.000000000000000000 ) ) ;
#7321 = ORIENTED_EDGE ( 'NONE', *, *, #24917, .F. ) ;
#7322 = CARTESIAN_POINT ( 'NONE',  ( 79.45016587565679345, 64.47252957033367693, -3.557377001560570573 ) ) ;
#7323 = B_SPLINE_CURVE_WITH_KNOTS ( 'NONE', 3,
 ( #21337, #14722, #8753, #4672, #33080, #17207, #4865, #17400, #14322, #33292 ),
 .UNSPECIFIED., .F., .F.,
 ( 4, 3, 3, 4 ),
 ( 0.000000000000000000, 3.025505781527821749E-05, 6.051003801291572674E-05, 6.468145402690739221E-05 ),
 .UNSPECIFIED. ) ;
#7324 = CARTESIAN_POINT ( 'NONE',  ( 33.87523647309109265, -5.320081038359204761, 1.808392000078312467 ) ) ;
#7325 = CARTESIAN_POINT ( 'NONE',  ( 79.07938959848826244, 65.20837507400389654, 3.070011659370390777 ) ) ;
#7327 = ORIENTED_EDGE ( 'NONE', *, *, #32705, .F. ) ;
#7326 = DIRECTION ( 'NONE',  ( 0.3420201433256790380, -0.9396926207859046531, -0.000000000000000000 ) ) ;
#7328 = EDGE_CURVE ( 'NONE', #20273, #18938, #35123, .T. ) ;
#7329 = DIRECTION ( 'NONE',  ( 0.000000000000000000, 1.000000000000000000, 0.000000000000000000 ) ) ;
#7330 = CARTESIAN_POINT ( 'NONE',  ( 0.9751061736955158876, -32.99397343253602344, 6.865706122441728176 ) ) ;
#7331 = CARTESIAN_POINT ( 'NONE',  ( -1.785187679209235379, -29.50141875348822751, 7.784513003884693916 ) ) ;
#7332 = DIRECTION ( 'NONE',  ( -0.000000000000000000, -1.000000000000000000, -0.000000000000000000 ) ) ;
#7333 = CARTESIAN_POINT ( 'NONE',  ( 4.946955026107762166, -30.87529236204174765, 7.761113333117553914 ) ) ;
#7334 = CARTESIAN_POINT ( 'NONE',  ( 22.18599700961289756, 5.272392256036439129, -3.073166440102835573 ) ) ;
#7335 = ORIENTED_EDGE ( 'NONE', *, *, #40621, .F. ) ;
#7336 = CARTESIAN_POINT ( 'NONE',  ( 14.75467646479344097, -5.149013399961007487, -2.500000000000000000 ) ) ;
#7337 = LINE ( 'NONE', #6942, #33326 ) ;
#7338 = AXIS2_PLACEMENT_3D ( 'NONE', #2088, #14600, #27172 ) ;
#7339 = CARTESIAN_POINT ( 'NONE',  ( -73.13193655429402895, 4.589176838546805470, -10.93047759564017696 ) ) ;
#7340 = CARTESIAN_POINT ( 'NONE',  ( -30.44874870218064089, -25.49307895267003587, 6.800000000000000711 ) ) ;
#7341 = DIRECTION ( 'NONE',  ( 1.000000000000000000, -1.061555284671232059E-15, 0.000000000000000000 ) ) ;
#7342 = CARTESIAN_POINT ( 'NONE',  ( 80.22001885188443282, 64.95903095167625452, 3.330128783915578872 ) ) ;
#7343 = DIRECTION ( 'NONE',  ( -0.000000000000000000, 1.000000000000000000, -0.000000000000000000 ) ) ;
#7344 = CARTESIAN_POINT ( 'NONE',  ( 21.58874331597417040, 7.202613857503122219, -2.924296597703472500 ) ) ;
#7345 = DIRECTION ( 'NONE',  ( 1.000000000000000000, 0.000000000000000000, 0.000000000000000000 ) ) ;
#7346 = CARTESIAN_POINT ( 'NONE',  ( 3.923056598701467834, -26.86627451898972652, 7.710604733652633769 ) ) ;
#7347 = EDGE_CURVE ( 'NONE', #24455, #19192, #13879, .T. ) ;
#7348 = EDGE_CURVE ( 'NONE', #30583, #35921, #38973, .T. ) ;
#7349 = EDGE_CURVE ( 'NONE', #34241, #24116, #9979, .T. ) ;
#7350 = CARTESIAN_POINT ( 'NONE',  ( -64.66796849410252435, 36.23110552202045653, 6.165526157072420688 ) ) ;
#7351 = CARTESIAN_POINT ( 'NONE',  ( 14.77222812468899349, 12.33286846116284252, -2.511961485181726239 ) ) ;
#7352 = CARTESIAN_POINT ( 'NONE',  ( 4.886820230737117576, -28.38388714888618480, 7.740055089680400791 ) ) ;
#7353 = CYLINDRICAL_SURFACE ( 'NONE', #2358, 8.204531065793066347 ) ;
#7354 = ORIENTED_EDGE ( 'NONE', *, *, #17829, .F. ) ;
#7355 = CARTESIAN_POINT ( 'NONE',  ( 69.21678231378241719, 58.76388891306111617, 3.990151341881419622 ) ) ;
#7356 = CARTESIAN_POINT ( 'NONE',  ( 34.33282722039242429, -1.486069782136362205, 5.564866048942920251 ) ) ;
#7357 = B_SPLINE_CURVE_WITH_KNOTS ( 'NONE', 3,
 ( #8551, #8957, #3038, #14721, #24414, #34122, #18021, #11630 ),
 .UNSPECIFIED., .F., .F.,
 ( 4, 2, 2, 4 ),
 ( 0.000000000000000000, 0.1250305178534032724, 0.2500610357068065448, 0.5001220714136037637 ),
 .UNSPECIFIED. ) ;
#7358 = CARTESIAN_POINT ( 'NONE',  ( -40.87867591359218977, -24.55319635012989110, 6.700000000000000178 ) ) ;
#7359 = CARTESIAN_POINT ( 'NONE',  ( 86.12362567153361681, 1.619580568575353485, 4.895344567657775592 ) ) ;
#7361 = CARTESIAN_POINT ( 'NONE',  ( 4.826124500149282959, -30.90777074620061171, 6.895222827070020877 ) ) ;
#7360 = CARTESIAN_POINT ( 'NONE',  ( 81.20616577872307573, 61.45478060783982244, -1.852607187800904942 ) ) ;
#7362 = CARTESIAN_POINT ( 'NONE',  ( 4.372846383550529126, -27.30984669459420289, 7.635761828346578461 ) ) ;
#7363 = CARTESIAN_POINT ( 'NONE',  ( 87.73735837800707316, -0.1930405997103058768, -3.830955553240402711 ) ) ;
#7364 = VERTEX_POINT ( 'NONE', #7700 ) ;
#7365 = CARTESIAN_POINT ( 'NONE',  ( 4.907037958954144408, -30.70015833522101545, 7.712764235869105534 ) ) ;
#7366 = VERTEX_POINT ( 'NONE', #16355 ) ;
#7367 = CARTESIAN_POINT ( 'NONE',  ( -71.26311553261176357, -21.73200267494512161, 6.003704795174108710 ) ) ;
#7368 = ORIENTED_EDGE ( 'NONE', *, *, #15054, .F. ) ;
#7369 = CARTESIAN_POINT ( 'NONE',  ( 80.72314371186274684, 62.66258842508732840, -3.386558198656251406 ) ) ;
#7370 = DIRECTION ( 'NONE',  ( -0.000000000000000000, -0.000000000000000000, -1.000000000000000000 ) ) ;
#7371 = CARTESIAN_POINT ( 'NONE',  ( 78.77108537463557525, 65.94663689831973841, 1.925402693829579626 ) ) ;
#7372 = CARTESIAN_POINT ( 'NONE',  ( 23.45630354681979313, 1.541145148875956883, 5.001686380149122257 ) ) ;
#7374 = ORIENTED_EDGE ( 'NONE', *, *, #30465, .F. ) ;
#7373 = CIRCLE ( 'NONE', #38929, 98.38357402481355507 ) ;
#7375 = DIRECTION ( 'NONE',  ( 0.000000000000000000, 0.7541618601367601205, -0.6566885781822779933 ) ) ;
#7377 = CARTESIAN_POINT ( 'NONE',  ( 85.15174684586190779, 2.711240993721571790, -0.5174129942806917626 ) ) ;
#7376 = CARTESIAN_POINT ( 'NONE',  ( 14.73750015949766023, 12.90700633730901359, -2.501527175807457759 ) ) ;
#7378 = LINE ( 'NONE', #13558, #17838 ) ;
#7379 = CARTESIAN_POINT ( 'NONE',  ( -64.08758708074093136, 42.96264881669708302, -3.162281979264331966 ) ) ;
#7380 = CARTESIAN_POINT ( 'NONE',  ( 72.04157359233609270, 60.08177168861285367, 3.962431611490357053 ) ) ;
#7381 = ORIENTED_EDGE ( 'NONE', *, *, #16004, .F. ) ;
#7382 = CARTESIAN_POINT ( 'NONE',  ( 23.17191900141983041, 3.801330203260075091, -3.394942160406552834 ) ) ;
#7383 = ORIENTED_EDGE ( 'NONE', *, *, #1940, .T. ) ;
#7384 = CARTESIAN_POINT ( 'NONE',  ( 5.123272199033605645, -30.27793340842993786, 7.771081512783704071 ) ) ;
#7385 = EDGE_CURVE ( 'NONE', #40564, #27839, #20610, .T. ) ;
#7386 = ORIENTED_EDGE ( 'NONE', *, *, #39361, .T. ) ;
#7387 = CARTESIAN_POINT ( 'NONE',  ( 21.85643539959776049, -13.25144142801168634, -1.676981927294508345 ) ) ;
#7388 = EDGE_CURVE ( 'NONE', #25777, #2799, #28217, .T. ) ;
#7389 = CARTESIAN_POINT ( 'NONE',  ( 21.80882946373430542, 5.293150380057753956, 3.367598806148119905 ) ) ;
#7390 = ORIENTED_EDGE ( 'NONE', *, *, #32756, .F. ) ;
#7391 = CARTESIAN_POINT ( 'NONE',  ( 0.3765978019783249309, -32.70163482617414275, 6.882085323592684212 ) ) ;
#7392 = CARTESIAN_POINT ( 'NONE',  ( 81.48777377602155525, 63.71638886500237220, 3.187395722566881862 ) ) ;
#7393 = CARTESIAN_POINT ( 'NONE',  ( 88.18839210903504977, -0.8832026502337909646, 4.329116466421397469 ) ) ;
#7394 = CYLINDRICAL_SURFACE ( 'NONE', #36478, 3.399999999999999911 ) ;
#7395 = ORIENTED_EDGE ( 'NONE', *, *, #7107, .F. ) ;
#7396 = EDGE_CURVE ( 'NONE', #19528, #5651, #29686, .T. ) ;
#7397 = CARTESIAN_POINT ( 'NONE',  ( -81.15124214773400979, -5.648850483656841170, 4.015016724928055503 ) ) ;
#7398 = CARTESIAN_POINT ( 'NONE',  ( 14.59363405247780321, -5.046850784924433064, 2.484087560899213010 ) ) ;
#7399 = CARTESIAN_POINT ( 'NONE',  ( 31.28009924878942627, -3.760136573936985194, 4.659093935210213644 ) ) ;
#7400 = CARTESIAN_POINT ( 'NONE',  ( 17.00076660167203357, -3.039841025278140041, -2.859778811921668940 ) ) ;
#7401 = CARTESIAN_POINT ( 'NONE',  ( 20.42384695622214963, 3.665139109075679524, -3.394033288760437639 ) ) ;
#7402 = CARTESIAN_POINT ( 'NONE',  ( 0.5616195162123727158, -32.77355560770597975, 7.652160403243383868 ) ) ;
#7403 = CARTESIAN_POINT ( 'NONE',  ( 85.08263568025058987, 1.762786880713592463, 5.091211749826051403 ) ) ;
#7404 = DIRECTION ( 'NONE',  ( 1.000000000000000000, 0.000000000000000000, 0.000000000000000000 ) ) ;
#7405 = CARTESIAN_POINT ( 'NONE',  ( -5.078675913592192614, -26.64985754041175525, 6.800000000000000711 ) ) ;
#7406 = CARTESIAN_POINT ( 'NONE',  ( -1.641762495386305254, -30.19444782469885880, 7.712764235869103757 ) ) ;
#7407 = CARTESIAN_POINT ( 'NONE',  ( 4.998738087972761868, -28.44140482322499963, 7.784725160561909441 ) ) ;
#7408 = ORIENTED_EDGE ( 'NONE', *, *, #14620, .F. ) ;
#7409 = VERTEX_POINT ( 'NONE', #20449 ) ;
#7410 = CARTESIAN_POINT ( 'NONE',  ( 34.63713585988073618, -0.7818613632861374230, 5.275101436747132055 ) ) ;
#7411 = CARTESIAN_POINT ( 'NONE',  ( -1.613161587038500766, -30.69708474973657530, 6.867280401193708528 ) ) ;
#7412 = LINE ( 'NONE', #4733, #37241 ) ;
#7413 = CARTESIAN_POINT ( 'NONE',  ( 86.30560996193628398, -0.3002381051633802866, 5.887336558433836409 ) ) ;
#7414 = ORIENTED_EDGE ( 'NONE', *, *, #7837, .F. ) ;
#7415 = LINE ( 'NONE', #1265, #25983 ) ;
#7416 = ORIENTED_EDGE ( 'NONE', *, *, #27185, .T. ) ;
#7417 = CARTESIAN_POINT ( 'NONE',  ( -58.33732831438487665, 31.01206039140789983, -4.738023936417821602 ) ) ;
#7418 = CARTESIAN_POINT ( 'NONE',  ( 3.805094080858060668, -32.36639755374996241, 6.989977667959446528 ) ) ;
#7419 = EDGE_LOOP ( 'NONE', ( #24341, #10477, #1753, #30453 ) ) ;
#7420 = CARTESIAN_POINT ( 'NONE',  ( 22.73433657433409749, 4.113458136755731687, 3.466401380080733396 ) ) ;
#7421 = CARTESIAN_POINT ( 'NONE',  ( 79.31644831670712392, 66.29498274501729327, -1.214491505233945334 ) ) ;
#7422 = B_SPLINE_CURVE_WITH_KNOTS ( 'NONE', 3,
 ( #4574, #11882, #29672, #17493, #27747, #2872, #40494, #26590, #5732, #17296, #29874, #1484, #14018, #14989 ),
 .UNSPECIFIED., .F., .F.,
 ( 4, 2, 2, 2, 2, 2, 4 ),
 ( 0.000000000000000000, 0.0002935890969200457981, 0.0005871781938400915963, 0.0008807672907601373944, 0.001174356387680183193, 0.001761534581520288884, 0.002348712775360395008 ),
 .UNSPECIFIED. ) ;
#7423 = CARTESIAN_POINT ( 'NONE',  ( -69.92837670882107659, -20.78299143688747819, 5.916079783099620570 ) ) ;
#7424 = VERTEX_POINT ( 'NONE', #32832 ) ;
#7425 = CARTESIAN_POINT ( 'NONE',  ( 75.34312381977423456, 60.33875818837522331, -3.724166978290133212 ) ) ;
#7427 = DIRECTION ( 'NONE',  ( 0.000000000000000000, 1.000000000000000000, 0.000000000000000000 ) ) ;
#7426 = CARTESIAN_POINT ( 'NONE',  ( -1.593833517588955972, -28.38751944612305422, 7.638132480492516585 ) ) ;
#7428 = CARTESIAN_POINT ( 'NONE',  ( 21.28603936774592498, 5.337095168022400138, -3.528599266780989563 ) ) ;
#7429 = CARTESIAN_POINT ( 'NONE',  ( 77.29563288604623494, 62.10585478181953079, 3.856837490696072290 ) ) ;
#7430 = AXIS2_PLACEMENT_3D ( 'NONE', #2036, #29609, #20738 ) ;
#7431 = FACE_OUTER_BOUND ( 'NONE', #6994, .T. ) ;
#7432 = CARTESIAN_POINT ( 'NONE',  ( 1.810168977974152105, -26.07424362682720442, 7.766640943994646662 ) ) ;
#7433 = DIRECTION ( 'NONE',  ( -1.000000000000000000, 0.000000000000000000, 0.000000000000000000 ) ) ;
#7434 = FACE_BOUND ( 'NONE', #33299, .T. ) ;
#7435 = CARTESIAN_POINT ( 'NONE',  ( 82.15165036511250207, 63.00212529317524002, 2.340562087103263078 ) ) ;
#7436 =( BOUNDED_CURVE ( )  B_SPLINE_CURVE ( 3, ( #38688, #32934, #19958, #13790 ),
 .UNSPECIFIED., .F., .T. ) 
 B_SPLINE_CURVE_WITH_KNOTS ( ( 4, 4 ),
 ( 1.347909859412854017, 1.534781240595299634 ),
 .UNSPECIFIED. ) 
 CURVE ( )  GEOMETRIC_REPRESENTATION_ITEM ( )  RATIONAL_B_SPLINE_CURVE ( ( 1.000000000000000000, 0.9970920404276225613, 0.9970920404276225613, 1.000000000000000000 ) ) 
 REPRESENTATION_ITEM ( '' )  );
#7437 = CARTESIAN_POINT ( 'NONE',  ( -0.2037329942765146173, -32.50665443916160058, 6.998987538705438105 ) ) ;
#7438 = CARTESIAN_POINT ( 'NONE',  ( 32.02627343617642453, -1.895034194620857315, -5.999511542327915947 ) ) ;
#7439 = B_SPLINE_CURVE_WITH_KNOTS ( 'NONE', 3,
 ( #4032, #6702, #13267, #19251 ),
 .UNSPECIFIED., .F., .F.,
 ( 4, 4 ),
 ( 0.000000000000000000, 6.391136169898433355E-06 ),
 .UNSPECIFIED. ) ;
#7440 = CARTESIAN_POINT ( 'NONE',  ( -0.8688903936063803179, -27.19321022093548734, 7.013842709614101167 ) ) ;
#7441 = ADVANCED_FACE ( 'NONE', ( #33027 ), #1741, .F. ) ;
#7442 = EDGE_CURVE ( 'NONE', #27839, #35245, #3027, .T. ) ;
#7443 = CARTESIAN_POINT ( 'NONE',  ( -75.12839812606507905, -3.199487166374271663, -10.43546860170108026 ) ) ;
#7444 = ORIENTED_EDGE ( 'NONE', *, *, #15097, .F. ) ;
#7445 = CARTESIAN_POINT ( 'NONE',  ( -24.97867591359219475, -24.55319635012989110, 6.800000000000000711 ) ) ;
#7446 = VECTOR ( 'NONE', #15507, 1000.000000000000000 ) ;
#7447 = LINE ( 'NONE', #687, #9836 ) ;
#7448 = EDGE_CURVE ( 'NONE', #11412, #34747, #17551, .T. ) ;
#7449 = CARTESIAN_POINT ( 'NONE',  ( 30.74497410374950945, 0.4681497935174912528, -4.860627807659219535 ) ) ;
#7450 = DIRECTION ( 'NONE',  ( -0.000000000000000000, -1.000000000000000000, -0.000000000000000000 ) ) ;
#7451 = DIRECTION ( 'NONE',  ( -0.000000000000000000, -0.000000000000000000, -1.000000000000000000 ) ) ;
#7452 = CARTESIAN_POINT ( 'NONE',  ( -34.97867591359219830, -24.55319635012989110, 6.800000000000000711 ) ) ;
#7453 = DIRECTION ( 'NONE',  ( 0.000000000000000000, 0.000000000000000000, 1.000000000000000000 ) ) ;
#7454 = DIRECTION ( 'NONE',  ( 0.000000000000000000, 0.000000000000000000, 1.000000000000000000 ) ) ;
#7455 = AXIS2_PLACEMENT_3D ( 'NONE', #36732, #26859, #30364 ) ;
#7456 = CARTESIAN_POINT ( 'NONE',  ( -73.45070404594234503, 38.65432087843066711, 9.800414904976365804 ) ) ;
#7457 = CARTESIAN_POINT ( 'NONE',  ( -4.444218661349752963, -35.94265729135299381, 6.000000000000000000 ) ) ;
#7458 = ORIENTED_EDGE ( 'NONE', *, *, #2864, .T. ) ;
#7459 = CARTESIAN_POINT ( 'NONE',  ( 36.58893514583110118, -2.079415496222606574, 5.884068123001751083 ) ) ;
#7460 = PLANE ( 'NONE',  #39575 ) ;
#7461 = CARTESIAN_POINT ( 'NONE',  ( 67.38390057489351648, 58.33093658501181267, -3.992553130659726168 ) ) ;
#7462 = LINE ( 'NONE', #7260, #11443 ) ;
#7463 = ORIENTED_EDGE ( 'NONE', *, *, #9860, .T. ) ;
#7464 = CARTESIAN_POINT ( 'NONE',  ( -1.577879219085749574, -30.81516921323670744, 7.255881584735163869 ) ) ;
#7465 = CARTESIAN_POINT ( 'NONE',  ( 30.79039095446131213, -3.336666825807130810, 4.961975926287203187 ) ) ;
#7466 = CARTESIAN_POINT ( 'NONE',  ( 85.00501152238103941, 1.866990000816762585, -4.914164337049770737 ) ) ;
#7467 = CARTESIAN_POINT ( 'NONE',  ( 0.4728567017103387782, -26.29225390702066179, 7.670465701733746755 ) ) ;
#7468 = DIRECTION ( 'NONE',  ( -0.000000000000000000, -0.000000000000000000, 1.000000000000000000 ) ) ;
#7469 = CARTESIAN_POINT ( 'NONE',  ( 4.397682185089559326, -31.80032238106598186, 7.651421919295144924 ) ) ;
#7470 = ORIENTED_EDGE ( 'NONE', *, *, #28244, .T. ) ;
#7471 = CARTESIAN_POINT ( 'NONE',  ( 21.83074723418732432, 5.960639454754549149, 3.136932506330722514 ) ) ;
#7472 = DIRECTION ( 'NONE',  ( 1.000000000000000000, 0.000000000000000000, 0.000000000000000000 ) ) ;
#7474 = VECTOR ( 'NONE', #27507, 1000.000000000000000 ) ;
#7473 = CARTESIAN_POINT ( 'NONE',  ( 79.78769048662040575, 65.07306089581300057, 3.312281065658529311 ) ) ;
#7475 = AXIS2_PLACEMENT_3D ( 'NONE', #30738, #27423, #31137 ) ;
#7476 = DIRECTION ( 'NONE',  ( -0.000000000000000000, -0.000000000000000000, -1.000000000000000000 ) ) ;
#7477 = ORIENTED_EDGE ( 'NONE', *, *, #30227, .T. ) ;
#7478 = CARTESIAN_POINT ( 'NONE',  ( 79.66831987096976775, 61.58041732747442154, -3.164065397988993222 ) ) ;
#7479 = B_SPLINE_CURVE_WITH_KNOTS ( 'NONE', 3,
 ( #23894, #27400, #5180, #30292 ),
 .UNSPECIFIED., .F., .F.,
 ( 4, 4 ),
 ( 2.100641709190665082E-19, 6.391136169898844166E-06 ),
 .UNSPECIFIED. ) ;
#7481 = CARTESIAN_POINT ( 'NONE',  ( -1.717161396028226150, -28.81472039912961591, 6.878836779550822733 ) ) ;
#7480 = CARTESIAN_POINT ( 'NONE',  ( 22.62344975043419026, 0.2992865745580874370, 6.483493247686526573 ) ) ;
#7482 = CARTESIAN_POINT ( 'NONE',  ( 79.42963897889082148, 66.02853703565287447, -2.226826180274442457 ) ) ;
#7483 = CARTESIAN_POINT ( 'NONE',  ( 80.30053069885686057, 62.24503436470106266, 3.340572457511948201 ) ) ;
#7484 = B_SPLINE_CURVE_WITH_KNOTS ( 'NONE', 3,
 ( #18490, #3502, #28592, #13651 ),
 .UNSPECIFIED., .F., .F.,
 ( 4, 4 ),
 ( 0.6621368017907995895, 0.8210829304512126114 ),
 .UNSPECIFIED. ) ;
#7485 = AXIS2_PLACEMENT_3D ( 'NONE', #12835, #40223, #22123 ) ;
#7486 = FACE_OUTER_BOUND ( 'NONE', #22537, .T. ) ;
#7487 = CARTESIAN_POINT ( 'NONE',  ( 82.18775271763095702, 62.23297483488567394, 1.085061034363232979 ) ) ;
#7488 = CARTESIAN_POINT ( 'NONE',  ( -64.08758708074093136, 41.04287353446839148, 3.000000000000000000 ) ) ;
#7489 = CARTESIAN_POINT ( 'NONE',  ( 22.42980438978510449, 1.271109115893125585, 8.904229291692644210 ) ) ;
#7490 = CARTESIAN_POINT ( 'NONE',  ( -64.50921092724659900, 36.42665533667735644, -5.809226461016741894 ) ) ;
#7491 = ORIENTED_EDGE ( 'NONE', *, *, #36349, .F. ) ;
#7492 = CARTESIAN_POINT ( 'NONE',  ( -76.49288603080218252, -4.334318986430696796, 9.797079263697156648 ) ) ;
#7493 = CARTESIAN_POINT ( 'NONE',  ( 24.12420224480490916, 0.5001390095518741807, -5.094071010228495844 ) ) ;
#7494 = CARTESIAN_POINT ( 'NONE',  ( -1.057258846844102873, -31.72486802769777725, 7.754798119455333705 ) ) ;
#7495 = EDGE_CURVE ( 'NONE', #19268, #39722, #29723, .T. ) ;
#7496 = CARTESIAN_POINT ( 'NONE',  ( 37.18637049283714191, -2.963493602741866351, -6.000003475307118528 ) ) ;
#7497 = DIRECTION ( 'NONE',  ( -0.000000000000000000, 0.000000000000000000, 1.000000000000000000 ) ) ;
#7498 = CARTESIAN_POINT ( 'NONE',  ( -63.08758708074093136, 41.04287353446839148, 3.000000000000000000 ) ) ;
#7499 = CARTESIAN_POINT ( 'NONE',  ( 5.108737389288024566, -30.36564925015480654, 6.941203072598473689 ) ) ;
#7500 = DIRECTION ( 'NONE',  ( 0.000000000000000000, 0.000000000000000000, 1.000000000000000000 ) ) ;
#7501 = CARTESIAN_POINT ( 'NONE',  ( 5.751251297819365504, -26.64985754041175525, 6.700000000000000178 ) ) ;
#7502 = CARTESIAN_POINT ( 'NONE',  ( 5.094274781369510841, -29.77377858573793645, 6.920489980334481928 ) ) ;
#7503 = AXIS2_PLACEMENT_3D ( 'NONE', #4004, #35294, #32401 ) ;
#7504 = CARTESIAN_POINT ( 'NONE',  ( 0.3457495631895174948, -32.79715019981050972, 7.013842709614101167 ) ) ;
#7505 = CARTESIAN_POINT ( 'NONE',  ( 4.301450302647315205, -31.91148321001355370, 7.754798119455333705 ) ) ;
#7506 = ORIENTED_EDGE ( 'NONE', *, *, #29570, .F. ) ;
#7507 = CARTESIAN_POINT ( 'NONE',  ( 66.70283438698932343, 57.92520761901871396, 3.999543855873470388 ) ) ;
#7508 = CARTESIAN_POINT ( 'NONE',  ( 71.78591447743995957, 60.68937113591298527, -3.856543183828340826 ) ) ;
#7509 = CIRCLE ( 'NONE', #35800, 4.406751979251624540 ) ;
#7510 = CARTESIAN_POINT ( 'NONE',  ( 2.273382508532649116, -26.11715138113199686, 7.707984471951054850 ) ) ;
#7511 = CARTESIAN_POINT ( 'NONE',  ( 88.16134551068515179, -2.448791080374484341, 0.2153404935567143075 ) ) ;
#7512 = AXIS2_PLACEMENT_3D ( 'NONE', #11605, #20890, #20470 ) ;
#7513 = DIRECTION ( 'NONE',  ( 1.000000000000000000, -0.000000000000000000, 0.000000000000000000 ) ) ;
#7514 = CARTESIAN_POINT ( 'NONE',  ( -81.79890681550139675, 10.46299657128043314, 0.6911394749367771873 ) ) ;
#7515 = ADVANCED_FACE ( 'NONE', ( #36515 ), #23743, .F. ) ;
#7516 = PRODUCT_CONTEXT ( 'NONE', #33465, 'mechanical' ) ;
#7517 = FACE_OUTER_BOUND ( 'NONE', #14999, .T. ) ;
#7518 = CARTESIAN_POINT ( 'NONE',  ( -54.01549048184568846, -38.28842912540938670, 6.000000000000000000 ) ) ;
#7519 = EDGE_LOOP ( 'NONE', ( #6621, #23845, #13661, #8467 ) ) ;
#7520 = CARTESIAN_POINT ( 'NONE',  ( 5.200390093233090205, -29.78421258894830004, 7.376841543590331618 ) ) ;
#7521 = ORIENTED_EDGE ( 'NONE', *, *, #21855, .T. ) ;
#7522 = CARTESIAN_POINT ( 'NONE',  ( 78.75925357433533236, 65.51276736450270732, -2.660933152496149479 ) ) ;
#7523 = CARTESIAN_POINT ( 'NONE',  ( 37.14386006597155898, -2.493502119373617099, 5.967606418918435907 ) ) ;
#7524 = CARTESIAN_POINT ( 'NONE',  ( 80.87650043350870988, 61.69514696456048597, 2.603857329607122573 ) ) ;
#7525 = CARTESIAN_POINT ( 'NONE',  ( -1.294668884637889983, -31.17919483241161771, 6.864651958020304257 ) ) ;
#7526 = EDGE_CURVE ( 'NONE', #22132, #31681, #25093, .T. ) ;
#7527 = PRESENTATION_LAYER_ASSIGNMENT (  '', '', ( #31237 ) ) ;
#7528 = CIRCLE ( 'NONE', #10783, 0.1000000000000028644 ) ;
#7529 = CARTESIAN_POINT ( 'NONE',  ( 2.913833110970087681, -32.85284901314008010, 7.750000000000001776 ) ) ;
#7530 = CARTESIAN_POINT ( 'NONE',  ( 4.037545593495729612, -27.10057719777305962, 6.988553391373222290 ) ) ;
#7531 = PLANE ( 'NONE',  #5117 ) ;
#7532 = CARTESIAN_POINT ( 'NONE',  ( -70.92837670882107659, -37.87473357531881391, 0.000000000000000000 ) ) ;
#7533 = CARTESIAN_POINT ( 'NONE',  ( 21.71190961143752673, 6.329471954421165059, -3.192818159646633625 ) ) ;
#7534 = VERTEX_POINT ( 'NONE', #24152 ) ;
#7535 = DIRECTION ( 'NONE',  ( -0.9848077530122015810, -0.1736481776669674404, 0.000000000000000000 ) ) ;
#7536 = AXIS2_PLACEMENT_3D ( 'NONE', #38904, #4547, #17069 ) ;
#7537 = CARTESIAN_POINT ( 'NONE',  ( -1.763152082461436843, -30.07389502416336668, 6.863784140767622333 ) ) ;
#7538 = CARTESIAN_POINT ( 'NONE',  ( -0.5525555990343373747, -32.24114388472590775, 7.773839561854632763 ) ) ;
#7539 = CARTESIAN_POINT ( 'NONE',  ( -74.65853108593573495, -2.675584617184129765, -9.325032285645074026 ) ) ;
#7540 = EDGE_CURVE ( 'NONE', #12025, #12828, #8358, .T. ) ;
#7541 = DIRECTION ( 'NONE',  ( -0.000000000000000000, -0.000000000000000000, 1.000000000000000000 ) ) ;
#7542 = FACE_OUTER_BOUND ( 'NONE', #6060, .T. ) ;
#7543 = CARTESIAN_POINT ( 'NONE',  ( 80.28274408427736830, 64.63090917800610669, 3.500437194783546868 ) ) ;
#7544 = CARTESIAN_POINT ( 'NONE',  ( -70.92837670882107659, -23.80776546975053165, 0.000000000000000000 ) ) ;
#7545 = CYLINDRICAL_SURFACE ( 'NONE', #39766, 0.09010775117052929883 ) ;
#7546 = CARTESIAN_POINT ( 'NONE',  ( -40.34874870218063592, -25.49307895267003587, 6.700000000000000178 ) ) ;
#7547 = FACE_OUTER_BOUND ( 'NONE', #14020, .T. ) ;
#7548 = CARTESIAN_POINT ( 'NONE',  ( 4.487153213455422396, -27.45239593059636363, 7.013842709614101167 ) ) ;
#7549 = DIRECTION ( 'NONE',  ( 0.000000000000000000, 0.000000000000000000, -1.000000000000000000 ) ) ;
#7550 = CARTESIAN_POINT ( 'NONE',  ( 5.149536281657578485, -30.16439681061213918, 7.635761828346576685 ) ) ;
#7551 = DIRECTION ( 'NONE',  ( -0.000000000000000000, -0.000000000000000000, 1.000000000000000000 ) ) ;
#7552 = B_SPLINE_CURVE_WITH_KNOTS ( 'NONE', 3,
 ( #26493, #26887, #10623, #1391, #17392, #20099, #35770, #23784, #29973, #13922, #11017, #4477, #36363, #29575, #39018, #8130, #10822, #20701, #35963, #5065, #4665, #33284, #17598, #27090, #5266 ),
 .UNSPECIFIED., .F., .F.,
 ( 4, 3, 3, 3, 3, 3, 3, 3, 4 ),
 ( 6.468151674593380289E-05, 9.076621574722002080E-05, 0.0001210204262067981427, 0.0001512763324577423183, 0.0001815301820994218098, 0.0002117781465860724133, 0.0002420274594459777555, 0.0002722905548971147043, 0.0002816827545175574869 ),
 .UNSPECIFIED. ) ;
#7553 = CARTESIAN_POINT ( 'NONE',  ( 69.33847993643759366, 58.44820081139205570, 3.962610901733985447 ) ) ;
#7554 = CARTESIAN_POINT ( 'NONE',  ( 37.04382469011167700, -2.892849699906013150, 5.987982769814347073 ) ) ;
#7555 = EDGE_CURVE ( 'NONE', #25058, #9646, #40203, .T. ) ;
#7556 = AXIS2_PLACEMENT_3D ( 'NONE', #11274, #39288, #4720 ) ;
#7557 = LINE ( 'NONE', #30619, #4957 ) ;
#7558 = CARTESIAN_POINT ( 'NONE',  ( 84.79389884800966115, 3.063713526918731223, 0.3112276665278714827 ) ) ;
#7560 = DIRECTION ( 'NONE',  ( 0.4582725098355732163, -0.8888117386314183799, -1.924382947419148497E-16 ) ) ;
#7559 = CARTESIAN_POINT ( 'NONE',  ( 78.65660921518627902, 66.03460256502702919, -1.194943971655633375 ) ) ;
#7561 = VECTOR ( 'NONE', #16166, 1000.000000000000000 ) ;
#7562 = CARTESIAN_POINT ( 'NONE',  ( -1.292970362984873223, -27.75612332118079095, 6.867280401193707640 ) ) ;
#7563 = ORIENTED_EDGE ( 'NONE', *, *, #37581, .F. ) ;
#7564 = CARTESIAN_POINT ( 'NONE',  ( -80.67007510693973416, 11.48218648236320050, -2.296920554925718339 ) ) ;
#7565 = CARTESIAN_POINT ( 'NONE',  ( 21.78047190118184773, 5.616103730238553027, 3.473245441588607374 ) ) ;
#7566 = CIRCLE ( 'NONE', #37162, 0.1000000000000028644 ) ;
#7567 = ORIENTED_EDGE ( 'NONE', *, *, #24444, .F. ) ;
#7568 = CYLINDRICAL_SURFACE ( 'NONE', #22138, 0.09010775117052938210 ) ;
#7570 = ORIENTED_EDGE ( 'NONE', *, *, #11465, .T. ) ;
#7569 = VERTEX_POINT ( 'NONE', #15909 ) ;
#7571 = CARTESIAN_POINT ( 'NONE',  ( 78.61080321328475407, 66.00207709680658752, -1.298998371267914953 ) ) ;
#7572 = EDGE_CURVE ( 'NONE', #10043, #14380, #28058, .T. ) ;
#7573 = CARTESIAN_POINT ( 'NONE',  ( 25.01091298175105848, 3.329590532566609529, -1.936828115965013142 ) ) ;
#7574 = EDGE_CURVE ( 'NONE', #2073, #1149, #26272, .T. ) ;
#7575 = CARTESIAN_POINT ( 'NONE',  ( 81.12912465015324415, 61.32884242822650833, 1.592560325354579254 ) ) ;
#7576 = CARTESIAN_POINT ( 'NONE',  ( 21.77340129706707472, 1.030455091318688288, 7.426159514375072490 ) ) ;
#7577 = VERTEX_POINT ( 'NONE', #34065 ) ;
#7578 = ADVANCED_FACE ( 'NONE', ( #24565 ), #40608, .F. ) ;
#7579 = CARTESIAN_POINT ( 'NONE',  ( 0.02833428261566706824, -32.53037429976859585, 7.721096864323904185 ) ) ;
#7580 = CARTESIAN_POINT ( 'NONE',  ( 39.57450465021913999, -13.08403409140692553, 6.000000000000001776 ) ) ;
#7581 = LINE ( 'NONE', #10659, #1449 ) ;
#7582 = B_SPLINE_SURFACE_WITH_KNOTS ( 'NONE', 5, 3, ( 
 ( #25392, #1248, #13975, #26353, #38885, #12818, #14177, #29825, #10678, #7400, #23453, #19212, #26544, #10481, #16854, #4530, #15914 ),
 ( #36021, #4334, #32340, #23259, #13578, #35826, #28473, #26747, #32929, #17252, #4133, #20351, #9524, #22108, #7601, #17052, #7798 ),
 ( #1044, #4718, #1638, #32735, #34685, #19012, #29629, #31573, #1443, #19953, #39082, #37931, #280, #6660, #16648, #29236, #26151 ),
 ( #38684, #23061, #24043, #40106, #8183, #14992, #39690, #5325, #33746, #33131, #36411, #11886, #33550, #20755, #39903, #2052, #14774 ),
 ( #15192, #21384, #5734, #33346, #8800, #39286, #11074, #30441, #5525, #24459, #30237, #14565, #37017, #18274, #20969, #17860, #27139 ),
 ( #30866, #5122, #33960, #14371, #23644, #4913, #2251, #27550, #36211, #17655, #27345, #17444, #7990, #18069, #8600, #2673, #20547 ),
 ( #11677, #24254, #30034, #36817, #1849, #26941, #39483, #11272, #23835, #11478, #36612, #8396, #21178, #30658, #2468, #37221, #12308 ),
 ( #9012, #12928, #28159, #5940, #9217, #18478, #19309, #31065, #21591, #25293, #6145, #34785, #27750, #21796, #37828, #27954, #2875 ) ),
 .UNSPECIFIED., .F., .F., .F.,
 ( 6, 2, 6 ),
 ( 4, 1, 1, 1, 1, 1, 1, 1, 1, 1, 1, 1, 1, 1, 4 ),
 ( 0.000000000000000000, 0.5000000000000000000, 1.000000000000000000 ),
 ( 0.006307410990057117292, 0.008855845011544563258, 0.01161705605602081880, 0.01384754710661961243, 0.01682153517408467233, 0.01905202622468346596, 0.02091076876684912558, 0.02239776280058165467, 0.02351300832588105669, 0.02462825385118044830, 0.02555762512226328331, 0.02630112213912954092, 0.02685874490177924193, 0.02741636766442894294, 0.02797399042707864047 ),
 .UNSPECIFIED. ) ;
#7583 = DIRECTION ( 'NONE',  ( 1.000000000000000000, 0.000000000000000000, 0.000000000000000000 ) ) ;
#7584 = CARTESIAN_POINT ( 'NONE',  ( 21.79149120270722406, 5.488331395040956018, -3.526327173381369917 ) ) ;
#7585 = VERTEX_POINT ( 'NONE', #18791 ) ;
#7586 = CARTESIAN_POINT ( 'NONE',  ( 2.336689928817082151, -33.01160456067486848, 7.730015791551948290 ) ) ;
#7587 = AXIS2_PLACEMENT_3D ( 'NONE', #1633, #5323, #24456 ) ;
#7588 = CARTESIAN_POINT ( 'NONE',  ( 22.68001568621454567, -4.050230952900990111, -7.789969220879865652 ) ) ;
#7589 = AXIS2_PLACEMENT_3D ( 'NONE', #20820, #17511, #30927 ) ;
#7590 = CARTESIAN_POINT ( 'NONE',  ( 20.24823138111565868, 11.68787526792871567, -3.842642712661572979 ) ) ;
#7591 = CARTESIAN_POINT ( 'NONE',  ( 18.62546845537173823, 11.49410710365845034, 2.500000000000000444 ) ) ;
#7592 = EDGE_CURVE ( 'NONE', #26219, #21380, #27051, .T. ) ;
#7593 = ORIENTED_EDGE ( 'NONE', *, *, #36258, .T. ) ;
#7594 = DIRECTION ( 'NONE',  ( 0.8660254037844378194, 0.000000000000000000, -0.5000000000000015543 ) ) ;
#7595 = CARTESIAN_POINT ( 'NONE',  ( 80.65926296283299735, 64.83599339274636009, 3.316380171285409517 ) ) ;
#7596 = CARTESIAN_POINT ( 'NONE',  ( 88.31640312351544253, -1.506181138579067103, 3.771763452802144201 ) ) ;
#7597 = CARTESIAN_POINT ( 'NONE',  ( -0.4954141421830357550, -26.97407892422453202, 7.635761828346577573 ) ) ;
#7598 = ORIENTED_EDGE ( 'NONE', *, *, #23247, .F. ) ;
#7599 = CARTESIAN_POINT ( 'NONE',  ( 26.28491678605064052, -2.762637008470093303, 4.308794986214664391 ) ) ;
#7600 = DIRECTION ( 'NONE',  ( -1.000000000000000000, 0.000000000000000000, 0.000000000000000000 ) ) ;
#7601 = CARTESIAN_POINT ( 'NONE',  ( 14.65806710266428858, -5.610108328300923652, -2.494143896700089957 ) ) ;
#7602 = CARTESIAN_POINT ( 'NONE',  ( 35.33510954239903867, -3.168965055208807780, -5.721296445581753431 ) ) ;
#7603 = CARTESIAN_POINT ( 'NONE',  ( 2.428848143534461101, -33.77897949353074836, 7.635761828346577573 ) ) ;
#7604 = CARTESIAN_POINT ( 'NONE',  ( 84.10606912909534572, 3.010615857166643927, -0.2786395050580429689 ) ) ;
#7605 = CARTESIAN_POINT ( 'NONE',  ( 30.38040035538539385, -3.658749391580585986, -4.669445293200252145 ) ) ;
#7606 = DIRECTION ( 'NONE',  ( -0.000000000000000000, -1.000000000000000000, -0.000000000000000000 ) ) ;
#7607 = CARTESIAN_POINT ( 'NONE',  ( -26.44874870218064089, -26.64985754041175525, 6.700000000000000178 ) ) ;
#7608 = CARTESIAN_POINT ( 'NONE',  ( -1.133852526008121142, -27.69188090276239933, 6.969307238440509700 ) ) ;
#7609 = ORIENTED_EDGE ( 'NONE', *, *, #34523, .F. ) ;
#7610 = VERTEX_POINT ( 'NONE', #2770 ) ;
#7611 = CARTESIAN_POINT ( 'NONE',  ( 36.88815924642239708, -3.351591737224890899, 5.910525939546068308 ) ) ;
#7612 = B_SPLINE_CURVE_WITH_KNOTS ( 'NONE', 3,
 ( #4878, #30407, #21349, #27309, #11644, #36782, #8565, #9384, #25456, #28129 ),
 .UNSPECIFIED., .F., .F.,
 ( 4, 2, 2, 2, 4 ),
 ( 0.000000000000000000, 0.0003915841590506205440, 0.0007831683181012410880, 0.001174752477151861686, 0.001566336636202482176 ),
 .UNSPECIFIED. ) ;
#7613 = CARTESIAN_POINT ( 'NONE',  ( -0.5217032702065451666, -32.27405686018898479, 7.686927408461905920 ) ) ;
#7614 = CARTESIAN_POINT ( 'NONE',  ( 66.27376694609004915, 57.73522568913436004, -4.000000000000000000 ) ) ;
#7615 = EDGE_CURVE ( 'NONE', #4993, #32730, #11773, .T. ) ;
#7616 = CARTESIAN_POINT ( 'NONE',  ( 87.93119157070556469, -2.517311565827366593, -0.4176833736063458868 ) ) ;
#7617 = AXIS2_PLACEMENT_3D ( 'NONE', #39230, #7746, #17600 ) ;
#7618 = ORIENTED_EDGE ( 'NONE', *, *, #10630, .F. ) ;
#7619 = AXIS2_PLACEMENT_3D ( 'NONE', #21458, #15060, #18547 ) ;
#7620 = ADVANCED_FACE ( 'NONE', ( #11985 ), #25388, .F. ) ;
#7621 = CARTESIAN_POINT ( 'NONE',  ( 4.919815665899403889, -28.47658946930290469, 6.874555630061442990 ) ) ;
#7622 = CARTESIAN_POINT ( 'NONE',  ( -57.81912131869246707, 32.28080896713289860, -4.194423477175957871 ) ) ;
#7624 = CARTESIAN_POINT ( 'NONE',  ( 4.355968852827314386, -27.44672806176293278, 7.782034975670476307 ) ) ;
#7623 = DIRECTION ( 'NONE',  ( 0.8660254037844378194, 0.000000000000000000, -0.5000000000000015543 ) ) ;
#7625 = EDGE_LOOP ( 'NONE', ( #4741, #30511, #37381, #19273 ) ) ;
#7626 = CARTESIAN_POINT ( 'NONE',  ( 21.96632414918468257, 4.998869592191663713, 3.577591828290626275 ) ) ;
#7627 = VECTOR ( 'NONE', #19445, 1000.000000000000000 ) ;
#7628 = EDGE_CURVE ( 'NONE', #35289, #28513, #6041, .T. ) ;
#7629 = CARTESIAN_POINT ( 'NONE',  ( 82.47129118679410453, 63.86074534520101764, -1.718006205139864129 ) ) ;
#7630 = CARTESIAN_POINT ( 'NONE',  ( -1.317602929293604674, -31.34242190827973218, 7.737115613922529889 ) ) ;
#7631 = ORIENTED_EDGE ( 'NONE', *, *, #3895, .F. ) ;
#7633 = CARTESIAN_POINT ( 'NONE',  ( -28.87867591359218977, -26.64985754041175525, 6.700000000000000178 ) ) ;
#7632 = CARTESIAN_POINT ( 'NONE',  ( -1.600658481268679267, -28.40671124064021669, 7.695279973900954751 ) ) ;
#7634 = CARTESIAN_POINT ( 'NONE',  ( -69.92837670882107659, -0.7829914368874778541, 5.916079783099621459 ) ) ;
#7635 = CARTESIAN_POINT ( 'NONE',  ( 76.07689452438883393, 60.24265224227302440, 3.527522301306113661 ) ) ;
#7636 = CARTESIAN_POINT ( 'NONE',  ( 23.74466947080636103, 2.426168263719876261, -4.268781924364951408 ) ) ;
#7637 = EDGE_LOOP ( 'NONE', ( #24808, #1742, #36801, #29004 ) ) ;
#7638 = CARTESIAN_POINT ( 'NONE',  ( -17.07867591359219617, -26.64985754041175525, 6.700000000000000178 ) ) ;
#7639 = B_SPLINE_CURVE_WITH_KNOTS ( 'NONE', 3,
 ( #15345, #30816, #15139, #14718, #15555, #31216, #12038, #36970, #24828, #33697, #27901, #24413, #3037, #8550, #2823, #8749, #37372, #5682, #18019, #24616, #14938, #27698, #37171, #7796, #11626 ),
 .UNSPECIFIED., .F., .F.,
 ( 4, 3, 3, 3, 3, 3, 3, 3, 4 ),
 ( 6.468151674593702839E-05, 9.076621574722029185E-05, 0.0001210204262067993760, 0.0001512763324577439446, 0.0001815301820994234903, 0.0002117781465860706243, 0.0002420274594459773489, 0.0002722905548971168185, 0.0002816827545175608479 ),
 .UNSPECIFIED. ) ;
#7640 = CARTESIAN_POINT ( 'NONE',  ( 1.700390093233090871, -29.56993018339339940, 7.750000000000000888 ) ) ;
#7641 = CARTESIAN_POINT ( 'NONE',  ( -9.796229648729232409, -33.54387950140292673, 2.500000000000000000 ) ) ;
#7642 = CARTESIAN_POINT ( 'NONE',  ( 4.358291535071521672, -27.29274773012506827, 7.695279973900954751 ) ) ;
#7643 = CARTESIAN_POINT ( 'NONE',  ( 8.290806648384990041, -10.90558813203967148, 6.000000000000000000 ) ) ;
#7644 = CARTESIAN_POINT ( 'NONE',  ( 78.93443484242885688, 66.17773471521380202, 1.251938014746359240 ) ) ;
#7645 = CARTESIAN_POINT ( 'NONE',  ( 87.04213330793400871, 0.5878691963681530464, -4.891134986362597914 ) ) ;
#7646 = CARTESIAN_POINT ( 'NONE',  ( 31.36201648005763332, -1.233860125724708379, -5.969386505766030915 ) ) ;
#7647 = CARTESIAN_POINT ( 'NONE',  ( 2.403859601798915779, -26.24350106938568317, 7.761597726988851420 ) ) ;
#7648 = CARTESIAN_POINT ( 'NONE',  ( -1.017153196554518857, -27.35348519339999029, 7.255881584735165646 ) ) ;
#7649 = CARTESIAN_POINT ( 'NONE',  ( 4.668540769505296950, -31.42424039273510061, 7.754798119455333705 ) ) ;
#7650 = ORIENTED_EDGE ( 'NONE', *, *, #38567, .T. ) ;
#7651 = CARTESIAN_POINT ( 'NONE',  ( 0.7091610176047873360, -26.31761870563095584, 6.887945620086119547 ) ) ;
#7652 = CARTESIAN_POINT ( 'NONE',  ( 0.08572186079895513511, -26.46462327674753112, 6.880828092187099010 ) ) ;
#7653 = CARTESIAN_POINT ( 'NONE',  ( 33.65804166975612333, -1.144990435965010711, -5.459549444016131403 ) ) ;
#7654 = CARTESIAN_POINT ( 'NONE',  ( 1.145429890469515932, -32.92433313672930240, 7.695279973900954751 ) ) ;
#7655 = DIRECTION ( 'NONE',  ( -1.000000000000000000, 0.000000000000000000, 0.000000000000000000 ) ) ;
#7656 = CARTESIAN_POINT ( 'NONE',  ( -1.553762755224460390, -28.32229481116360148, 7.785593909369613819 ) ) ;
#7657 = AXIS2_PLACEMENT_3D ( 'NONE', #8432, #30484, #39121 ) ;
#7658 = EDGE_CURVE ( 'NONE', #13011, #26146, #9520, .T. ) ;
#7659 = CARTESIAN_POINT ( 'NONE',  ( -14.24874870218063450, -25.49307895267003587, 6.700000000000000178 ) ) ;
#7660 = CARTESIAN_POINT ( 'NONE',  ( 4.327092635631263562, -31.72873540009916837, 7.712764235869101093 ) ) ;
#7661 = ORIENTED_EDGE ( 'NONE', *, *, #34680, .F. ) ;
#7662 = CARTESIAN_POINT ( 'NONE',  ( 34.12202789009461412, -3.607432811949276896, 5.453396193817899196 ) ) ;
#7663 = FACE_OUTER_BOUND ( 'NONE', #35038, .T. ) ;
#7664 = CARTESIAN_POINT ( 'NONE',  ( 67.19584252064707641, 57.93747020029492489, -3.996350724342223604 ) ) ;
#7665 = CARTESIAN_POINT ( 'NONE',  ( 5.100363281305461349, -29.55642757665872722, 7.635761828346577573 ) ) ;
#7666 = ORIENTED_EDGE ( 'NONE', *, *, #13605, .F. ) ;
#7667 = LINE ( 'NONE', #4591, #39735 ) ;
#7668 = CARTESIAN_POINT ( 'NONE',  ( 86.43572624768425783, -0.5192074800720990480, -5.777013305174518720 ) ) ;
#7669 = CARTESIAN_POINT ( 'NONE',  ( -59.87552183813128437, 24.84364830758654108, 9.681005660250221467 ) ) ;
#7670 = CARTESIAN_POINT ( 'NONE',  ( 0.9405239856375441354, -32.88393131473412012, 6.882085323592684212 ) ) ;
#7671 = DIRECTION ( 'NONE',  ( -0.7055275666422152758, 0.2567910337120286601, -0.6605219282605402364 ) ) ;
#7672 = DIRECTION ( 'NONE',  ( -0.000000000000000000, -0.000000000000000000, -1.000000000000000000 ) ) ;
#7673 = EDGE_LOOP ( 'NONE', ( #2551, #26103, #29495, #25941 ) ) ;
#7674 = CARTESIAN_POINT ( 'NONE',  ( 24.39331214698706063, 3.157612729095597093, 3.298590225890907668 ) ) ;
#7675 = EDGE_CURVE ( 'NONE', #22775, #26905, #31568, .T. ) ;
#7676 = CARTESIAN_POINT ( 'NONE',  ( -70.92837670882107659, -47.11702805680359063, 38.00000000000000711 ) ) ;
#7677 = CARTESIAN_POINT ( 'NONE',  ( 81.18025391627377019, 61.34316975053406651, 1.531260274641954133 ) ) ;
#7678 = CIRCLE ( 'NONE', #12943, 4.500000000000003553 ) ;
#7679 = EDGE_CURVE ( 'NONE', #347, #29836, #23617, .T. ) ;
#7680 = CARTESIAN_POINT ( 'NONE',  ( 15.71855938504309158, -1.673920629206014921, -2.500000000000009770 ) ) ;
#7681 = ORIENTED_EDGE ( 'NONE', *, *, #6318, .F. ) ;
#7682 = CARTESIAN_POINT ( 'NONE',  ( 79.81867444595899030, 61.24600406626227311, -2.764360460937574260 ) ) ;
#7683 =( BOUNDED_SURFACE ( )  B_SPLINE_SURFACE ( 3, 2, ( 
 ( #24814, #37355, #39324 ),
 ( #1082, #32966, #23874 ),
 ( #33170, #1887, #23684 ),
 ( #4956, #32573, #20386 ),
 ( #14009, #4752, #1680 ),
 ( #26784, #26188, #19989 ) ),
 .UNSPECIFIED., .F., .F., .F. ) 
 B_SPLINE_SURFACE_WITH_KNOTS ( ( 4, 2, 4 ),
 ( 3, 3 ),
 ( 0.000000000000000000, 0.001067213068432975882, 0.002134426136865951763 ),
 ( 0.000000000000000000, 1.000000000000000000 ),
 .UNSPECIFIED. ) 
 GEOMETRIC_REPRESENTATION_ITEM ( )  RATIONAL_B_SPLINE_SURFACE ( (
 ( 1.000000000000000000, 0.6872206705710276475, 1.000000000000000000),
 ( 1.000000000000000000, 0.6752582546152587906, 1.000000000000000000),
 ( 1.000000000000000000, 0.6623616715682778544, 1.000000000000000000),
 ( 1.000000000000000000, 0.6342435107462536248, 1.000000000000000000),
 ( 1.000000000000000000, 0.6188407181625764641, 1.000000000000000000),
 ( 1.000000000000000000, 0.6029302108204156463, 1.000000000000000000) ) ) 
 REPRESENTATION_ITEM ( '' )  SURFACE ( )  );
#7685 = CARTESIAN_POINT ( 'NONE',  ( -1.656077431862442717, -30.11226380117775037, 6.894806418505347700 ) ) ;
#7684 = CARTESIAN_POINT ( 'NONE',  ( 24.12554661758536412, 0.5101533851207924464, 5.092830807977074770 ) ) ;
#7686 = AXIS2_PLACEMENT_3D ( 'NONE', #4544, #7213, #32352 ) ;
#7687 = CARTESIAN_POINT ( 'NONE',  ( 79.76387963405315418, 62.93107248426419176, 3.707164540951496168 ) ) ;
#7688 = AXIS2_PLACEMENT_3D ( 'NONE', #8541, #36553, #5261 ) ;
#7689 = AXIS2_PLACEMENT_3D ( 'NONE', #16316, #32392, #28886 ) ;
#7690 = DIRECTION ( 'NONE',  ( -0.000000000000000000, -1.000000000000000000, -0.000000000000000000 ) ) ;
#7691 = CARTESIAN_POINT ( 'NONE',  ( 81.04763707098177861, 66.10603528134694784, 1.133121492189030244 ) ) ;
#7692 = LINE ( 'NONE', #8078, #38661 ) ;
#7693 = CARTESIAN_POINT ( 'NONE',  ( 27.90799128822289177, 2.452171383980988661, -2.014541967423249424 ) ) ;
#7694 = CARTESIAN_POINT ( 'NONE',  ( -64.53809346645441281, 34.68836506924190388, -5.879071147244565587 ) ) ;
#7695 = ORIENTED_EDGE ( 'NONE', *, *, #13605, .T. ) ;
#7696 = CARTESIAN_POINT ( 'NONE',  ( -77.66794378176071234, -6.280236162145751422, 7.398505571724361296 ) ) ;
#7697 = CARTESIAN_POINT ( 'NONE',  ( 23.58963810436863184, 0.4214879312981080761, -5.525765152133263136 ) ) ;
#7698 = DIRECTION ( 'NONE',  ( -0.7660444431189813441, 0.6427876096865353661, -0.000000000000000000 ) ) ;
#7699 = ORIENTED_EDGE ( 'NONE', *, *, #25169, .F. ) ;
#7700 = CARTESIAN_POINT ( 'NONE',  ( -63.03213158086253287, 38.26878225442504800, 4.032857076801014351 ) ) ;
#7701 = CARTESIAN_POINT ( 'NONE',  ( 36.20057779688249866, -3.648500508209620907, -5.719125637313637434 ) ) ;
#7702 = CYLINDRICAL_SURFACE ( 'NONE', #24889, 0.09010775117052782779 ) ;
#7703 = CARTESIAN_POINT ( 'NONE',  ( 5.110065143779969787, -30.35994034135222464, 6.921725064902949143 ) ) ;
#7704 = FACE_OUTER_BOUND ( 'NONE', #26436, .T. ) ;
#7705 = CARTESIAN_POINT ( 'NONE',  ( -89.20959394718985891, -30.27593629695115496, 6.954324564059724878 ) ) ;
#7706 = CIRCLE ( 'NONE', #6426, 2.999999999999998668 ) ;
#7707 = CARTESIAN_POINT ( 'NONE',  ( 21.56351936394880653, 7.350594945348953857, 2.885250585115055166 ) ) ;
#7708 = CARTESIAN_POINT ( 'NONE',  ( 2.140324932704912975, -33.04217115098462898, 6.895394898881669121 ) ) ;
#7709 = VERTEX_POINT ( 'NONE', #34271 ) ;
#7710 =( GEOMETRIC_REPRESENTATION_CONTEXT ( 3 ) GLOBAL_UNCERTAINTY_ASSIGNED_CONTEXT ( ( #34143 ) ) GLOBAL_UNIT_ASSIGNED_CONTEXT ( ( #37895, #37681, #35048 ) ) REPRESENTATION_CONTEXT ( 'NONE', 'WORKASPACE' ) );
#7711 = CARTESIAN_POINT ( 'NONE',  ( 66.27376694608996388, 57.73522568913447373, 4.000000000000000000 ) ) ;
#7712 = AXIS2_PLACEMENT_3D ( 'NONE', #24148, #37114, #17961 ) ;
#7713 = CARTESIAN_POINT ( 'NONE',  ( 73.49116904989887189, 59.86802450872643533, -3.864208391251975350 ) ) ;
#7714 = VECTOR ( 'NONE', #8151, 1000.000000000000227 ) ;
#7715 = CARTESIAN_POINT ( 'NONE',  ( 87.52985346608603834, -1.683278932971326691, -4.201117388013917875 ) ) ;
#7716 = CARTESIAN_POINT ( 'NONE',  ( 23.06591706423118637, -8.086835649431872497, -2.500000000000005773 ) ) ;
#7717 = PLANE ( 'NONE',  #16267 ) ;
#7718 = LINE ( 'NONE', #26066, #20840 ) ;
#7719 = DIRECTION ( 'NONE',  ( 1.000000000000000000, 0.000000000000000000, 0.000000000000000000 ) ) ;
#7720 = DIRECTION ( 'NONE',  ( 0.000000000000000000, 1.000000000000000000, 0.000000000000000000 ) ) ;
#7721 = CYLINDRICAL_SURFACE ( 'NONE', #33152, 0.1000000000000028644 ) ;
#7722 = EDGE_CURVE ( 'NONE', #32500, #30676, #24574, .T. ) ;
#7723 = CARTESIAN_POINT ( 'NONE',  ( 5.054776957217135269, -30.12498762792620255, 7.691066658568944447 ) ) ;
#7724 = ORIENTED_EDGE ( 'NONE', *, *, #29155, .F. ) ;
#7725 = EDGE_CURVE ( 'NONE', #5658, #40275, #17045, .T. ) ;
#7726 = ORIENTED_EDGE ( 'NONE', *, *, #31680, .F. ) ;
#7727 = CARTESIAN_POINT ( 'NONE',  ( 80.03393078220564405, 63.38059744715224042, -3.720735635808767761 ) ) ;
#7728 = CARTESIAN_POINT ( 'NONE',  ( 33.79019614278077199, -4.865436059503933208, 3.423093293932546022 ) ) ;
#7729 = CARTESIAN_POINT ( 'NONE',  ( 78.56188500726534585, 65.90376500477509580, 1.760837461004421733 ) ) ;
#7730 = CARTESIAN_POINT ( 'NONE',  ( 6.053772676492744864, -27.07209504432901070, 7.635761828346577573 ) ) ;
#7731 = AXIS2_PLACEMENT_3D ( 'NONE', #12305, #40101, #24879 ) ;
#7732 = DIRECTION ( 'NONE',  ( -1.000000000000000000, 0.000000000000000000, 0.000000000000000000 ) ) ;
#7733 = CARTESIAN_POINT ( 'NONE',  ( 3.934882339056233302, -27.00729354443371477, 6.880147297696980857 ) ) ;
#7734 = DIRECTION ( 'NONE',  ( -0.000000000000000000, -0.000000000000000000, 1.000000000000000000 ) ) ;
#7735 = CARTESIAN_POINT ( 'NONE',  ( 21.85643539959774273, 8.980655621775115449, -3.220279653634019468 ) ) ;
#7736 = CARTESIAN_POINT ( 'NONE',  ( 23.43555436076258047, 3.792607145904837829, -3.105262516303788800 ) ) ;
#7737 = ORIENTED_EDGE ( 'NONE', *, *, #15538, .T. ) ;
#7738 = CARTESIAN_POINT ( 'NONE',  ( -1.312560436656866392, -31.35097737660188244, 7.695279973900954751 ) ) ;
#7739 = DIRECTION ( 'NONE',  ( 1.000000000000000000, 0.000000000000000000, 0.000000000000000000 ) ) ;
#7740 = CARTESIAN_POINT ( 'NONE',  ( -74.03255566204833826, -1.800923653458333273, -9.560995967708043608 ) ) ;
#7741 = CARTESIAN_POINT ( 'NONE',  ( -0.03016364352379581268, -26.64329662474590066, 7.680992449362114449 ) ) ;
#7742 = CARTESIAN_POINT ( 'NONE',  ( -24.44874870218064089, -25.49307895267003587, 6.700000000000000178 ) ) ;
#7743 = CARTESIAN_POINT ( 'NONE',  ( 79.02829278184948691, 65.95432764922182400, 2.098997056523008276 ) ) ;
#7744 = LINE ( 'NONE', #38829, #36722 ) ;
#7745 = DIRECTION ( 'NONE',  ( 1.000000000000000000, 0.000000000000000000, 0.000000000000000000 ) ) ;
#7746 = DIRECTION ( 'NONE',  ( -1.000000000000000000, 0.000000000000000000, 0.000000000000000000 ) ) ;
#7747 = DIRECTION ( 'NONE',  ( 0.1736481776669127897, 0.9848077530122111289, 0.000000000000000000 ) ) ;
#7748 = CARTESIAN_POINT ( 'NONE',  ( -70.31483849620295246, 0.01762406564628603983, 9.981599438687137393 ) ) ;
#7749 = EDGE_CURVE ( 'NONE', #40076, #30228, #10124, .T. ) ;
#7750 = CARTESIAN_POINT ( 'NONE',  ( 4.466905112401445166, -27.42599002650289819, 6.870724624169669781 ) ) ;
#7751 = DIRECTION ( 'NONE',  ( 0.000000000000000000, 0.000000000000000000, 1.000000000000000000 ) ) ;
#7752 = PLANE ( 'NONE',  #22838 ) ;
#7753 = DIRECTION ( 'NONE',  ( 1.000000000000000000, 0.000000000000000000, 0.000000000000000000 ) ) ;
#7754 = AXIS2_PLACEMENT_3D ( 'NONE', #37603, #3277, #37202 ) ;
#7755 = CARTESIAN_POINT ( 'NONE',  ( 67.75953150630846267, 58.21208410194267202, 3.997018227265523027 ) ) ;
#7756 = CARTESIAN_POINT ( 'NONE',  ( 34.13608517534122910, -3.137549310921635470, 5.534159694588579370 ) ) ;
#7757 = ADVANCED_FACE ( 'NONE', ( #488 ), #22313, .F. ) ;
#7758 = CARTESIAN_POINT ( 'NONE',  ( -64.08758708074094557, 42.86724024650072096, -2.417504074514746026 ) ) ;
#7759 = CARTESIAN_POINT ( 'NONE',  ( 86.31714526353648864, 1.402210177843808081, 5.108895447378689170 ) ) ;
#7761 = CARTESIAN_POINT ( 'NONE',  ( -0.4043138943918587747, -26.77346281303682218, 6.989977667959440311 ) ) ;
#7760 = CARTESIAN_POINT ( 'NONE',  ( 80.26353224374044260, 64.23390916343181800, -3.625945587094181022 ) ) ;
#7762 = CARTESIAN_POINT ( 'NONE',  ( -1.233457003589831347, -27.66138591813160019, 6.921725064902950919 ) ) ;
#7763 = CARTESIAN_POINT ( 'NONE',  ( -58.91620474891572456, 27.52990360452330876, 4.138963871842780584 ) ) ;
#7764 = ORIENTED_EDGE ( 'NONE', *, *, #34848, .T. ) ;
#7765 = CARTESIAN_POINT ( 'NONE',  ( -80.88140849387957587, 11.46041792646347268, -1.055489314687744207 ) ) ;
#7766 = DIRECTION ( 'NONE',  ( 0.000000000000000000, -0.000000000000000000, 1.000000000000000000 ) ) ;
#7767 = AXIS2_PLACEMENT_3D ( 'NONE', #2617, #40052, #15341 ) ;
#7768 = EDGE_LOOP ( 'NONE', ( #1, #39472, #12966, #30977 ) ) ;
#7769 = CARTESIAN_POINT ( 'NONE',  ( -71.78177034180626492, -21.31587262608876543, 3.939402591579943547 ) ) ;
#7770 = EDGE_CURVE ( 'NONE', #22883, #10139, #16311, .T. ) ;
#7771 = ORIENTED_EDGE ( 'NONE', *, *, #29780, .T. ) ;
#7772 = CARTESIAN_POINT ( 'NONE',  ( 80.99395165659464624, 61.72087377645419082, -2.545842637937974828 ) ) ;
#7773 = DIRECTION ( 'NONE',  ( -0.000000000000000000, -0.000000000000000000, -1.000000000000000000 ) ) ;
#7774 = CARTESIAN_POINT ( 'NONE',  ( 81.11594168931695492, 61.32525408782629484, 1.607835478472323221 ) ) ;
#7775 = CARTESIAN_POINT ( 'NONE',  ( 27.06702955060504578, 1.340722218708290114, 4.422313656526443815 ) ) ;
#7777 = ORIENTED_EDGE ( 'NONE', *, *, #17403, .F. ) ;
#7776 = CARTESIAN_POINT ( 'NONE',  ( -0.7662878407683642035, -27.22994832146974176, 6.979335674598006634 ) ) ;
#7778 = CARTESIAN_POINT ( 'NONE',  ( -0.04300629806284254203, -32.48894888815854642, 7.785868773668302545 ) ) ;
#7780 = CARTESIAN_POINT ( 'NONE',  ( -39.07867591359219261, -26.64985754041175525, 6.700000000000000178 ) ) ;
#7779 = CARTESIAN_POINT ( 'NONE',  ( 14.69558838330753936, 10.99631180437154399, 5.999999999999998224 ) ) ;
#7781 = FACE_OUTER_BOUND ( 'NONE', #24645, .T. ) ;
#7782 = CARTESIAN_POINT ( 'NONE',  ( -63.43903122600000444, 42.92536711289877616, -3.490931750529367772 ) ) ;
#7783 = CARTESIAN_POINT ( 'NONE',  ( -34.44874870218064444, -26.64985754041175525, 6.700000000000000178 ) ) ;
#7784 = CARTESIAN_POINT ( 'NONE',  ( 22.26302464024987060, 4.951729634934853408, -3.260511412105697282 ) ) ;
#7785 = VERTEX_POINT ( 'NONE', #10528 ) ;
#7786 = CARTESIAN_POINT ( 'NONE',  ( -83.92837670882109080, 2.429809908903242999, -12.50000000000000000 ) ) ;
#7787 = CARTESIAN_POINT ( 'NONE',  ( 22.42980438978510449, 1.271109115893125585, 8.904229291692644210 ) ) ;
#7788 = CARTESIAN_POINT ( 'NONE',  ( 16.28258120957830712, 10.03625422200891570, 2.499999999999521272 ) ) ;
#7789 = DIRECTION ( 'NONE',  ( 0.000000000000000000, 0.000000000000000000, 1.000000000000000000 ) ) ;
#7790 = CARTESIAN_POINT ( 'NONE',  ( 81.00465555257858341, 64.24153452434767075, 3.375310687858767977 ) ) ;
#7791 = CARTESIAN_POINT ( 'NONE',  ( 86.69422455818764206, -0.1941184515037400471, -5.886102099071623073 ) ) ;
#7792 = DIRECTION ( 'NONE',  ( 0.000000000000000000, 0.000000000000000000, -1.000000000000000000 ) ) ;
#7793 = ORIENTED_EDGE ( 'NONE', *, *, #37643, .T. ) ;
#7794 = EDGE_CURVE ( 'NONE', #18315, #24999, #7447, .T. ) ;
#7795 = ORIENTED_EDGE ( 'NONE', *, *, #2280, .F. ) ;
#7796 = CARTESIAN_POINT ( 'NONE',  ( 5.067448495235368888, -29.09778390448199659, 7.757178535559534183 ) ) ;
#7797 = CARTESIAN_POINT ( 'NONE',  ( 4.381563664431031846, -27.47916279290977570, 7.754798119455333705 ) ) ;
#7798 = CARTESIAN_POINT ( 'NONE',  ( 14.83377924836928763, -6.137502382583376992, -2.521568026651588301 ) ) ;
#7799 = CARTESIAN_POINT ( 'NONE',  ( 36.44628851498989519, -2.355918992659408406, -5.894722798219696358 ) ) ;
#7800 = CARTESIAN_POINT ( 'NONE',  ( -70.92837670882107659, 13.87661300689599386, 0.000000000000000000 ) ) ;
#7801 = CARTESIAN_POINT ( 'NONE',  ( 84.11566709744786863, 2.998976903239075842, -0.6299403505785813318 ) ) ;
#7802 = ADVANCED_FACE ( 'NONE', ( #16906 ), #38325, .F. ) ;
#7803 = CARTESIAN_POINT ( 'NONE',  ( 30.05768800033484567, -3.720313780293153183, -4.561934355542292430 ) ) ;
#7804 = ORIENTED_EDGE ( 'NONE', *, *, #28965, .F. ) ;
#7805 = CARTESIAN_POINT ( 'NONE',  ( -1.675359094926574866, -29.97529103330290212, 7.013842709614101167 ) ) ;
#7806 = ADVANCED_FACE ( 'NONE', ( #19614 ), #16505, .T. ) ;
#7807 = LINE ( 'NONE', #16654, #15199 ) ;
#7808 = CARTESIAN_POINT ( 'NONE',  ( -1.133226946762783793, -27.69093715879794360, 6.949473656533220023 ) ) ;
#7809 = AXIS2_PLACEMENT_3D ( 'NONE', #7232, #20184, #9916 ) ;
#7810 = ORIENTED_EDGE ( 'NONE', *, *, #12864, .T. ) ;
#7811 = ORIENTED_EDGE ( 'NONE', *, *, #24794, .T. ) ;
#7812 = CARTESIAN_POINT ( 'NONE',  ( 23.38580533471466438, 3.559992555223038924, 3.092799683450411230 ) ) ;
#7813 = CARTESIAN_POINT ( 'NONE',  ( -0.5217032702065468319, -32.27405686018897768, 7.695279973900954751 ) ) ;
#7814 = CARTESIAN_POINT ( 'NONE',  ( 33.45208957067621469, -3.251134754649326553, 5.427405637984302089 ) ) ;
#7815 = CARTESIAN_POINT ( 'NONE',  ( -32.44874870218063734, -26.64985754041175525, 6.800000000000000711 ) ) ;
#7816 = ORIENTED_EDGE ( 'NONE', *, *, #38021, .F. ) ;
#7817 = DIRECTION ( 'NONE',  ( 1.000000000000000000, 0.000000000000000000, 0.000000000000000000 ) ) ;
#7818 = EDGE_CURVE ( 'NONE', #18445, #30749, #6423, .T. ) ;
#7819 = SHAPE_REPRESENTATION_RELATIONSHIP ( 'NONE' , 'NONE' ,  #23772, #21063 ) ;
#7820 = ORIENTED_EDGE ( 'NONE', *, *, #1697, .F. ) ;
#7821 = CARTESIAN_POINT ( 'NONE',  ( -55.97227462678459631, 30.94442605972648508, -3.900682954687262782 ) ) ;
#7823 = DIRECTION ( 'NONE',  ( -0.000000000000000000, -0.000000000000000000, -1.000000000000000000 ) ) ;
#7822 = CARTESIAN_POINT ( 'NONE',  ( 4.817771186832979780, -27.97871391774301486, 6.998987538705432776 ) ) ;
#7824 = ORIENTED_EDGE ( 'NONE', *, *, #30559, .F. ) ;
#7825 = CARTESIAN_POINT ( 'NONE',  ( 24.54631049625050565, 2.974125097758586911, 3.602083437275587219 ) ) ;
#7826 = CARTESIAN_POINT ( 'NONE',  ( 81.75239774439246787, 65.41456323740523260, -1.882325606869287959 ) ) ;
#7827 = FACE_OUTER_BOUND ( 'NONE', #38939, .T. ) ;
#7828 = CARTESIAN_POINT ( 'NONE',  ( -24.44874870218064089, -26.64985754041175525, 6.800000000000000711 ) ) ;
#7829 = ORIENTED_EDGE ( 'NONE', *, *, #28970, .T. ) ;
#7830 = B_SPLINE_CURVE_WITH_KNOTS ( 'NONE', 3,
 ( #19963, #26948, #10688, #23844, #36220, #7608, #23655, #7808, #20161, #26555, #8000, #32747, #20762, #39494, #33356, #4537, #5130, #13982, #29835, #20556, #39091, #10887, #14185, #36030, #20359, #4727, #17662, #24262, #14783, #5536, #24465 ),
 .UNSPECIFIED., .F., .F.,
 ( 4, 3, 3, 3, 3, 3, 3, 3, 3, 3, 4 ),
 ( 1.852685484479510593E-18, 2.999644130997501231E-05, 6.002588995694337391E-05, 8.960886084587722073E-05, 0.0001190604700446470872, 0.0001489538463052668957, 0.0001796139255493938976, 0.0002109707048517038531, 0.0002426195318110337031, 0.0002740640997890010340, 0.0002849778069099823054 ),
 .UNSPECIFIED. ) ;
#7832 = CARTESIAN_POINT ( 'NONE',  ( 1.096693473209699121, -26.22395493079927320, 7.635761828346577573 ) ) ;
#7831 = CARTESIAN_POINT ( 'NONE',  ( 0.1332591166277097561, -0.5999999999999993117, -3.927378378441396922 ) ) ;
#7833 = CARTESIAN_POINT ( 'NONE',  ( 21.58930880649559469, 5.738281464677914556, -3.444703897471878218 ) ) ;
#7834 = CARTESIAN_POINT ( 'NONE',  ( 76.86947707741242652, 60.02096306738859255, 3.097219288968718676 ) ) ;
#7835 = CARTESIAN_POINT ( 'NONE',  ( 22.94681503686735979, 2.560486077929890136, -4.549303765806815392 ) ) ;
#7836 = LINE ( 'NONE', #14813, #21779 ) ;
#7837 = EDGE_CURVE ( 'NONE', #17583, #13035, #16112, .T. ) ;
#7838 = DIRECTION ( 'NONE',  ( -1.000000000000000000, 0.000000000000000000, 0.000000000000000000 ) ) ;
#7839 = AXIS2_PLACEMENT_3D ( 'NONE', #1426, #29807, #33112 ) ;
#7840 = CARTESIAN_POINT ( 'NONE',  ( 5.053206214525213902, -25.63013845337225405, 7.695279973900954751 ) ) ;
#7841 = LINE ( 'NONE', #20797, #608 ) ;
#7842 = CARTESIAN_POINT ( 'NONE',  ( -64.92837670882106238, 13.87661300689593880, 0.000000000000000000 ) ) ;
#7843 = CARTESIAN_POINT ( 'NONE',  ( 79.43434746088968268, 66.19712225821035645, 1.744953761006671433 ) ) ;
#7844 = CARTESIAN_POINT ( 'NONE',  ( 86.36291470068610465, 1.350799773688788674, 4.987004148466622766 ) ) ;
#7845 = CARTESIAN_POINT ( 'NONE',  ( 31.00707005056823817, -0.8718966892480422004, 5.891928739871540088 ) ) ;
#7846 = PLANE ( 'NONE',  #34616 ) ;
#7847 = CARTESIAN_POINT ( 'NONE',  ( -81.79890681550139675, 10.46299657128043314, 0.6911394749367771873 ) ) ;
#7848 = CARTESIAN_POINT ( 'NONE',  ( -72.99860296447080543, 0.8259586708074142525, -10.94618862030606898 ) ) ;
#7849 = DIRECTION ( 'NONE',  ( -0.000000000000000000, -0.000000000000000000, 1.000000000000000000 ) ) ;
#7850 = CARTESIAN_POINT ( 'NONE',  ( -0.001601940877974058304, -26.51162622272786606, 6.875671892026061549 ) ) ;
#7851 = CARTESIAN_POINT ( 'NONE',  ( 36.24028759768958707, -2.130151203274132765, -5.862571372923810031 ) ) ;
#7852 = FACE_OUTER_BOUND ( 'NONE', #38071, .T. ) ;
#7853 = CARTESIAN_POINT ( 'NONE',  ( -1.699583094839331787, -29.58343279012807159, 7.635761828346577573 ) ) ;
#7854 = ADVANCED_FACE ( 'NONE', ( #34881 ), #19205, .T. ) ;
#7855 = CARTESIAN_POINT ( 'NONE',  ( -1.550429272321787622, -28.30655406119563722, 7.782861076432732617 ) ) ;
#7856 = ADVANCED_FACE ( 'NONE', ( #20599 ), #17104, .F. ) ;
#7857 = AXIS2_PLACEMENT_3D ( 'NONE', #33183, #23305, #23696 ) ;
#7858 = DIRECTION ( 'NONE',  ( -0.000000000000000000, 1.000000000000000000, -0.000000000000000000 ) ) ;
#7859 = EDGE_CURVE ( 'NONE', #18940, #26569, #19692, .T. ) ;
#7860 = VERTEX_POINT ( 'NONE', #24094 ) ;
#7861 = CARTESIAN_POINT ( 'NONE',  ( 37.05414849786873788, -3.059465710589756249, 5.984234486237220985 ) ) ;
#7862 = CYLINDRICAL_SURFACE ( 'NONE', #33041, 0.1000000000000028644 ) ;
#7863 = ADVANCED_FACE ( 'NONE', ( #20402 ), #30496, .F. ) ;
#7864 = CARTESIAN_POINT ( 'NONE',  ( 67.17215761800675011, 58.00255761909972563, -3.998533043703387690 ) ) ;
#7865 = CARTESIAN_POINT ( 'NONE',  ( 4.716523069940627089, -27.79427549280784149, 7.660770905198780234 ) ) ;
#7866 = EDGE_LOOP ( 'NONE', ( #9943, #193, #30943, #22848 ) ) ;
#7867 = CARTESIAN_POINT ( 'NONE',  ( -2.448748702180640446, -25.49307895267003587, 6.700000000000000178 ) ) ;
#7868 = CIRCLE ( 'NONE', #34858, 0.1000000000000028644 ) ;
#7869 = DIRECTION ( 'NONE',  ( -0.000000000000000000, -0.000000000000000000, 1.000000000000000000 ) ) ;
#7870 = CARTESIAN_POINT ( 'NONE',  ( -59.89982099243564306, 24.84364830758654463, 9.562162450795216984 ) ) ;
#7871 = CARTESIAN_POINT ( 'NONE',  ( 0.9202033279314624226, -32.87921311799081536, 7.006423389747790331 ) ) ;
#7872 = ADVANCED_FACE ( 'NONE', ( #30285 ), #13129, .T. ) ;
#7873 = CARTESIAN_POINT ( 'NONE',  ( 0.3560817122006099678, -32.80147640128887332, 6.883550009118462931 ) ) ;
#7874 = CARTESIAN_POINT ( 'NONE',  ( -69.32837670882108227, -34.30579396504363388, 1.870248747537495149E-15 ) ) ;
#7875 = VERTEX_POINT ( 'NONE', #14616 ) ;
#7876 = CARTESIAN_POINT ( 'NONE',  ( -1.740039500620327972, -30.21292645845072400, 7.700536657684220465 ) ) ;
#7877 = CARTESIAN_POINT ( 'NONE',  ( 80.89892670780336914, 62.72941125082672187, 3.340002271463668571 ) ) ;
#7878 = FACE_OUTER_BOUND ( 'NONE', #25909, .T. ) ;
#7879 = VERTEX_POINT ( 'NONE', #33402 ) ;
#7880 = CARTESIAN_POINT ( 'NONE',  ( 78.21991615976335765, 63.09003589986988914, -3.816136337383043031 ) ) ;
#7882 = CARTESIAN_POINT ( 'NONE',  ( -1.729658636700265983, -28.87367900006760735, 6.864746396199586265 ) ) ;
#7881 = CARTESIAN_POINT ( 'NONE',  ( 24.74497300857456850, 0.5733567267288544045, 4.778227254168478488 ) ) ;
#7883 = CARTESIAN_POINT ( 'NONE',  ( 81.47197553453537466, 61.72158698297718615, -1.969816429101936439 ) ) ;
#7884 = CARTESIAN_POINT ( 'NONE',  ( -26.34874870218063947, -26.64985754041175525, 6.800000000000000711 ) ) ;
#7885 = CARTESIAN_POINT ( 'NONE',  ( 80.13677637144074595, 61.33843513727117625, 2.660685394430964745 ) ) ;
#7886 = AXIS2_PLACEMENT_3D ( 'NONE', #40186, #34045, #37100 ) ;
#7887 = CARTESIAN_POINT ( 'NONE',  ( 37.17969408807407916, -3.008184067405535345, -5.999999779455217563 ) ) ;
#7888 = CARTESIAN_POINT ( 'NONE',  ( 82.01097102582275511, 65.15803335478938152, 1.775718711109096404 ) ) ;
#7889 = CARTESIAN_POINT ( 'NONE',  ( 14.69558838330753758, 3.996311804371543985, 6.000000000000000000 ) ) ;
#7890 = CARTESIAN_POINT ( 'NONE',  ( 26.56638717734885802, 2.990222579127657099, 1.122734419917069237 ) ) ;
#7891 = CARTESIAN_POINT ( 'NONE',  ( -62.87442376950072287, 35.57781650258913686, -5.904453864323630619 ) ) ;
#7892 = VERTEX_POINT ( 'NONE', #23888 ) ;
#7893 = CARTESIAN_POINT ( 'NONE',  ( -28.44874870218064444, -26.64985754041175525, 6.700000000000000178 ) ) ;
#7894 = CARTESIAN_POINT ( 'NONE',  ( 24.12519416928313731, 0.5064133828745956967, -5.093109222506538636 ) ) ;
#7895 = EDGE_CURVE ( 'NONE', #38802, #34099, #1692, .T. ) ;
#7896 = DIRECTION ( 'NONE',  ( 0.000000000000000000, 0.000000000000000000, 1.000000000000000000 ) ) ;
#7897 = DIRECTION ( 'NONE',  ( 0.000000000000000000, 0.000000000000000000, 1.000000000000000000 ) ) ;
#7898 = EDGE_CURVE ( 'NONE', #3715, #8480, #21655, .T. ) ;
#7899 = VECTOR ( 'NONE', #37749, 1000.000000000000000 ) ;
#7900 = VERTEX_POINT ( 'NONE', #20805 ) ;
#7901 = CARTESIAN_POINT ( 'NONE',  ( 37.00777520336294657, -3.244670941504010919, -5.947354996402821392 ) ) ;
#7902 = FACE_OUTER_BOUND ( 'NONE', #32845, .T. ) ;
#7903 = CARTESIAN_POINT ( 'NONE',  ( 3.283585891740897544, -32.69138896436592034, 6.931070083220553180 ) ) ;
#7904 = CARTESIAN_POINT ( 'NONE',  ( 5.113812245512664667, -30.34358980514384285, 7.013842709614101167 ) ) ;
#7905 = CARTESIAN_POINT ( 'NONE',  ( 6.173121028034443292, -31.06824956420287975, 7.754798119455333705 ) ) ;
#7906 = CARTESIAN_POINT ( 'NONE',  ( -69.92837670882107659, -23.80776546975053520, 9.949874371066204759 ) ) ;
#7907 = ADVANCED_FACE ( 'NONE', ( #5174 ), #8040, .F. ) ;
#7908 = CARTESIAN_POINT ( 'NONE',  ( 1.888561142012757044, -26.07499217873563779, 6.980586498568967180 ) ) ;
#7909 = EDGE_CURVE ( 'NONE', #14684, #20444, #39749, .T. ) ;
#7910 = VERTEX_POINT ( 'NONE', #15241 ) ;
#7911 = CARTESIAN_POINT ( 'NONE',  ( 66.27376694608996388, 57.73522568913447373, 4.000000000000000000 ) ) ;
#7912 = CARTESIAN_POINT ( 'NONE',  ( 71.29558780583862188, 58.60460498947428931, -3.808711916423244581 ) ) ;
#7913 = VECTOR ( 'NONE', #37773, 1000.000000000000000 ) ;
#7914 = ORIENTED_EDGE ( 'NONE', *, *, #11645, .T. ) ;
#7915 = CARTESIAN_POINT ( 'NONE',  ( 86.43572624768424362, -0.5192074800720991590, -5.777013305174518720 ) ) ;
#7916 = CARTESIAN_POINT ( 'NONE',  ( -81.80090188080514224, -5.603160304130404334, -0.6545554231109831367 ) ) ;
#7917 =( BOUNDED_CURVE ( )  B_SPLINE_CURVE ( 3, ( #14237, #35888, #7060, #7665 ),
 .UNSPECIFIED., .F., .T. ) 
 B_SPLINE_CURVE_WITH_KNOTS ( ( 4, 4 ),
 ( 1.381924640371167579, 1.574767692156076260 ),
 .UNSPECIFIED. ) 
 CURVE ( )  GEOMETRIC_REPRESENTATION_ITEM ( )  RATIONAL_B_SPLINE_CURVE ( ( 1.000000000000000000, 0.9969033633783032089, 0.9969033633783032089, 1.000000000000000000 ) ) 
 REPRESENTATION_ITEM ( '' )  );
#7918 = LINE ( 'NONE', #21302, #14937 ) ;
#7919 = SHAPE_DEFINITION_REPRESENTATION ( #12565, #32460 ) ;
#7920 = CARTESIAN_POINT ( 'NONE',  ( 1.751251297819361730, -26.64985754041175525, 6.700000000000000178 ) ) ;
#7921 = DIRECTION ( 'NONE',  ( -0.000000000000000000, -0.000000000000000000, -1.000000000000000000 ) ) ;
#7922 = CARTESIAN_POINT ( 'NONE',  ( -1.752498985642892304, -28.99760421947164701, 7.695279973900954751 ) ) ;
#7923 = VECTOR ( 'NONE', #11994, 1000.000000000000000 ) ;
#7924 = EDGE_LOOP ( 'NONE', ( #37577, #27002, #28454, #16920 ) ) ;
#7925 = CARTESIAN_POINT ( 'NONE',  ( 80.17375466371954928, 63.09909492358892180, -3.665158340976944817 ) ) ;
#7926 = CARTESIAN_POINT ( 'NONE',  ( 5.166053052204034657, -29.08252373668924307, 7.754798119455333705 ) ) ;
#7927 = CARTESIAN_POINT ( 'NONE',  ( 79.26327435592847337, 64.69753611046425590, 3.458772244351174585 ) ) ;
#7928 = CARTESIAN_POINT ( 'NONE',  ( 0.5073350864888854783, -26.38612432390972273, 7.721096864323905073 ) ) ;
#7929 = CARTESIAN_POINT ( 'NONE',  ( -26.44874870218064089, -26.64985754041175525, 6.700000000000000178 ) ) ;
#7930 = CARTESIAN_POINT ( 'NONE',  ( 4.038094055326753029, -27.10109490474136607, 6.920489980334480151 ) ) ;
#7931 = CYLINDRICAL_SURFACE ( 'NONE', #20241, 0.1000000000000028644 ) ;
#7932 = CARTESIAN_POINT ( 'NONE',  ( 21.85643539959776760, 10.44946649885084966, 7.640826779728119078 ) ) ;
#7933 = ORIENTED_EDGE ( 'NONE', *, *, #12366, .F. ) ;
#7934 = CARTESIAN_POINT ( 'NONE',  ( 73.32739823182221528, 62.33856649896100777, -3.356242416136164142 ) ) ;
#7935 = CIRCLE ( 'NONE', #28972, 2.500000000000002220 ) ;
#7936 = CARTESIAN_POINT ( 'NONE',  ( 14.61802060940782155, -4.492733667522514907, 2.499999999999997780 ) ) ;
#7937 = CARTESIAN_POINT ( 'NONE',  ( -77.10359778981232637, 9.587385728467753054, -7.883471332551708066 ) ) ;
#7938 = CARTESIAN_POINT ( 'NONE',  ( -0.3565594025764889374, -32.28597026120641544, 7.139196562012274150 ) ) ;
#7939 = CARTESIAN_POINT ( 'NONE',  ( -4.266520354791871306, -48.67644278316300444, -6.000000000000000000 ) ) ;
#7940 = CARTESIAN_POINT ( 'NONE',  ( 81.15583125883576088, 62.51952284974313301, 3.108243619504618138 ) ) ;
#7941 = LINE ( 'NONE', #23198, #25539 ) ;
#7942 = CARTESIAN_POINT ( 'NONE',  ( 3.369155479471896530, -26.60763004909045293, 7.695279973900954751 ) ) ;
#7943 = DIRECTION ( 'NONE',  ( 0.000000000000000000, 0.000000000000000000, 1.000000000000000000 ) ) ;
#7944 = CARTESIAN_POINT ( 'NONE',  ( 0.6797214339997408317, -26.22205989199040133, 6.921725064902949143 ) ) ;
#7945 = EDGE_CURVE ( 'NONE', #16154, #32844, #15232, .T. ) ;
#7946 = EDGE_CURVE ( 'NONE', #6604, #21608, #21639, .T. ) ;
#7947 = CARTESIAN_POINT ( 'NONE',  ( 3.977533665642330352, -32.22786493825372389, 7.698786668945015954 ) ) ;
#7948 = LINE ( 'NONE', #30183, #2924 ) ;
#7949 = EDGE_CURVE ( 'NONE', #22149, #393, #24947, .T. ) ;
#7950 = CARTESIAN_POINT ( 'NONE',  ( 4.202471298688592150, -31.87203467081731745, 6.871394612369937427 ) ) ;
#7951 = B_SPLINE_CURVE_WITH_KNOTS ( 'NONE', 3,
 ( #15799, #9399, #15590, #5924, #21986, #34767, #163, #37806, #18463, #6739 ),
 .UNSPECIFIED., .F., .F.,
 ( 4, 2, 2, 2, 4 ),
 ( 0.001564566806966613413, 0.001955354412007498724, 0.002346142017048383818, 0.002736929622089268911, 0.003127717227130154005 ),
 .UNSPECIFIED. ) ;
#7952 = CARTESIAN_POINT ( 'NONE',  ( 67.89958468297673733, 58.72729936788584837, 3.969942683317638110 ) ) ;
#7953 = CARTESIAN_POINT ( 'NONE',  ( 36.78962651020381713, -3.042574519117287490, 5.948308996033500939 ) ) ;
#7954 = CARTESIAN_POINT ( 'NONE',  ( 2.278721782424116160, -33.01050799907499567, 7.781480525794717273 ) ) ;
#7955 = CARTESIAN_POINT ( 'NONE',  ( 87.78348876263190448, -0.2448564372010923473, 4.525229423219702340 ) ) ;
#7957 = DIRECTION ( 'NONE',  ( -0.9267318687906764829, 0.3757233601570978965, 0.000000000000000000 ) ) ;
#7956 = CARTESIAN_POINT ( 'NONE',  ( 79.75420125634298074, 65.05222905597021565, -3.324099845469145276 ) ) ;
#7958 = B_SPLINE_CURVE_WITH_KNOTS ( 'NONE', 3,
 ( #33972, #2885, #15406, #2263, #24055, #14788, #19117, #6768, #12727, #19526, #25500, #22014, #13330, #25702, #11034, #29592, #4291, #20506, #29992 ),
 .UNSPECIFIED., .F., .F.,
 ( 4, 3, 3, 3, 3, 3, 4 ),
 ( 8.940560153363745023E-19, 2.546128104244470004E-05, 5.711050680484456503E-05, 8.113074941676400118E-05, 0.0001053129305727060346, 0.0001360598016347115799, 0.0001612931755713786319 ),
 .UNSPECIFIED. ) ;
#7959 = CARTESIAN_POINT ( 'NONE',  ( -1.605123960799514249, -28.77395478264728723, 6.959317978105167057 ) ) ;
#7960 = CARTESIAN_POINT ( 'NONE',  ( -59.14838763364235064, 27.28340689960987575, 4.628958989307227156 ) ) ;
#7961 = ORIENTED_EDGE ( 'NONE', *, *, #11418, .F. ) ;
#7962 = CARTESIAN_POINT ( 'NONE',  ( -61.24591834330252027, -49.47158280949359010, -2.500000000000000000 ) ) ;
#7963 = VERTEX_POINT ( 'NONE', #8650 ) ;
#7964 = CARTESIAN_POINT ( 'NONE',  ( -0.5359795030213230227, -32.26226207767182785, 7.750000000000001776 ) ) ;
#7965 = CARTESIAN_POINT ( 'NONE',  ( 79.25227124789766719, 65.35518565838725635, -2.996423812020331479 ) ) ;
#7966 = CARTESIAN_POINT ( 'NONE',  ( 24.91734749558309758, 3.524439253337528832, -0.6529367285399855225 ) ) ;
#7967 = CARTESIAN_POINT ( 'NONE',  ( 80.23783879855322709, 63.84144632218769999, 3.668443954219270609 ) ) ;
#7968 = CARTESIAN_POINT ( 'NONE',  ( 25.84367263793748393, 1.600840454158463322, 4.297283297516126588 ) ) ;
#7970 = EDGE_LOOP ( 'NONE', ( #19165, #8346, #10889, #5275 ) ) ;
#7969 = CARTESIAN_POINT ( 'NONE',  ( 4.737757460784507657, -27.85713558299313064, 7.783750581861600182 ) ) ;
#7971 = CIRCLE ( 'NONE', #36265, 6.329987104167475565 ) ;
#7972 = CARTESIAN_POINT ( 'NONE',  ( 3.344239474442606941, -32.54613940854532217, 6.880147297696980857 ) ) ;
#7974 = DIRECTION ( 'NONE',  ( -0.000000000000000000, -0.000000000000000000, 1.000000000000000000 ) ) ;
#7973 = CARTESIAN_POINT ( 'NONE',  ( -37.07867591359219261, -26.64985754041175525, 6.800000000000000711 ) ) ;
#7975 = DIRECTION ( 'NONE',  ( 0.7126435865141255155, 0.000000000000000000, -0.7015262779114437297 ) ) ;
#7976 = CARTESIAN_POINT ( 'NONE',  ( 24.46786998095842591, 2.964482678099346291, -3.659345439263766764 ) ) ;
#7977 = ORIENTED_EDGE ( 'NONE', *, *, #29022, .T. ) ;
#7978 = CARTESIAN_POINT ( 'NONE',  ( 2.343386368290429012, -33.01035977724681914, 7.700536657684215136 ) ) ;
#7979 = ORIENTED_EDGE ( 'NONE', *, *, #3163, .T. ) ;
#7980 = CARTESIAN_POINT ( 'NONE',  ( 21.85643539959774273, 9.214175136349357587, -0.8338435668127727185 ) ) ;
#7981 = CARTESIAN_POINT ( 'NONE',  ( 16.14085267862078510, 12.58767977203877741, 2.500000000000000444 ) ) ;
#7982 = CARTESIAN_POINT ( 'NONE',  ( -38.87867591359218977, -26.64985754041175525, 6.700000000000000178 ) ) ;
#7983 = CARTESIAN_POINT ( 'NONE',  ( 81.56578493134864516, 62.15373153752177871, 2.499697124809907578 ) ) ;
#7984 = CARTESIAN_POINT ( 'NONE',  ( 84.35358620389857265, 3.041238144818853684, 1.123552906098365112 ) ) ;
#7985 = CYLINDRICAL_SURFACE ( 'NONE', #23972, 5.950000000000010836 ) ;
#7986 = VERTEX_POINT ( 'NONE', #24512 ) ;
#7987 = CARTESIAN_POINT ( 'NONE',  ( 3.598499603178781037, -24.87029584672219329, 6.954324564059724878 ) ) ;
#7988 = EDGE_LOOP ( 'NONE', ( #39774, #40644, #14063, #11904 ) ) ;
#7989 = LINE ( 'NONE', #27749, #35511 ) ;
#7990 = CARTESIAN_POINT ( 'NONE',  ( 14.83986818923396456, -4.481383445363374740, -2.516351727591476184 ) ) ;
#7991 = EDGE_CURVE ( 'NONE', #8630, #15393, #17185, .T. ) ;
#7992 = CARTESIAN_POINT ( 'NONE',  ( 34.77305545370109030, -3.160087570433653514, -5.633574311711002203 ) ) ;
#7993 = CARTESIAN_POINT ( 'NONE',  ( -39.07867591359219261, -24.55319635012989110, 6.700000000000000178 ) ) ;
#7994 = CARTESIAN_POINT ( 'NONE',  ( 25.26334528616294151, 0.8481682192316492008, -4.614059732833895033 ) ) ;
#7995 = CARTESIAN_POINT ( 'NONE',  ( 29.71865375326818537, -3.785866092356776402, -4.452099570374444149 ) ) ;
#7996 = ORIENTED_EDGE ( 'NONE', *, *, #33635, .T. ) ;
#7997 = CARTESIAN_POINT ( 'NONE',  ( 36.14140113770966423, -3.140483868442980775, 5.847137749265862716 ) ) ;
#7998 = CARTESIAN_POINT ( 'NONE',  ( -1.641525177248355227, -30.19571155489859393, 7.695279973900954751 ) ) ;
#7999 = AXIS2_PLACEMENT_3D ( 'NONE', #19936, #35415, #13766 ) ;
#8000 = CARTESIAN_POINT ( 'NONE',  ( -1.136876063035818785, -27.69644994437396690, 6.920489980334479263 ) ) ;
#8001 = ORIENTED_EDGE ( 'NONE', *, *, #480, .F. ) ;
#8002 = ORIENTED_EDGE ( 'NONE', *, *, #25950, .T. ) ;
#8003 = CARTESIAN_POINT ( 'NONE',  ( 21.73971162413815250, 4.236108717388963996, 2.798398138428574100 ) ) ;
#8004 = DIRECTION ( 'NONE',  ( -0.000000000000000000, -1.000000000000000000, -0.000000000000000000 ) ) ;
#8005 = CARTESIAN_POINT ( 'NONE',  ( 66.27376694609004915, 57.73522568913436004, -4.000000000000000000 ) ) ;
#8006 = AXIS2_PLACEMENT_3D ( 'NONE', #24944, #37477, #24523 ) ;
#8007 = DIRECTION ( 'NONE',  ( 1.000000000000000000, 0.000000000000000000, 0.000000000000000000 ) ) ;
#8008 = ORIENTED_EDGE ( 'NONE', *, *, #22195, .F. ) ;
#8009 = DIRECTION ( 'NONE',  ( -1.000000000000000000, 0.000000000000000000, 0.000000000000000000 ) ) ;
#8010 = VERTEX_POINT ( 'NONE', #18117 ) ;
#8011 = ORIENTED_EDGE ( 'NONE', *, *, #20725, .T. ) ;
#8012 = CARTESIAN_POINT ( 'NONE',  ( -58.25352014915284826, 31.25337030895682133, -4.614317915849918350 ) ) ;
#8013 = EDGE_LOOP ( 'NONE', ( #39260, #22502, #40043, #10733 ) ) ;
#8014 = EDGE_CURVE ( 'NONE', #21404, #21657, #21285, .T. ) ;
#8015 = B_SPLINE_CURVE_WITH_KNOTS ( 'NONE', 3,
 ( #3810, #19832, #38952, #35498, #20027, #7469, #35697, #16327, #13854, #4010 ),
 .UNSPECIFIED., .F., .F.,
 ( 4, 3, 3, 4 ),
 ( 0.0002170292169044733984, 0.0002420761345915937069, 0.0002723302478206994981, 0.0002816811360866810837 ),
 .UNSPECIFIED. ) ;
#8016 = CARTESIAN_POINT ( 'NONE',  ( 5.200390093233090205, -29.56993018339339940, 7.202408869016171167 ) ) ;
#8017 = VERTEX_POINT ( 'NONE', #24933 ) ;
#8018 = CARTESIAN_POINT ( 'NONE',  ( 22.75783442990022820, 3.925414047687008523, 3.607444980655814870 ) ) ;
#8019 = CARTESIAN_POINT ( 'NONE',  ( 80.71833143474471228, 65.93084270547788606, -2.217414436011610146 ) ) ;
#8020 = CARTESIAN_POINT ( 'NONE',  ( -1.229291416742352983, -31.29531890774162761, 7.661510568013100375 ) ) ;
#8021 = EDGE_LOOP ( 'NONE', ( #35000, #22591, #6071, #33571, #12427 ) ) ;
#8022 = CARTESIAN_POINT ( 'NONE',  ( 18.11164821838002581, -2.856713029497280232, -3.033158754982376859 ) ) ;
#8023 = CARTESIAN_POINT ( 'NONE',  ( -1.797707963539134868, -29.45456127420909453, 6.865482280155369210 ) ) ;
#8024 = CARTESIAN_POINT ( 'NONE',  ( 75.68633765818296411, 59.56198246982955169, 3.184487947857407963 ) ) ;
#8025 = CARTESIAN_POINT ( 'NONE',  ( 23.12551116169677812, 2.829306214856787349, -4.256801911362003921 ) ) ;
#8026 = LINE ( 'NONE', #39119, #31334 ) ;
#8027 = EDGE_CURVE ( 'NONE', #15998, #6497, #27600, .T. ) ;
#8028 = DIRECTION ( 'NONE',  ( -3.491481338843133750E-15, 1.000000000000000000, -0.000000000000000000 ) ) ;
#8029 = CARTESIAN_POINT ( 'NONE',  ( 2.255350295996689347, -26.21552723005750352, 7.695279973900954751 ) ) ;
#8030 = CARTESIAN_POINT ( 'NONE',  ( 0.5083189215969784458, -0.5999999999999994227, -3.960569937088305181 ) ) ;
#8031 = PLANE ( 'NONE',  #16870 ) ;
#8032 = CARTESIAN_POINT ( 'NONE',  ( 81.56984355495256978, 61.60674381500906804, 1.524764441711115248 ) ) ;
#8033 = CARTESIAN_POINT ( 'NONE',  ( 86.17935586795600500, 1.556981766839054426, 4.792924669753763744 ) ) ;
#8034 = CARTESIAN_POINT ( 'NONE',  ( 33.81722006525239266, -4.984950771528167124, -3.153948780582495726 ) ) ;
#8035 = DIRECTION ( 'NONE',  ( -0.000000000000000000, -0.000000000000000000, 1.000000000000000000 ) ) ;
#8036 = CARTESIAN_POINT ( 'NONE',  ( 2.455443087130759761, -25.36557027936252950, 7.635761828346577573 ) ) ;
#8037 = AXIS2_PLACEMENT_3D ( 'NONE', #19020, #15919, #4190 ) ;
#8038 = CARTESIAN_POINT ( 'NONE',  ( -1.666363480296579214, -25.64183336440431660, 7.695279973900954751 ) ) ;
#8039 = CARTESIAN_POINT ( 'NONE',  ( 0.6070493791425947139, -26.35050461072708217, 6.874555630061442102 ) ) ;
#8040 = CYLINDRICAL_SURFACE ( 'NONE', #32195, 0.09010775117053089478 ) ;
#8041 = EDGE_CURVE ( 'NONE', #31820, #32857, #9866, .T. ) ;
#8042 = CARTESIAN_POINT ( 'NONE',  ( 36.43203232075673270, -3.203092416211517524, -5.892497774322134951 ) ) ;
#8043 = LINE ( 'NONE', #14425, #1635 ) ;
#8044 = CARTESIAN_POINT ( 'NONE',  ( 5.913132016808740232, -27.35729686493488444, 6.894806418505347700 ) ) ;
#8045 = FACE_OUTER_BOUND ( 'NONE', #21369, .T. ) ;
#8046 = CARTESIAN_POINT ( 'NONE',  ( -63.03213158086148837, 38.26878225442760595, -4.032857076800604901 ) ) ;
#8047 = VERTEX_POINT ( 'NONE', #30709 ) ;
#8048 = CARTESIAN_POINT ( 'NONE',  ( 35.81810683760681968, -3.623504837237730314, 5.691522942300115240 ) ) ;
#8049 = FACE_OUTER_BOUND ( 'NONE', #12714, .T. ) ;
#8050 = CARTESIAN_POINT ( 'NONE',  ( 67.71971274774827521, 58.31971506597766819, -3.997018227265501267 ) ) ;
#8051 = EDGE_CURVE ( 'NONE', #25629, #408, #21227, .T. ) ;
#8052 = CARTESIAN_POINT ( 'NONE',  ( -0.6423071664414388149, -32.17016755036935649, 7.753200566781599967 ) ) ;
#8053 = ORIENTED_EDGE ( 'NONE', *, *, #38697, .T. ) ;
#8054 = CARTESIAN_POINT ( 'NONE',  ( -0.5081950327262328981, -32.15491601341089734, 7.782167645815903256 ) ) ;
#8055 = CARTESIAN_POINT ( 'NONE',  ( 2.041952719453895781, -26.17999055166718847, 7.505001789837626447 ) ) ;
#8056 = CARTESIAN_POINT ( 'NONE',  ( 86.00134810727946899, 0.2530519298808260320, -5.999722280616810899 ) ) ;
#8057 = CARTESIAN_POINT ( 'NONE',  ( -78.38494362056192699, 11.33516465962242670, 6.676281561881168614 ) ) ;
#8058 = CARTESIAN_POINT ( 'NONE',  ( 3.325856478880445000, -25.14347697372913615, 7.635761828346577573 ) ) ;
#8059 = AXIS2_PLACEMENT_3D ( 'NONE', #37949, #28283, #6679 ) ;
#8060 = CARTESIAN_POINT ( 'NONE',  ( 3.375652116166204753, -26.60313850063288754, 7.257242401810563237 ) ) ;
#8061 = ORIENTED_EDGE ( 'NONE', *, *, #10630, .T. ) ;
#8062 = CARTESIAN_POINT ( 'NONE',  ( 22.19016211074803380, 5.251790732463271105, 3.087872149380293418 ) ) ;
#8063 = CARTESIAN_POINT ( 'NONE',  ( 82.45631153319118312, 62.87735296625317005, -1.118100487915077546 ) ) ;
#8064 = CARTESIAN_POINT ( 'NONE',  ( 80.54296318544949429, 63.62250603730376497, 3.633989118465184465 ) ) ;
#8065 = DIRECTION ( 'NONE',  ( -0.000000000000000000, -0.000000000000000000, 1.000000000000000000 ) ) ;
#8066 = ORIENTED_EDGE ( 'NONE', *, *, #20621, .F. ) ;
#8067 = CARTESIAN_POINT ( 'NONE',  ( 78.86847112531718551, 61.76850681771003337, -3.535928464255535530 ) ) ;
#8069 = CARTESIAN_POINT ( 'NONE',  ( -42.34874870218063592, -25.49307895267003587, 6.700000000000000178 ) ) ;
#8068 = CARTESIAN_POINT ( 'NONE',  ( 21.97297751200100535, 0.2232358743075266438, 7.728093094151400777 ) ) ;
#8070 = EDGE_CURVE ( 'NONE', #9413, #8271, #34961, .T. ) ;
#8071 = EDGE_CURVE ( 'NONE', #38621, #25777, #23119, .T. ) ;
#8072 = CARTESIAN_POINT ( 'NONE',  ( 81.56787793379467644, 61.92707632880870960, -2.226826180274436240 ) ) ;
#8073 = CARTESIAN_POINT ( 'NONE',  ( 79.93789898034924590, 60.96822905336945553, 2.313798345564227255 ) ) ;
#8074 = EDGE_CURVE ( 'NONE', #1010, #8622, #31565, .T. ) ;
#8075 = LINE ( 'NONE', #21064, #16182 ) ;
#8076 = CARTESIAN_POINT ( 'NONE',  ( 82.31572251369559012, 62.52525979466052064, 1.394285451509447382 ) ) ;
#8078 = CARTESIAN_POINT ( 'NONE',  ( 0.9453370993353911178, -33.77429008742427641, 7.635761828346577573 ) ) ;
#8077 = CARTESIAN_POINT ( 'NONE',  ( 3.372445903850545879, -26.60948606701822072, 7.721096864323912179 ) ) ;
#8079 = CARTESIAN_POINT ( 'NONE',  ( 26.62075075102985267, 2.678422205045695392, 2.704210781993271695 ) ) ;
#8080 = VERTEX_POINT ( 'NONE', #17228 ) ;
#8081 = DIRECTION ( 'NONE',  ( 0.000000000000000000, 0.000000000000000000, 1.000000000000000000 ) ) ;
#8082 = CARTESIAN_POINT ( 'NONE',  ( 23.05347533656128078, 0.3447057208869356293, -5.959858412725844268 ) ) ;
#8083 = CARTESIAN_POINT ( 'NONE',  ( -1.798246035484871941, -29.45711074671229213, 7.076385936538748922 ) ) ;
#8084 = CYLINDRICAL_SURFACE ( 'NONE', #20438, 34.02204673211314656 ) ;
#8085 = CARTESIAN_POINT ( 'NONE',  ( 5.173998118306290195, -29.14088312892098998, 6.998987538705437217 ) ) ;
#8086 = CARTESIAN_POINT ( 'NONE',  ( -18.97867591359219475, -24.55319635012989110, 6.700000000000000178 ) ) ;
#8087 = CARTESIAN_POINT ( 'NONE',  ( 29.48679710191445480, 1.217383870121761857, -4.226918706498755007 ) ) ;
#8088 = CARTESIAN_POINT ( 'NONE',  ( 3.353162068531330586, -32.65217298741799112, 7.766640943994647550 ) ) ;
#8089 = CARTESIAN_POINT ( 'NONE',  ( 3.291606358883502725, -32.68731127699327033, 6.998987538705430111 ) ) ;
#8090 = CARTESIAN_POINT ( 'NONE',  ( 5.123175978192011648, -30.30112382633142332, 6.867199677474202346 ) ) ;
#8091 = CARTESIAN_POINT ( 'NONE',  ( 4.994613704055145043, -30.75234092066372682, 7.638132480492516585 ) ) ;
#8092 = CARTESIAN_POINT ( 'NONE',  ( 2.784495919998266622, -32.79246250384788652, 6.870716933885665512 ) ) ;
#8093 = CARTESIAN_POINT ( 'NONE',  ( 5.095188070987068940, -29.75802495820000360, 6.895222827070025318 ) ) ;
#8094 = CIRCLE ( 'NONE', #38982, 0.1000000000000028644 ) ;
#8095 = CARTESIAN_POINT ( 'NONE',  ( 1.854699838584355609, -26.07332139947373406, 6.880828092187096345 ) ) ;
#8096 = ORIENTED_EDGE ( 'NONE', *, *, #11088, .T. ) ;
#8097 = CARTESIAN_POINT ( 'NONE',  ( -18.24874870218063450, -26.64985754041175525, 6.700000000000000178 ) ) ;
#8098 = CARTESIAN_POINT ( 'NONE',  ( 73.43932658456094487, 59.98824119151031198, -3.894134109119617992 ) ) ;
#8099 = AXIS2_PLACEMENT_3D ( 'NONE', #37717, #11782, #21084 ) ;
#8100 = ORIENTED_EDGE ( 'NONE', *, *, #8860, .T. ) ;
#8101 = CARTESIAN_POINT ( 'NONE',  ( -1.261910041069868260, -27.90116479715461750, 7.695279973900954751 ) ) ;
#8102 = DIRECTION ( 'NONE',  ( 0.000000000000000000, -0.5555716052200797561, -0.8314686954258614371 ) ) ;
#8103 = DIRECTION ( 'NONE',  ( -0.000000000000000000, 1.000000000000000000, -0.000000000000000000 ) ) ;
#8104 = CARTESIAN_POINT ( 'NONE',  ( -54.01549048184568846, -30.38627270959228710, -4.152976064860135708 ) ) ;
#8105 = EDGE_CURVE ( 'NONE', #34705, #6990, #32880, .T. ) ;
#8106 = FACE_OUTER_BOUND ( 'NONE', #2892, .T. ) ;
#8107 = DIRECTION ( 'NONE',  ( 1.000000000000000000, 0.000000000000000000, 0.000000000000000000 ) ) ;
#8108 = CARTESIAN_POINT ( 'NONE',  ( 5.054338971983688644, -30.12764086567874244, 7.670860738520327793 ) ) ;
#8109 = ADVANCED_FACE ( 'NONE', ( #11050 ), #17835, .F. ) ;
#8110 = ORIENTED_EDGE ( 'NONE', *, *, #25965, .T. ) ;
#8111 = CARTESIAN_POINT ( 'NONE',  ( 80.07543224467224263, 63.05907417235837187, -3.676305632669316203 ) ) ;
#8112 = CARTESIAN_POINT ( 'NONE',  ( 17.82514639985922855, 11.84176496571321202, -2.500000000000005773 ) ) ;
#8113 = CARTESIAN_POINT ( 'NONE',  ( 80.17375466371993298, 63.09909492358909944, 3.665158340976903517 ) ) ;
#8114 = CARTESIAN_POINT ( 'NONE',  ( 0.6222788575979638637, -26.34538739974215815, 7.778050822775631978 ) ) ;
#8115 = EDGE_CURVE ( 'NONE', #7900, #34397, #2660, .T. ) ;
#8116 = DIRECTION ( 'NONE',  ( 0.9396926207859126468, -0.3420201433256568890, -0.000000000000000000 ) ) ;
#8117 = CARTESIAN_POINT ( 'NONE',  ( 0.9267304714826871681, -32.98335233567298275, 7.013842709614101167 ) ) ;
#8118 = CARTESIAN_POINT ( 'NONE',  ( 18.33573041183021957, 13.40081273568012676, 2.499999999999999556 ) ) ;
#8119 = CARTESIAN_POINT ( 'NONE',  ( 21.85643539959779602, 5.813509198596546135, -11.62788251339591206 ) ) ;
#8120 = VERTEX_POINT ( 'NONE', #26722 ) ;
#8121 = CARTESIAN_POINT ( 'NONE',  ( -76.85200812145377824, 9.438718831883464944, 8.072108724517537581 ) ) ;
#8122 = B_SPLINE_CURVE_WITH_KNOTS ( 'NONE', 3,
 ( #5351, #13997, #14801, #17889, #11706, #29854, #30470, #1665, #32761, #23671, #4942, #36237, #17470, #2277, #36438, #30062, #24283, #7624, #31089, #5960, #8624, #24695, #8826, #37639, #28393 ),
 .UNSPECIFIED., .F., .F.,
 ( 4, 3, 3, 3, 3, 3, 3, 3, 4 ),
 ( 6.468151674593574090E-05, 9.076621574722103724E-05, 0.0001210204262067975870, 0.0001512763324577450831, 0.0001815301820994219724, 0.0002117781465860735517, 0.0002420274594459779723, 0.0002722905548971180111, 0.0002816827545175614985 ),
 .UNSPECIFIED. ) ;
#8123 = CARTESIAN_POINT ( 'NONE',  ( 14.62957350336051299, -4.708282797761865979, 2.500000000000223377 ) ) ;
#8124 = AXIS2_PLACEMENT_3D ( 'NONE', #30782, #11593, #15108 ) ;
#8125 = VECTOR ( 'NONE', #22758, 1000.000000000000000 ) ;
#8126 = CARTESIAN_POINT ( 'NONE',  ( -78.25485146663302771, 11.30612734474080305, -6.818008430746309578 ) ) ;
#8127 = CARTESIAN_POINT ( 'NONE',  ( 14.61802081865033820, 12.33286846116140190, 2.500000000000000000 ) ) ;
#8128 = CARTESIAN_POINT ( 'NONE',  ( 2.489749636244892095, -26.26283001680391394, 6.988553391373222290 ) ) ;
#8129 = CARTESIAN_POINT ( 'NONE',  ( 79.92139222979440660, 65.15389119341904234, 3.261148789966884287 ) ) ;
#8130 = CARTESIAN_POINT ( 'NONE',  ( -1.514709952630465484, -30.67588302826887414, 7.785172627573962778 ) ) ;
#8131 = LINE ( 'NONE', #20702, #16745 ) ;
#8132 = CARTESIAN_POINT ( 'NONE',  ( -71.92837670882106238, -42.87473357531881391, 1.732050807568877637 ) ) ;
#8133 = CARTESIAN_POINT ( 'NONE',  ( 31.50273333289666766, -0.4788391926020078571, 5.123161451720045001 ) ) ;
#8134 = VECTOR ( 'NONE', #4592, 1000.000000000000000 ) ;
#8135 = CARTESIAN_POINT ( 'NONE',  ( 4.487471559492266060, -27.45281495260537952, 6.895394898881672674 ) ) ;
#8136 = CARTESIAN_POINT ( 'NONE',  ( 87.88065579682655937, -0.3539990618341573025, 3.436608579331488666 ) ) ;
#8137 = CARTESIAN_POINT ( 'NONE',  ( 4.167068027234559047, -31.90991204531703929, 6.979335674598008410 ) ) ;
#8138 = ORIENTED_EDGE ( 'NONE', *, *, #37421, .F. ) ;
#8139 =( BOUNDED_CURVE ( )  B_SPLINE_CURVE ( 3, ( #30184, #11024, #39646, #4484 ),
 .UNSPECIFIED., .F., .T. ) 
 B_SPLINE_CURVE_WITH_KNOTS ( ( 4, 4 ),
 ( 1.347909859412853351, 1.534781240595298302 ),
 .UNSPECIFIED. ) 
 CURVE ( )  GEOMETRIC_REPRESENTATION_ITEM ( )  RATIONAL_B_SPLINE_CURVE ( ( 1.000000000000000000, 0.9970920404276226723, 0.9970920404276226723, 1.000000000000000000 ) ) 
 REPRESENTATION_ITEM ( '' )  );
#8140 = CARTESIAN_POINT ( 'NONE',  ( 68.17490759376208587, 57.99096015551094041, 3.964697573200901548 ) ) ;
#8141 = CARTESIAN_POINT ( 'NONE',  ( 37.06191389059799945, -2.795325952453375784, 5.990806027039132786 ) ) ;
#8142 = ORIENTED_EDGE ( 'NONE', *, *, #36261, .F. ) ;
#8143 = CARTESIAN_POINT ( 'NONE',  ( 2.254972451256867849, -33.01089166153567334, 7.785344483711591934 ) ) ;
#8144 = CARTESIAN_POINT ( 'NONE',  ( 88.05979627311084812, -0.5552181473167765446, -3.927858985986737661 ) ) ;
#8146 = PLANE ( 'NONE',  #32315 ) ;
#8145 = CARTESIAN_POINT ( 'NONE',  ( 79.09180288389933366, 65.81009211479097587, -2.442092683901130545 ) ) ;
#8147 = DIRECTION ( 'NONE',  ( 0.000000000000000000, 0.000000000000000000, 1.000000000000000000 ) ) ;
#8148 = CARTESIAN_POINT ( 'NONE',  ( -58.12241481891157235, 28.59128022406730096, 4.921134609696964368 ) ) ;
#8149 = CARTESIAN_POINT ( 'NONE',  ( -0.6791847275073886747, -32.13656744003537824, 7.009310105710484073 ) ) ;
#8150 = ORIENTED_EDGE ( 'NONE', *, *, #11186, .F. ) ;
#8151 = DIRECTION ( 'NONE',  ( -0.4999999999999918954, -0.8660254037844432595, -0.000000000000000000 ) ) ;
#8152 = AXIS2_PLACEMENT_3D ( 'NONE', #13438, #4194, #38544 ) ;
#8153 = AXIS2_PLACEMENT_3D ( 'NONE', #1573, #14105, #26683 ) ;
#8154 =( REPRESENTATION_RELATIONSHIP ('NONE','NONE', #24012, #19830 ) REPRESENTATION_RELATIONSHIP_WITH_TRANSFORMATION ( #36942 )SHAPE_REPRESENTATION_RELATIONSHIP( ) );
#8155 = CARTESIAN_POINT ( 'NONE',  ( 80.32629651820978722, 63.16159226777920566, -3.644176963625957111 ) ) ;
#8156 = LINE ( 'NONE', #39875, #39806 ) ;
#8157 = CARTESIAN_POINT ( 'NONE',  ( 78.93661819519711287, 65.67810670493912539, 2.545842637937921982 ) ) ;
#8158 = CARTESIAN_POINT ( 'NONE',  ( 21.97258699089572787, 0.9762916292323234879, 6.992449600740251014 ) ) ;
#8160 = EDGE_LOOP ( 'NONE', ( #20889, #22797, #17847, #14792 ) ) ;
#8159 = CARTESIAN_POINT ( 'NONE',  ( -0.7689628923872616761, -27.23277468313077065, 6.988553391373223178 ) ) ;
#8161 = EDGE_CURVE ( 'NONE', #23657, #24852, #33924, .T. ) ;
#8162 = EDGE_CURVE ( 'NONE', #36353, #32421, #39259, .T. ) ;
#8163 = CARTESIAN_POINT ( 'NONE',  ( 75.07588875331117606, 60.93231399735385878, -3.896954863271551162 ) ) ;
#8165 = EDGE_CURVE ( 'NONE', #16587, #15980, #34441, .T. ) ;
#8164 = CARTESIAN_POINT ( 'NONE',  ( 3.300358881314253257, -32.56994682954156417, 6.864276522220859711 ) ) ;
#8167 = DIRECTION ( 'NONE',  ( -0.000000000000000000, -0.000000000000000000, 1.000000000000000000 ) ) ;
#8166 = CARTESIAN_POINT ( 'NONE',  ( 59.69572451838116933, -0.8894979772356270686, -6.000000000000000000 ) ) ;
#8168 = DIRECTION ( 'NONE',  ( 0.000000000000000000, 0.000000000000000000, 1.000000000000000000 ) ) ;
#8169 = CYLINDRICAL_SURFACE ( 'NONE', #10075, 0.09010775117052900740 ) ;
#8170 = CARTESIAN_POINT ( 'NONE',  ( 22.52956484789606506, 4.299479892231873102, -3.494393047605991676 ) ) ;
#8171 = ORIENTED_EDGE ( 'NONE', *, *, #23351, .T. ) ;
#8172 = CARTESIAN_POINT ( 'NONE',  ( 0.9267304714826859469, -32.88073836111571779, 7.013842709614101167 ) ) ;
#8173 = CARTESIAN_POINT ( 'NONE',  ( 22.56491764776242803, -2.112007571549842755, -8.936849366082922685 ) ) ;
#8174 = DIRECTION ( 'NONE',  ( 1.000000000000000000, 0.000000000000000000, 0.000000000000000000 ) ) ;
#8175 = DIRECTION ( 'NONE',  ( 0.000000000000000000, 1.000000000000000000, 0.000000000000000000 ) ) ;
#8176 = CARTESIAN_POINT ( 'NONE',  ( 79.40189760860924650, 66.01232247510012030, 2.246767365023765617 ) ) ;
#8177 = CARTESIAN_POINT ( 'NONE',  ( 88.70663687723717317, -1.959581838532896025, -1.901098908833099621 ) ) ;
#8178 = CARTESIAN_POINT ( 'NONE',  ( 5.123097946374971734, -30.30141562551846235, 7.750000000000000888 ) ) ;
#8179 = ORIENTED_EDGE ( 'NONE', *, *, #28275, .T. ) ;
#8180 = CARTESIAN_POINT ( 'NONE',  ( -0.3426461445235795544, -32.42013594030808576, 7.501983001166816045 ) ) ;
#8181 = CIRCLE ( 'NONE', #38435, 2.500000000000000444 ) ;
#8182 = CARTESIAN_POINT ( 'NONE',  ( 23.38224997196427069, 4.144869090478608520, -2.193203930993182116 ) ) ;
#8183 = CARTESIAN_POINT ( 'NONE',  ( 26.27012936093719020, -2.986060737681520916, -4.299671860209199892 ) ) ;
#8184 = CARTESIAN_POINT ( 'NONE',  ( 37.04540850726244372, -2.801148728805186394, -5.988229962785414529 ) ) ;
#8185 = DIRECTION ( 'NONE',  ( -0.000000000000000000, -0.000000000000000000, 1.000000000000000000 ) ) ;
#8186 = CARTESIAN_POINT ( 'NONE',  ( 21.81064708091828663, 0.2586250352159095711, -8.253171913261097004 ) ) ;
#8187 = DIRECTION ( 'NONE',  ( 0.000000000000000000, 0.000000000000000000, 1.000000000000000000 ) ) ;
#8188 = ORIENTED_EDGE ( 'NONE', *, *, #2821, .T. ) ;
#8189 = CARTESIAN_POINT ( 'NONE',  ( 36.64484841828976869, -2.463732939319398074, 5.925712873318776275 ) ) ;
#8190 = AXIS2_PLACEMENT_3D ( 'NONE', #18545, #27616, #27209 ) ;
#8191 = CARTESIAN_POINT ( 'NONE',  ( 4.987265455424083171, -28.39286803235026113, 7.778495531946294506 ) ) ;
#8192 = EDGE_LOOP ( 'NONE', ( #31555, #7289, #3746, #23538 ) ) ;
#8193 = ORIENTED_EDGE ( 'NONE', *, *, #19675, .F. ) ;
#8194 = CARTESIAN_POINT ( 'NONE',  ( 37.11057928807143469, -2.402894445895731756, 5.951415949967167052 ) ) ;
#8195 = B_SPLINE_CURVE_WITH_KNOTS ( 'NONE', 3,
 ( #21607, #5953, #18918, #18495, #12528, #2891, #15410, #15624, #27969, #12325, #24899, #18703, #9430, #28172, #22018, #34593, #6367, #31486, #20120, #39044, #16427, #32899, #23421, #13754, #16822 ),
 .UNSPECIFIED., .F., .F.,
 ( 4, 2, 1, 2, 2, 1, 1, 2, 2, 1, 2, 2, 1, 2, 4 ),
 ( 0.3785350882168260211, 0.4562182021897382977, 0.4950597591761943805, 0.4999149537995015713, 0.5023425511111547781, 0.5047701484228080959, 0.5144805376694194798, 0.5339013161626424697, 0.6892675441084263888, 0.7281091010948728126, 0.7475298795880955804, 0.7572402688347070754, 0.7669506580813184593, 0.8446337720542123062, 1.000000000000000000 ),
 .UNSPECIFIED. ) ;
#8196 = CARTESIAN_POINT ( 'NONE',  ( -1.647280818465151064, -30.59125681868832913, 6.989977667959442975 ) ) ;
#8197 = LINE ( 'NONE', #20767, #38559 ) ;
#8198 = LINE ( 'NONE', #17669, #16532 ) ;
#8199 = ORIENTED_EDGE ( 'NONE', *, *, #32196, .F. ) ;
#8200 = CARTESIAN_POINT ( 'NONE',  ( 5.197301300333582397, -29.56993018336890700, 7.767301406056524193 ) ) ;
#8201 = ORIENTED_EDGE ( 'NONE', *, *, #7448, .F. ) ;
#8202 = ORIENTED_EDGE ( 'NONE', *, *, #20447, .F. ) ;
#8203 = CARTESIAN_POINT ( 'NONE',  ( -2.496911308493820147, -30.36501393308138574, 7.695279973900954751 ) ) ;
#8204 = CARTESIAN_POINT ( 'NONE',  ( 81.15619658878986797, 61.33623061796058806, -1.560659576774479973 ) ) ;
#8205 = ORIENTED_EDGE ( 'NONE', *, *, #32608, .F. ) ;
#8206 = CARTESIAN_POINT ( 'NONE',  ( 14.74038269587535233, -4.698843100384389793, 2.506102901012715822 ) ) ;
#8207 = ORIENTED_EDGE ( 'NONE', *, *, #30090, .F. ) ;
#8209 = DIRECTION ( 'NONE',  ( -1.000000000000000000, 0.000000000000000000, 0.000000000000000000 ) ) ;
#8208 = CARTESIAN_POINT ( 'NONE',  ( 4.767873141576740359, -27.88450741673118216, 6.867280401193708528 ) ) ;
#8210 = EDGE_LOOP ( 'NONE', ( #4949, #33053, #15625, #39246 ) ) ;
#8211 = CARTESIAN_POINT ( 'NONE',  ( 24.14924257540585728, 3.081831650159815084, 3.622205791944524744 ) ) ;
#8212 = CARTESIAN_POINT ( 'NONE',  ( 81.61324681686110694, 61.62795767120278612, -1.465632304122638452 ) ) ;
#8213 = VECTOR ( 'NONE', #35432, 1000.000000000000000 ) ;
#8214 = AXIS2_PLACEMENT_3D ( 'NONE', #5593, #24526, #18135 ) ;
#8216 = EDGE_CURVE ( 'NONE', #18044, #6925, #1543, .T. ) ;
#8215 = DIRECTION ( 'NONE',  ( -1.000000000000000000, 0.000000000000000000, 0.000000000000000000 ) ) ;
#8217 = ORIENTED_EDGE ( 'NONE', *, *, #26139, .T. ) ;
#8219 = CARTESIAN_POINT ( 'NONE',  ( 22.74155280133190260, -2.655454342507609145, -3.755767339817497774 ) ) ;
#8218 = CARTESIAN_POINT ( 'NONE',  ( -70.92837670882107659, -65.19654454972992141, 0.000000000000000000 ) ) ;
#8220 = CARTESIAN_POINT ( 'NONE',  ( -1.799471907747695942, -29.53885005966835919, 6.894806418505347700 ) ) ;
#8221 = CARTESIAN_POINT ( 'NONE',  ( 76.13754644452941989, 60.10671110989439114, 3.424891502433685009 ) ) ;
#8222 = CARTESIAN_POINT ( 'NONE',  ( 22.97307122621484865, 2.409484201040166251, -4.646973716149349620 ) ) ;
#8223 = EDGE_LOOP ( 'NONE', ( #27328, #37364, #8201, #28998 ) ) ;
#8224 = VECTOR ( 'NONE', #25451, 1000.000000000000000 ) ;
#8225 = CARTESIAN_POINT ( 'NONE',  ( 16.11725891508299924, 15.27317977276803873, 2.500000000000000000 ) ) ;
#8226 = DIRECTION ( 'NONE',  ( -0.000000000000000000, -1.000000000000000000, -0.000000000000000000 ) ) ;
#8227 = CARTESIAN_POINT ( 'NONE',  ( 4.878343045835490166, -30.77848925561357873, 6.894806418505348589 ) ) ;
#8228 = CARTESIAN_POINT ( 'NONE',  ( -1.654007494988858573, -29.01493754880614517, 7.692469944509195301 ) ) ;
#8229 = CARTESIAN_POINT ( 'NONE',  ( 82.08208307362221490, 62.96685751817979337, 2.430878896394114808 ) ) ;
#8230 = CARTESIAN_POINT ( 'NONE',  ( 87.61456772748933020, -0.05511631305283664489, -4.124113870075747812 ) ) ;
#8231 = CARTESIAN_POINT ( 'NONE',  ( 29.93139500891458127, 0.4880113553092989553, -5.118255730029571460 ) ) ;
#8232 = CARTESIAN_POINT ( 'NONE',  ( -77.05165876229449395, -4.661780768167600009, -9.444144087646179742 ) ) ;
#8233 = ORIENTED_EDGE ( 'NONE', *, *, #3313, .T. ) ;
#8234 = FACE_OUTER_BOUND ( 'NONE', #24737, .T. ) ;
#8235 = CARTESIAN_POINT ( 'NONE',  ( -34.34874870218063592, -25.49307895267003587, 6.700000000000000178 ) ) ;
#8236 = CARTESIAN_POINT ( 'NONE',  ( 36.81799887185016473, -2.525268165826815459, -5.952737189256588124 ) ) ;
#8237 = DIRECTION ( 'NONE',  ( 0.000000000000000000, 0.000000000000000000, 1.000000000000000000 ) ) ;
#8238 = CARTESIAN_POINT ( 'NONE',  ( 4.632207264391903223, -31.48159488532770212, 6.931070083220553180 ) ) ;
#8239 = PRODUCT ( 'Fixed Die', 'Fixed Die', '', ( #7316 ) ) ;
#8240 = DIRECTION ( 'NONE',  ( -0.000000000000000000, -0.000000000000000000, 1.000000000000000000 ) ) ;
#8241 = EDGE_CURVE ( 'NONE', #33614, #3549, #33935, .T. ) ;
#8242 = CARTESIAN_POINT ( 'NONE',  ( -38.97867591359219119, -24.55319635012989110, 6.800000000000000711 ) ) ;
#8243 = AXIS2_PLACEMENT_3D ( 'NONE', #31883, #26108, #3695 ) ;
#8244 = LINE ( 'NONE', #2727, #8578 ) ;
#8245 = ORIENTED_EDGE ( 'NONE', *, *, #21712, .F. ) ;
#8246 = CARTESIAN_POINT ( 'NONE',  ( 36.70930901955060222, -3.420528228347338828, 5.875135601664768892 ) ) ;
#8247 = CARTESIAN_POINT ( 'NONE',  ( -2.619165735930222727, -32.12635497920775407, 7.695279973900954751 ) ) ;
#8248 = CARTESIAN_POINT ( 'NONE',  ( 66.73521764480442187, 57.83500309307840581, -3.999076693781861813 ) ) ;
#8249 = FACE_OUTER_BOUND ( 'NONE', #16143, .T. ) ;
#8250 = ORIENTED_EDGE ( 'NONE', *, *, #1516, .F. ) ;
#8251 = DIRECTION ( 'NONE',  ( -0.000000000000000000, -0.000000000000000000, 1.000000000000000000 ) ) ;
#8252 = LINE ( 'NONE', #10741, #8134 ) ;
#8253 = CARTESIAN_POINT ( 'NONE',  ( -14.87867591359218977, -26.64985754041175525, 6.800000000000000711 ) ) ;
#8254 = CARTESIAN_POINT ( 'NONE',  ( -79.60043556232082551, 11.50163111191179866, 4.996739675375823531 ) ) ;
#8255 =( BOUNDED_SURFACE ( )  B_SPLINE_SURFACE ( 3, 2, ( 
 ( #12958, #6178, #37859 ),
 ( #18720, #19341, #9663 ),
 ( #28188, #31704, #6388 ),
 ( #15, #12546, #3520 ),
 ( #2707, #12127, #1234 ),
 ( #20137, #19744, #7782 ),
 ( #31911, #7379, #32127 ),
 ( #10660, #29018, #19937 ),
 ( #32515, #17033, #1428 ),
 ( #822, #13960, #1026 ),
 ( #620, #13353, #26527 ),
 ( #13560, #4314, #22647 ),
 ( #28817, #26336, #13163 ),
 ( #23239, #35213, #38460 ),
 ( #25724, #16836, #38266 ),
 ( #22843, #6985, #19551 ) ),
 .UNSPECIFIED., .F., .F., .F. ) 
 B_SPLINE_SURFACE_WITH_KNOTS ( ( 4, 2, 2, 2, 2, 2, 2, 4 ),
 ( 3, 3 ),
 ( 6.938893903907228378E-18, 0.0008952345629814628409, 0.001342851844472190900, 0.001790469125962918743, 0.002238086407453646585, 0.002685703688944374862, 0.003133320970435102704, 0.003580938251925830547 ),
 ( 0.000000000000000000, 1.000000000000000000 ),
 .UNSPECIFIED. ) 
 GEOMETRIC_REPRESENTATION_ITEM ( )  RATIONAL_B_SPLINE_SURFACE ( (
 ( 1.000000000000000000, 0.7071067811865473507, 1.000000000000000000),
 ( 1.000000000000000000, 0.7332884733985617354, 1.000000000000000000),
 ( 1.000000000000000000, 0.7573851245654280584, 1.000000000000000000),
 ( 1.000000000000000000, 0.7911185894615297975, 1.000000000000000000),
 ( 1.000000000000000000, 0.8019092923332744594, 1.000000000000000000),
 ( 1.000000000000000000, 0.8220850550644049903, 1.000000000000000000),
 ( 1.000000000000000000, 0.8315581304763710602, 1.000000000000000000),
 ( 1.000000000000000000, 0.8492897706874269481, 1.000000000000000000),
 ( 1.000000000000000000, 0.8574674522647928177, 1.000000000000000000),
 ( 1.000000000000000000, 0.8719072631877536894, 1.000000000000000000),
 ( 1.000000000000000000, 0.8783188977574709622, 1.000000000000000000),
 ( 1.000000000000000000, 0.8888416513947781095, 1.000000000000000000),
 ( 1.000000000000000000, 0.8929346545673477742, 1.000000000000000000),
 ( 1.000000000000000000, 0.8985797510527644416, 1.000000000000000000),
 ( 1.000000000000000000, 0.9000264109954028147, 1.000000000000000000),
 ( 1.000000000000000000, 0.9000259740535768715, 1.000000000000000000) ) ) 
 REPRESENTATION_ITEM ( '' )  SURFACE ( )  );
#8256 = B_SPLINE_CURVE_WITH_KNOTS ( 'NONE', 3,
 ( #39085, #26155, #3944, #13181 ),
 .UNSPECIFIED., .F., .F.,
 ( 4, 4 ),
 ( 0.000000000000000000, 6.391136169898598526E-06 ),
 .UNSPECIFIED. ) ;
#8257 = CARTESIAN_POINT ( 'NONE',  ( 0.3642935312485215960, -32.80488561534932757, 6.877402575842993748 ) ) ;
#8258 = CARTESIAN_POINT ( 'NONE',  ( -17.07867591359219617, -24.55319635012989110, 6.700000000000000178 ) ) ;
#8259 = EDGE_LOOP ( 'NONE', ( #36223, #39781, #8815, #24678 ) ) ;
#8260 = CARTESIAN_POINT ( 'NONE',  ( 21.71651422438785417, 6.289002153562915254, 3.207190368607817810 ) ) ;
#8261 = CARTESIAN_POINT ( 'NONE',  ( 82.54941478318325210, 63.90107490703079662, -1.303631908149876617 ) ) ;
#8262 = CARTESIAN_POINT ( 'NONE',  ( 78.72446908900997187, 66.04077733106291248, 1.541060042019483989 ) ) ;
#8264 = EDGE_CURVE ( 'NONE', #36985, #14798, #31273, .T. ) ;
#8263 = CARTESIAN_POINT ( 'NONE',  ( -0.04602064563813425963, -32.48713041901819309, 6.889465824494256374 ) ) ;
#8265 = ORIENTED_EDGE ( 'NONE', *, *, #34074, .T. ) ;
#8266 = CARTESIAN_POINT ( 'NONE',  ( 77.65955580186951579, 62.78993503910590590, -3.839379600940507231 ) ) ;
#8268 = CARTESIAN_POINT ( 'NONE',  ( 14.74221411508265689, -5.125435651542595394, -2.499999999999999556 ) ) ;
#8267 = CARTESIAN_POINT ( 'NONE',  ( 22.28288117080667163, 0.2420143529008198235, 7.135959080246487396 ) ) ;
#8269 = CARTESIAN_POINT ( 'NONE',  ( 81.40003982928756443, 62.35377290961280750, -2.797238656122826850 ) ) ;
#8270 = CARTESIAN_POINT ( 'NONE',  ( 78.15185181088402544, 63.91595853815784523, 3.616565173810659672 ) ) ;
#8271 = VERTEX_POINT ( 'NONE', #37399 ) ;
#8272 = CARTESIAN_POINT ( 'NONE',  ( 36.86728531260331465, -3.360612826157867605, -5.906623357289592313 ) ) ;
#8273 = VERTEX_POINT ( 'NONE', #6123 ) ;
#8274 = CARTESIAN_POINT ( 'NONE',  ( 78.98267122246093663, 66.20432814577486624, 1.134074597586614663 ) ) ;
#8277 = ORIENTED_EDGE ( 'NONE', *, *, #3672, .T. ) ;
#8276 = CARTESIAN_POINT ( 'NONE',  ( -4.248748702180636272, -25.49307895267003587, 6.700000000000000178 ) ) ;
#8275 = LINE ( 'NONE', #33842, #32967 ) ;
#8278 = CARTESIAN_POINT ( 'NONE',  ( 26.75871784592184710, 2.055338430770167424, -4.125980934060708982 ) ) ;
#8279 = LINE ( 'NONE', #20854, #12239 ) ;
#8280 = DIRECTION ( 'NONE',  ( 0.000000000000000000, 0.000000000000000000, 1.000000000000000000 ) ) ;
#8281 = VERTEX_POINT ( 'NONE', #37801 ) ;
#8282 = CARTESIAN_POINT ( 'NONE',  ( -80.83308087135290521, -6.606543372238043332, 1.435207014940032444 ) ) ;
#8283 = CARTESIAN_POINT ( 'NONE',  ( 21.73414427015508110, 0.2235801105871568495, -9.085705942277243707 ) ) ;
#8284 = CIRCLE ( 'NONE', #14231, 0.1000000000000028644 ) ;
#8285 = ADVANCED_FACE ( 'NONE', ( #24858 ), #31246, .T. ) ;
#8286 = CARTESIAN_POINT ( 'NONE',  ( -1.795519090086910019, -29.40075872605237706, 7.013842709614101167 ) ) ;
#8287 = LINE ( 'NONE', #20861, #10568 ) ;
#8288 = CARTESIAN_POINT ( 'NONE',  ( -1.059169042549344519, -31.72279695996654780, 7.751599049952176301 ) ) ;
#8289 = CARTESIAN_POINT ( 'NONE',  ( 37.00800308128324190, -3.245149801803746570, -5.947249437311571185 ) ) ;
#8290 = CARTESIAN_POINT ( 'NONE',  ( 30.80771206660583061, -3.555147752975252651, -4.834189129258772866 ) ) ;
#8291 = AXIS2_PLACEMENT_3D ( 'NONE', #39843, #20686, #5254 ) ;
#8292 = DIRECTION ( 'NONE',  ( 0.000000000000000000, 1.000000000000000000, 0.000000000000000000 ) ) ;
#8293 = CARTESIAN_POINT ( 'NONE',  ( -0.07800893100938692537, -26.55541330231165986, 7.720710062488889136 ) ) ;
#8294 = DIRECTION ( 'NONE',  ( 0.000000000000000000, 0.000000000000000000, -1.000000000000000000 ) ) ;
#8295 = CARTESIAN_POINT ( 'NONE',  ( 1.736346942945644400, -33.06974547922812491, 7.695279973900954751 ) ) ;
#8296 = DIRECTION ( 'NONE',  ( 1.000000000000000000, 0.000000000000000000, 0.000000000000000000 ) ) ;
#8297 = CARTESIAN_POINT ( 'NONE',  ( 1.574364539997139767, -33.06766052747819629, 7.750000000000000888 ) ) ;
#8298 = CARTESIAN_POINT ( 'NONE',  ( 23.71146206689260083, 1.800196029863365688, -4.690086670497853660 ) ) ;
#8299 = ORIENTED_EDGE ( 'NONE', *, *, #3346, .T. ) ;
#8300 = EDGE_CURVE ( 'NONE', #10467, #32354, #1979, .T. ) ;
#8302 = EDGE_CURVE ( 'NONE', #24328, #25004, #24309, .T. ) ;
#8301 = CARTESIAN_POINT ( 'NONE',  ( 66.41407057682036452, 57.81332248272642715, 4.000000000000022204 ) ) ;
#8303 = CARTESIAN_POINT ( 'NONE',  ( 73.68879688780705806, 59.40709336146452557, -3.677837812263893280 ) ) ;
#8304 = ADVANCED_FACE ( 'NONE', ( #6327 ), #15794, .F. ) ;
#8305 = VERTEX_POINT ( 'NONE', #18875 ) ;
#8306 = CARTESIAN_POINT ( 'NONE',  ( 87.91343731185466481, -2.496140582104141359, -0.8634702502314072214 ) ) ;
#8307 = DIRECTION ( 'NONE',  ( -0.000000000000000000, -0.000000000000000000, -1.000000000000000000 ) ) ;
#8308 = AXIS2_PLACEMENT_3D ( 'NONE', #18489, #31483, #191 ) ;
#8309 = CARTESIAN_POINT ( 'NONE',  ( -0.8851743599023897957, -27.21093538503495068, 6.875780273367530171 ) ) ;
#8310 = VECTOR ( 'NONE', #30487, 1000.000000000000000 ) ;
#8311 = CONTEXT_DEPENDENT_SHAPE_REPRESENTATION ( #40509, #2637 ) ;
#8312 = AXIS2_PLACEMENT_3D ( 'NONE', #34478, #6253, #37126 ) ;
#8313 = CARTESIAN_POINT ( 'NONE',  ( 2.202186418506070886, -32.93269696804298974, 7.778050822775631978 ) ) ;
#8314 = ORIENTED_EDGE ( 'NONE', *, *, #2333, .F. ) ;
#8315 = CARTESIAN_POINT ( 'NONE',  ( -14.34874870218063769, -26.64985754041175525, 6.800000000000000711 ) ) ;
#8316 = CARTESIAN_POINT ( 'NONE',  ( -2.248748702180634940, -26.64985754041175525, 6.700000000000000178 ) ) ;
#8317 = EDGE_CURVE ( 'NONE', #30447, #7067, #33848, .T. ) ;
#8318 = ORIENTED_EDGE ( 'NONE', *, *, #23697, .F. ) ;
#8319 = CARTESIAN_POINT ( 'NONE',  ( 79.65304550238739978, 63.88563316389422653, -3.730195463674648604 ) ) ;
#8320 = CARTESIAN_POINT ( 'NONE',  ( 19.55994200078226797, 8.628030550684337996, -2.500000000001137757 ) ) ;
#8321 = CARTESIAN_POINT ( 'NONE',  ( 81.83960663661402180, 62.56551448482339595, -2.484976468875490063 ) ) ;
#8322 = CARTESIAN_POINT ( 'NONE',  ( 78.43571320973860850, 65.80086540191352640, 1.884339924308606085 ) ) ;
#8323 = DIRECTION ( 'NONE',  ( 0.000000000000000000, 1.000000000000000000, 0.000000000000000000 ) ) ;
#8324 = B_SPLINE_CURVE_WITH_KNOTS ( 'NONE', 3,
 ( #26892, #1592, #2005, #36169, #8137, #10829, #8553, #14724, #39860, #26700, #2204, #1398, #13928, #36368, #23993, #20301, #39236, #7950, #39435, #36770, #14323, #26501, #39031, #36564, #23406, #14123, #33504, #32886, #35974, #4673, #8345 ),
 .UNSPECIFIED., .F., .F.,
 ( 4, 3, 3, 3, 3, 3, 3, 3, 3, 3, 4 ),
 ( 8.673617379884035472E-19, 2.999644130997317255E-05, 6.002588995694823926E-05, 8.960886084587800678E-05, 0.0001190604700446473311, 0.0001489538463052700670, 0.0001796139255493905637, 0.0002109707048517013323, 0.0002426195318110273063, 0.0002740640997889962093, 0.0002849778069099833354 ),
 .UNSPECIFIED. ) ;
#8325 = CARTESIAN_POINT ( 'NONE',  ( 21.78047233922835346, 5.616103166486084319, -3.473245622192032034 ) ) ;
#8327 = ORIENTED_EDGE ( 'NONE', *, *, #32242, .F. ) ;
#8326 = CARTESIAN_POINT ( 'NONE',  ( -17.69482985384421880, -29.56993018339339940, 6.000000000000000000 ) ) ;
#8328 = CARTESIAN_POINT ( 'NONE',  ( 21.85643539959778892, -10.77729622265174392, -9.134175241038137827 ) ) ;
#8329 = EDGE_LOOP ( 'NONE', ( #24062, #13818, #35249, #14259, #28637 ) ) ;
#8330 = CARTESIAN_POINT ( 'NONE',  ( -77.61846184184865649, 9.846684257009661323, 7.446037897971843122 ) ) ;
#8331 = CARTESIAN_POINT ( 'NONE',  ( 14.72854306895793286, -5.062769318467021051, 2.500000000002235101 ) ) ;
#8332 = VECTOR ( 'NONE', #26931, 1000.000000000000000 ) ;
#8333 = CARTESIAN_POINT ( 'NONE',  ( -79.87311179269229910, 11.51046329118718958, -4.489559985497344030 ) ) ;
#8334 = CARTESIAN_POINT ( 'NONE',  ( 1.519484703345444609, -32.96512359005904358, 6.887945620086119547 ) ) ;
#8335 = FACE_OUTER_BOUND ( 'NONE', #623, .T. ) ;
#8336 = CARTESIAN_POINT ( 'NONE',  ( 4.907464300517769829, -30.69894525369553762, 7.695279973900954751 ) ) ;
#8337 = CARTESIAN_POINT ( 'NONE',  ( 3.976216693700143523, -27.04394172819598907, 7.757178535559533294 ) ) ;
#8338 = CARTESIAN_POINT ( 'NONE',  ( -45.33131703149249603, -29.56993018339339940, 6.000000000000000000 ) ) ;
#8339 = CARTESIAN_POINT ( 'NONE',  ( 0.5468258811901485217, -26.26548310648608009, 6.880608371227950215 ) ) ;
#8340 = VECTOR ( 'NONE', #26043, 1000.000000000000000 ) ;
#8341 = VECTOR ( 'NONE', #24629, 1000.000000000000000 ) ;
#8342 = CARTESIAN_POINT ( 'NONE',  ( 4.500789674022213305, -27.47046303393648614, 6.941203072598479906 ) ) ;
#8343 = EDGE_CURVE ( 'NONE', #20380, #25477, #27489, .T. ) ;
#8344 = DIRECTION ( 'NONE',  ( 0.000000000000000000, -0.000000000000000000, 1.000000000000000000 ) ) ;
#8345 = CARTESIAN_POINT ( 'NONE',  ( 4.273337484900067373, -31.79252814967387053, 6.894806418505345036 ) ) ;
#8346 = ORIENTED_EDGE ( 'NONE', *, *, #10125, .T. ) ;
#8347 = CARTESIAN_POINT ( 'NONE',  ( 67.69980720754315939, 58.37350455430767937, 3.995247128881052046 ) ) ;
#8348 = CARTESIAN_POINT ( 'NONE',  ( 33.68694953669930925, -3.106715461681162971, 5.464061215791960358 ) ) ;
#8349 = EDGE_CURVE ( 'NONE', #13245, #21734, #9812, .T. ) ;
#8350 = EDGE_LOOP ( 'NONE', ( #10985, #31039, #38270 ) ) ;
#8351 = DIRECTION ( 'NONE',  ( -1.000000000000000000, -0.000000000000000000, -0.000000000000000000 ) ) ;
#8352 = CARTESIAN_POINT ( 'NONE',  ( 85.96608680028057847, 1.729603650198207054, 5.123763289084741324 ) ) ;
#8354 = CARTESIAN_POINT ( 'NONE',  ( 31.24780275965614962, -0.3897380699759783740, -5.083373370246649259 ) ) ;
#8353 = DIRECTION ( 'NONE',  ( 1.000000000000000000, 0.000000000000000000, 0.000000000000000000 ) ) ;
#8355 = DIRECTION ( 'NONE',  ( -1.000000000000000000, 0.000000000000000000, 0.000000000000000000 ) ) ;
#8356 = CARTESIAN_POINT ( 'NONE',  ( -57.95974551600828306, 28.52258727176715780, 2.765331207962179239 ) ) ;
#8357 = CARTESIAN_POINT ( 'NONE',  ( -0.6928964808853791402, -32.12378599331628948, 6.941203072598472801 ) ) ;
#8358 = B_SPLINE_CURVE_WITH_KNOTS ( 'NONE', 3,
 ( #36712, #30548, #2361, #2980, #15500, #37518, #24984, #18172, #21488, #9314 ),
 .UNSPECIFIED., .F., .F.,
 ( 4, 3, 3, 4 ),
 ( 0.0002170292169044720973, 0.0002420761345915967968, 0.0002723302478206991728, 0.0002816811360866699164 ),
 .UNSPECIFIED. ) ;
#8359 = ORIENTED_EDGE ( 'NONE', *, *, #11986, .F. ) ;
#8360 = DIRECTION ( 'NONE',  ( 1.000000000000000000, -0.000000000000000000, 0.000000000000000000 ) ) ;
#8361 = EDGE_LOOP ( 'NONE', ( #33245, #39618, #23431, #8597 ) ) ;
#8362 = VERTEX_POINT ( 'NONE', #35558 ) ;
#8363 = CARTESIAN_POINT ( 'NONE',  ( 79.45910779949859659, 64.84755599131122494, -3.411701596789212143 ) ) ;
#8364 =( GEOMETRIC_REPRESENTATION_CONTEXT ( 3 ) GLOBAL_UNCERTAINTY_ASSIGNED_CONTEXT ( ( #5704 ) ) GLOBAL_UNIT_ASSIGNED_CONTEXT ( ( #38397, #151, #28335 ) ) REPRESENTATION_CONTEXT ( 'NONE', 'WORKASPACE' ) );
#8365 = CARTESIAN_POINT ( 'NONE',  ( -1.538176338396153753, -28.24264443121935386, 6.872971584836694348 ) ) ;
#8366 = AXIS2_PLACEMENT_3D ( 'NONE', #36660, #37464, #11525 ) ;
#8367 = CARTESIAN_POINT ( 'NONE',  ( 79.06216475166051794, 65.51459655345146871, 2.804471013201318197 ) ) ;
#8368 = CARTESIAN_POINT ( 'NONE',  ( 26.96776543102747681, 1.407182095274382982, 4.403121069298014056 ) ) ;
#8370 = ORIENTED_EDGE ( 'NONE', *, *, #18209, .T. ) ;
#8369 = CARTESIAN_POINT ( 'NONE',  ( 4.752662398340829597, -27.88579754063074034, 7.784725160561909441 ) ) ;
#8371 = VECTOR ( 'NONE', #21107, 1000.000000000000000 ) ;
#8372 = CARTESIAN_POINT ( 'NONE',  ( 74.44738948069034734, 59.23650550459285569, -3.391332960764822602 ) ) ;
#8373 = CARTESIAN_POINT ( 'NONE',  ( -70.92837670882140344, -21.78291075931342391, 6.000000000000002665 ) ) ;
#8375 = CARTESIAN_POINT ( 'NONE',  ( -45.33131703149249603, -29.56993018339339940, 6.800000000000000711 ) ) ;
#8374 = CARTESIAN_POINT ( 'NONE',  ( 87.04213330793392345, 0.5878691963682337596, 6.000000000000000000 ) ) ;
#8376 = CARTESIAN_POINT ( 'NONE',  ( 2.921324086407800280, -24.55319635012989110, 6.800000000000000711 ) ) ;
#8377 = CARTESIAN_POINT ( 'NONE',  ( 4.792526203416204389, -27.93020634197934982, 7.750000000000000888 ) ) ;
#8378 = CARTESIAN_POINT ( 'NONE',  ( 23.42523798194068974, 3.747132905502745359, -3.204823688547873139 ) ) ;
#8379 = ORIENTED_EDGE ( 'NONE', *, *, #26172, .F. ) ;
#8380 = LINE ( 'NONE', #21580, #22219 ) ;
#8381 = ADVANCED_FACE ( 'NONE', ( #38407 ), #4463, .T. ) ;
#8382 = CARTESIAN_POINT ( 'NONE',  ( 22.49462040199967916, -0.5704057512449431933, -9.208717712401224276 ) ) ;
#8383 = CARTESIAN_POINT ( 'NONE',  ( 2.896951166878261930, -32.75242002648047901, 7.692469944509197077 ) ) ;
#8384 = DIRECTION ( 'NONE',  ( -0.000000000000000000, -0.000000000000000000, 1.000000000000000000 ) ) ;
#8385 = CARTESIAN_POINT ( 'NONE',  ( 80.04208101465529523, 65.56312698749549384, 2.920975158735862998 ) ) ;
#8386 = CARTESIAN_POINT ( 'NONE',  ( 85.22136629666657370, 2.371628277241609517, -4.205523829021379001 ) ) ;
#8387 =( BOUNDED_CURVE ( )  B_SPLINE_CURVE ( 3, ( #29983, #34529, #6514, #34123 ),
 .UNSPECIFIED., .F., .T. ) 
 B_SPLINE_CURVE_WITH_KNOTS ( ( 4, 4 ),
 ( 4.708531083176465515, 4.895802057644187855 ),
 .UNSPECIFIED. ) 
 CURVE ( )  GEOMETRIC_REPRESENTATION_ITEM ( )  RATIONAL_B_SPLINE_CURVE ( ( 1.000000000000000000, 0.9970795998553221295, 0.9970795998553221295, 1.000000000000000000 ) ) 
 REPRESENTATION_ITEM ( '' )  );
#8388 = CARTESIAN_POINT ( 'NONE',  ( -71.72837670882105954, -34.30579396504363388, -1.385640646055078307 ) ) ;
#8389 = ORIENTED_EDGE ( 'NONE', *, *, #24928, .T. ) ;
#8390 = DIRECTION ( 'NONE',  ( 0.000000000000000000, 0.000000000000000000, 1.000000000000000000 ) ) ;
#8391 = ADVANCED_FACE ( 'NONE', ( #23181 ), #10495, .T. ) ;
#8392 = EDGE_LOOP ( 'NONE', ( #11141, #149, #11893, #11167 ) ) ;
#8393 = AXIS2_PLACEMENT_3D ( 'NONE', #20093, #16789, #32869 ) ;
#8394 = FACE_OUTER_BOUND ( 'NONE', #35744, .T. ) ;
#8395 = EDGE_CURVE ( 'NONE', #34207, #19528, #7087, .T. ) ;
#8396 = CARTESIAN_POINT ( 'NONE',  ( 15.29064274479596719, -3.935957078823225874, -2.582637740313979968 ) ) ;
#8397 = CARTESIAN_POINT ( 'NONE',  ( 36.79680087876906214, -2.557513486141199444, -5.949428729760880330 ) ) ;
#8398 = DIRECTION ( 'NONE',  ( 0.000000000000000000, 1.000000000000000000, 0.000000000000000000 ) ) ;
#8399 = CARTESIAN_POINT ( 'NONE',  ( 23.62653219015538042, 0.5414986629106450788, -5.462610290562567528 ) ) ;
#8400 = CARTESIAN_POINT ( 'NONE',  ( -0.3937826876777428264, -26.89141458432633769, 7.759451378593096749 ) ) ;
#8401 = ORIENTED_EDGE ( 'NONE', *, *, #38992, .T. ) ;
#8402 = CARTESIAN_POINT ( 'NONE',  ( 36.19294238595723812, -2.234500302844026010, 5.855182007584707193 ) ) ;
#8403 = EDGE_CURVE ( 'NONE', #5452, #40540, #6735, .T. ) ;
#8404 = EDGE_CURVE ( 'NONE', #18601, #39861, #11266, .T. ) ;
#8405 = CARTESIAN_POINT ( 'NONE',  ( 85.36681891225420316, 2.469661840813765608, 2.484336716295309166 ) ) ;
#8406 = ORIENTED_EDGE ( 'NONE', *, *, #12472, .T. ) ;
#8407 = ORIENTED_EDGE ( 'NONE', *, *, #15587, .T. ) ;
#8409 = CARTESIAN_POINT ( 'NONE',  ( 35.83265631856147593, -3.731003872579450764, 5.622499855908868582 ) ) ;
#8408 = CARTESIAN_POINT ( 'NONE',  ( 81.26385631823474398, 62.29349618781996156, -2.861733672647096327 ) ) ;
#8410 = CARTESIAN_POINT ( 'NONE',  ( 30.67406393699503298, -3.593393542108534344, -4.777508688867102116 ) ) ;
#8411 = CARTESIAN_POINT ( 'NONE',  ( 3.817924346030161509, -32.35669330361569962, 7.013842709614101167 ) ) ;
#8412 = ORIENTED_EDGE ( 'NONE', *, *, #28318, .T. ) ;
#8413 = FACE_OUTER_BOUND ( 'NONE', #6964, .T. ) ;
#8414 = ORIENTED_EDGE ( 'NONE', *, *, #17357, .T. ) ;
#8415 = ORIENTED_EDGE ( 'NONE', *, *, #11932, .F. ) ;
#8416 = DIRECTION ( 'NONE',  ( 1.000000000000000000, 1.288651725011342548E-14, 0.000000000000000000 ) ) ;
#8417 = CARTESIAN_POINT ( 'NONE',  ( 79.53763471700084153, 65.25825451995501680, -3.163072811751571400 ) ) ;
#8418 = VECTOR ( 'NONE', #18263, 1000.000000000000114 ) ;
#8419 = CARTESIAN_POINT ( 'NONE',  ( 4.758694053898627985, -27.86793814928234525, 6.875671892026064214 ) ) ;
#8420 = ORIENTED_EDGE ( 'NONE', *, *, #16134, .T. ) ;
#8421 = CARTESIAN_POINT ( 'NONE',  ( 22.18094696048607517, 4.340889477042914280, 3.790884728818065597 ) ) ;
#8422 = CARTESIAN_POINT ( 'NONE',  ( 81.40691186390333201, 61.43583663329572886, -1.251938014746444727 ) ) ;
#8423 = CARTESIAN_POINT ( 'NONE',  ( 4.741166332522630533, -28.04885166386452156, 6.988553391373221402 ) ) ;
#8424 = ORIENTED_EDGE ( 'NONE', *, *, #34584, .F. ) ;
#8426 = CARTESIAN_POINT ( 'NONE',  ( 21.92193887068393110, -2.651946117302231620, -3.627846763502060590 ) ) ;
#8425 = CARTESIAN_POINT ( 'NONE',  ( -5.316495087772350914, -32.84709638682603838, 0.000000000000000000 ) ) ;
#8427 = DIRECTION ( 'NONE',  ( -0.000000000000000000, -0.000000000000000000, 1.000000000000000000 ) ) ;
#8428 = CARTESIAN_POINT ( 'NONE',  ( 74.39246203999459794, 62.41596060291492876, 3.584990529380562840 ) ) ;
#8429 = CARTESIAN_POINT ( 'NONE',  ( 24.01376084489890417, 2.453835260611390456, -4.174832439456215738 ) ) ;
#8430 = VERTEX_POINT ( 'NONE', #32664 ) ;
#8431 = CARTESIAN_POINT ( 'NONE',  ( -22.97867591359219119, -26.64985754041175525, 6.700000000000000178 ) ) ;
#8432 = CARTESIAN_POINT ( 'NONE',  ( -4.220127061295482087E-17, 0.7293679304675931840, 6.000000000000000000 ) ) ;
#8433 = CARTESIAN_POINT ( 'NONE',  ( -4.890026461918814071, -8.228598103685714525E-16, -2.500000000000000000 ) ) ;
#8434 = CARTESIAN_POINT ( 'NONE',  ( -65.87013514635467004, 36.66000420377765323, 7.725785790319501523 ) ) ;
#8435 = CARTESIAN_POINT ( 'NONE',  ( 79.40575531231837658, 66.18134094231186282, 1.781440269582215796 ) ) ;
#8436 = CARTESIAN_POINT ( 'NONE',  ( 88.35060396620406209, -0.8818671507646100860, -0.7863509125847466530 ) ) ;
#8437 = CARTESIAN_POINT ( 'NONE',  ( 29.97939791730999914, 0.4010955892747467555, 5.210136963171234648 ) ) ;
#8438 = PRODUCT_DEFINITION ( 'UNKNOWN', '', #13007, #18868 ) ;
#8439 = CARTESIAN_POINT ( 'NONE',  ( 2.861759009453783253, -32.87163717142679786, 6.887161170156907097 ) ) ;
#8440 = VERTEX_POINT ( 'NONE', #38010 ) ;
#8441 = CARTESIAN_POINT ( 'NONE',  ( 0.6556028735496977067, -26.33441960479748545, 6.863904403958576594 ) ) ;
#8442 = CARTESIAN_POINT ( 'NONE',  ( 0.1194166765537494485, -26.44734742936537231, 6.951256099901593544 ) ) ;
#8443 = VECTOR ( 'NONE', #15501, 1000.000000000000000 ) ;
#8444 = CARTESIAN_POINT ( 'NONE',  ( 36.42653508247762772, -3.159901027683388985, -5.891639797337469453 ) ) ;
#8445 = DIRECTION ( 'NONE',  ( 0.000000000000000000, 0.000000000000000000, -1.000000000000000000 ) ) ;
#8446 = CARTESIAN_POINT ( 'NONE',  ( -75.45330471031414277, 33.71485196875532608, 8.800414904976364028 ) ) ;
#8447 = DIRECTION ( 'NONE',  ( -1.000000000000000000, 0.000000000000000000, 0.000000000000000000 ) ) ;
#8448 = DIRECTION ( 'NONE',  ( 0.000000000000000000, -1.000000000000000000, 0.000000000000000000 ) ) ;
#8449 = EDGE_CURVE ( 'NONE', #34557, #25138, #764, .T. ) ;
#8450 = DIRECTION ( 'NONE',  ( -0.000000000000000000, -0.000000000000000000, 1.000000000000000000 ) ) ;
#8451 = EDGE_CURVE ( 'NONE', #14204, #11497, #21690, .T. ) ;
#8452 = EDGE_LOOP ( 'NONE', ( #20078, #36416, #14998, #36877 ) ) ;
#8453 = CARTESIAN_POINT ( 'NONE',  ( 29.41998804195583972, 1.119444561410238625, 4.432470294405459477 ) ) ;
#8454 = CARTESIAN_POINT ( 'NONE',  ( -71.25654746924473670, 0.1680418597759353594, 6.003896035474988402 ) ) ;
#8455 = CARTESIAN_POINT ( 'NONE',  ( 66.90457105084450973, 57.82508126828634687, -3.996770903026528821 ) ) ;
#8456 = CARTESIAN_POINT ( 'NONE',  ( -71.54296365563132554, 0.01656620227473614565, 9.981524770340062247 ) ) ;
#8457 = CARTESIAN_POINT ( 'NONE',  ( -0.5468503132381580256, -26.89089984877168149, 7.767720160662276108 ) ) ;
#8458 = VERTEX_POINT ( 'NONE', #16193 ) ;
#8459 = CARTESIAN_POINT ( 'NONE',  ( -1.666363480296579214, -25.64183336440431660, 7.695279973900954751 ) ) ;
#8460 = CARTESIAN_POINT ( 'NONE',  ( 3.912314530024866954, -32.15206040780897467, 7.712764235869105534 ) ) ;
#8461 = CARTESIAN_POINT ( 'NONE',  ( 70.64617143260556986, 60.54601068761595428, 3.764554023424209195 ) ) ;
#8462 = CARTESIAN_POINT ( 'NONE',  ( -73.84684882489183622, 8.474083953686129433, 9.568945070976022649 ) ) ;
#8463 = B_SPLINE_CURVE_WITH_KNOTS ( 'NONE', 3,
 ( #17494, #33399, #36458, #7848, #36070, #17297, #29876, #20595, #23506, #1486, #1690, #7443, #20400, #14223, #39334, #26990, #33181, #17100, #8232, #32978, #20803, #26592, #4378, #5171, #26796, #29280, #1092, #11124, #23694, #1901, #20201, #32784, #14421, #13629, #10927, #36262 ),
 .UNSPECIFIED., .F., .F.,
 ( 4, 2, 2, 2, 2, 2, 2, 2, 2, 2, 2, 2, 2, 2, 2, 2, 2, 4 ),
 ( 0.02000509599350686063, 0.02121644006951485875, 0.02242778414552285687, 0.02363912822153085153, 0.02485047229753884965, 0.02606181637354684777, 0.02666748841155085897, 0.02727316044955487018, 0.02848450452556289259, 0.02909017656356688991, 0.02969584860157088724, 0.03090719267757885066, 0.03211853675358681409, 0.03454122490560271319, 0.03575256898161066621, 0.03696391305761861923, 0.03817525713362657225, 0.03938660120963451833 ),
 .UNSPECIFIED. ) ;
#8464 = ORIENTED_EDGE ( 'NONE', *, *, #27974, .F. ) ;
#8465 = DIRECTION ( 'NONE',  ( 0.000000000000000000, 0.000000000000000000, 1.000000000000000000 ) ) ;
#8466 = FACE_OUTER_BOUND ( 'NONE', #34624, .T. ) ;
#8467 = ORIENTED_EDGE ( 'NONE', *, *, #18169, .F. ) ;
#8468 = CARTESIAN_POINT ( 'NONE',  ( 23.14034614274038049, 4.027993350838696252, 3.114739222192818069 ) ) ;
#8469 = CARTESIAN_POINT ( 'NONE',  ( 81.35706873939176376, 65.93413826765579699, -1.145133701562419226 ) ) ;
#8470 = CARTESIAN_POINT ( 'NONE',  ( 78.65282594500106939, 66.03191569515874448, 1.205449537698852325 ) ) ;
#8471 = AXIS2_PLACEMENT_3D ( 'NONE', #33940, #15173, #5506 ) ;
#8472 = CARTESIAN_POINT ( 'NONE',  ( -0.1599037489455041594, -32.41586408544110043, 6.895222827070020877 ) ) ;
#8473 = ORIENTED_EDGE ( 'NONE', *, *, #16389, .T. ) ;
#8474 = CARTESIAN_POINT ( 'NONE',  ( 78.73442292448854118, 62.77418112150552787, -3.804514705604311597 ) ) ;
#8476 = CARTESIAN_POINT ( 'NONE',  ( 14.72888393404697638, -5.064079573351400576, -2.499999999997913669 ) ) ;
#8475 = CARTESIAN_POINT ( 'NONE',  ( 23.58567603336324225, 0.4095245276899994180, 5.530613567852399548 ) ) ;
#8477 = CARTESIAN_POINT ( 'NONE',  ( 79.82819440665738853, 65.73008711144039751, -2.710336141770836704 ) ) ;
#8478 = CARTESIAN_POINT ( 'NONE',  ( 80.27394690667868815, 60.98324426164374046, 1.908681007153611553 ) ) ;
#8479 = ORIENTED_EDGE ( 'NONE', *, *, #3817, .T. ) ;
#8480 = VERTEX_POINT ( 'NONE', #38207 ) ;
#8481 = CARTESIAN_POINT ( 'NONE',  ( 37.19747295490952155, -2.841588721108153415, -5.999818660317219887 ) ) ;
#8482 = ORIENTED_EDGE ( 'NONE', *, *, #25768, .T. ) ;
#8483 = CARTESIAN_POINT ( 'NONE',  ( 80.00335259508514696, 66.34466434620095754, 1.325417871280148985 ) ) ;
#8486 = ORIENTED_EDGE ( 'NONE', *, *, #25680, .F. ) ;
#8485 = CARTESIAN_POINT ( 'NONE',  ( 63.05383694556373797, -7.271989087314214117, 6.000000000000000000 ) ) ;
#8484 = CARTESIAN_POINT ( 'NONE',  ( 3.492838994194323643, -26.68078115845596443, 7.768425012602587998 ) ) ;
#8487 = CARTESIAN_POINT ( 'NONE',  ( 27.99192205930350497, 2.110044335382625924, -3.171593750069938711 ) ) ;
#8488 = CARTESIAN_POINT ( 'NONE',  ( -1.773393625443949073, -29.99752957843126566, 6.912143950357348743 ) ) ;
#8489 = CARTESIAN_POINT ( 'NONE',  ( -1.675359094926574866, -29.97529103330290212, 7.013842709614101167 ) ) ;
#8490 = CARTESIAN_POINT ( 'NONE',  ( -40.44874870218063734, -25.49307895267003587, 6.800000000000000711 ) ) ;
#8491 = CARTESIAN_POINT ( 'NONE',  ( 21.73475704421919374, 0.2471461942093770570, -9.024413037465413012 ) ) ;
#8492 = AXIS2_PLACEMENT_3D ( 'NONE', #6244, #275, #12413 ) ;
#8493 = PLANE ( 'NONE',  #7712 ) ;
#8494 = DIRECTION ( 'NONE',  ( 0.9616058754224561245, -0.2744342186262704875, 0.000000000000000000 ) ) ;
#8495 = DIRECTION ( 'NONE',  ( -0.000000000000000000, -0.000000000000000000, 1.000000000000000000 ) ) ;
#8496 = CARTESIAN_POINT ( 'NONE',  ( -71.80166262301922586, -0.2784082907551633790, 3.936323582618165950 ) ) ;
#8497 = CARTESIAN_POINT ( 'NONE',  ( 36.88745072424094218, -3.349843832818609979, -5.911037807513603859 ) ) ;
#8498 = CARTESIAN_POINT ( 'NONE',  ( 3.461020435952258278, -32.59486115124590100, 7.756742906098587298 ) ) ;
#8499 = CARTESIAN_POINT ( 'NONE',  ( 1.144867377203080405, -32.92424005792490505, 7.680992449362117114 ) ) ;
#8500 = CARTESIAN_POINT ( 'NONE',  ( 5.042305363714541855, -28.94414881188822619, 7.693875151218753317 ) ) ;
#8501 = CARTESIAN_POINT ( 'NONE',  ( 1.751251297819361730, -26.64985754041175525, 6.700000000000000178 ) ) ;
#8502 = DIRECTION ( 'NONE',  ( 1.000000000000000000, -0.000000000000000000, -0.000000000000000000 ) ) ;
#8503 = CARTESIAN_POINT ( 'NONE',  ( 4.626783558469344193, -27.83897054012538064, 7.691066658568949777 ) ) ;
#8504 = CARTESIAN_POINT ( 'NONE',  ( 3.551251297819357777, -26.64985754041175525, 6.700000000000000178 ) ) ;
#8505 = CARTESIAN_POINT ( 'NONE',  ( 23.79294960832602257, 1.583767941604382390, -4.781311079654926743 ) ) ;
#8506 = AXIS2_PLACEMENT_3D ( 'NONE', #23861, #8209, #39721 ) ;
#8507 = EDGE_CURVE ( 'NONE', #1678, #12553, #38128, .T. ) ;
#8508 = CARTESIAN_POINT ( 'NONE',  ( 2.214914452921659560, -33.03191941985759428, 6.863805608295729499 ) ) ;
#8509 = ORIENTED_EDGE ( 'NONE', *, *, #35184, .F. ) ;
#8510 =( BOUNDED_CURVE ( )  B_SPLINE_CURVE ( 3, ( #20927, #33513, #6723, #38394 ),
 .UNSPECIFIED., .F., .F. ) 
 B_SPLINE_CURVE_WITH_KNOTS ( ( 4, 4 ),
 ( 4.748221474220558846, 4.941946782021393147 ),
 .UNSPECIFIED. ) 
 CURVE ( )  GEOMETRIC_REPRESENTATION_ITEM ( )  RATIONAL_B_SPLINE_CURVE ( ( 1.000000000000000000, 0.9968749865767494445, 0.9968749865767494445, 1.000000000000000000 ) ) 
 REPRESENTATION_ITEM ( '' )  );
#8511 = CARTESIAN_POINT ( 'NONE',  ( 66.27376694608996388, 57.73522568913447373, 4.000000000000000000 ) ) ;
#8512 = CARTESIAN_POINT ( 'NONE',  ( 69.07430361466936120, 59.13263628650475567, -3.969490915146614007 ) ) ;
#8513 = CARTESIAN_POINT ( 'NONE',  ( 4.141053437885626742, -27.19263799006747462, 7.505001789837625559 ) ) ;
#8514 = ORIENTED_EDGE ( 'NONE', *, *, #25204, .F. ) ;
#8515 = DIRECTION ( 'NONE',  ( -0.000000000000000000, -0.000000000000000000, -1.000000000000000000 ) ) ;
#8516 = DIRECTION ( 'NONE',  ( -0.000000000000000000, -0.000000000000000000, 1.000000000000000000 ) ) ;
#8517 = CARTESIAN_POINT ( 'NONE',  ( 2.916291037025561916, -26.39477902244301433, 6.887041543973313473 ) ) ;
#8519 = CARTESIAN_POINT ( 'NONE',  ( 1.253764766991059432, -26.19939227113678015, 6.868387053540519815 ) ) ;
#8518 = FACE_OUTER_BOUND ( 'NONE', #34853, .T. ) ;
#8520 = CARTESIAN_POINT ( 'NONE',  ( -16.27783086239806210, 25.90100547710869705, 2.500000000000000000 ) ) ;
#8521 = ORIENTED_EDGE ( 'NONE', *, *, #29248, .F. ) ;
#8522 = CARTESIAN_POINT ( 'NONE',  ( 28.52663967383706023, 50.14399159706753295, -4.000000000000000000 ) ) ;
#8523 = CIRCLE ( 'NONE', #36142, 4.250000000000000000 ) ;
#8524 = LINE ( 'NONE', #12230, #8371 ) ;
#8525 = ORIENTED_EDGE ( 'NONE', *, *, #34074, .F. ) ;
#8526 = VERTEX_POINT ( 'NONE', #19285 ) ;
#8527 = CARTESIAN_POINT ( 'NONE',  ( 78.56734957671525876, 65.55328818492539256, -2.456741006817813044 ) ) ;
#8528 = CARTESIAN_POINT ( 'NONE',  ( 15.87703798546623801, 7.971370176595764079, -3.484773916741099153 ) ) ;
#8529 = CARTESIAN_POINT ( 'NONE',  ( 81.81391746733736170, 63.52311930392504280, -2.869341960395655811 ) ) ;
#8530 = EDGE_CURVE ( 'NONE', #19906, #26819, #8523, .T. ) ;
#8531 = CARTESIAN_POINT ( 'NONE',  ( 79.12445352002978893, 64.93440905817641351, 3.301258712451524246 ) ) ;
#8532 = ORIENTED_EDGE ( 'NONE', *, *, #27516, .F. ) ;
#8533 = PLANE ( 'NONE',  #33059 ) ;
#8534 = AXIS2_PLACEMENT_3D ( 'NONE', #37772, #13274, #35336 ) ;
#8535 = CARTESIAN_POINT ( 'NONE',  ( 8.290806648384990041, -33.63722727088462250, 27.90461065042423527 ) ) ;
#8536 = EDGE_CURVE ( 'NONE', #25105, #21404, #38101, .T. ) ;
#8537 = CARTESIAN_POINT ( 'NONE',  ( 21.85643539959774273, 10.54442680926682208, -0.8960936389291185300 ) ) ;
#8538 = ORIENTED_EDGE ( 'NONE', *, *, #39487, .T. ) ;
#8539 = CARTESIAN_POINT ( 'NONE',  ( -71.92837670882106238, -42.87473357531881391, 1.732050807568877637 ) ) ;
#8540 = EDGE_CURVE ( 'NONE', #39825, #5317, #6930, .T. ) ;
#8541 = CARTESIAN_POINT ( 'NONE',  ( -16.97867591359219475, -24.55319635012989110, 6.800000000000000711 ) ) ;
#8542 = CARTESIAN_POINT ( 'NONE',  ( -76.33197261733621986, 9.105972672263392909, -8.440813136491913227 ) ) ;
#8543 = DIRECTION ( 'NONE',  ( 1.000000000000000000, 0.000000000000000000, 0.000000000000000000 ) ) ;
#8544 = CARTESIAN_POINT ( 'NONE',  ( 2.490483471607719324, -26.26300413327467353, 6.920489980334478375 ) ) ;
#8545 = B_SPLINE_CURVE_WITH_KNOTS ( 'NONE', 5,
 ( #2779, #40618, #90, #31373, #15511, #37529, #27857, #24786 ),
 .UNSPECIFIED., .F., .F.,
 ( 6, 2, 6 ),
 ( 0.000000000000000000, 0.5000000000000000000, 1.000000000000000000 ),
 .UNSPECIFIED. ) ;
#8546 = CARTESIAN_POINT ( 'NONE',  ( 4.905277512680163987, -30.70513793031458505, 7.661510568013099487 ) ) ;
#8547 = CARTESIAN_POINT ( 'NONE',  ( 14.82857513895052293, 12.56830691318596038, 2.515104768166851468 ) ) ;
#8548 = CARTESIAN_POINT ( 'NONE',  ( -80.92837670882107659, 2.429809908903242555, 12.50000000000000000 ) ) ;
#8549 = LINE ( 'NONE', #11625, #24727 ) ;
#8550 = CARTESIAN_POINT ( 'NONE',  ( 5.055464264941726071, -29.01895665644428135, 7.784838882742139532 ) ) ;
#8551 = CARTESIAN_POINT ( 'NONE',  ( -69.92837670882107659, -0.7829914368874778541, 3.916079783099621014 ) ) ;
#8552 = DIRECTION ( 'NONE',  ( -0.000000000000000000, -0.000000000000000000, 1.000000000000000000 ) ) ;
#8553 = CARTESIAN_POINT ( 'NONE',  ( 4.165061536218790827, -31.91202212824329720, 6.959317978105167057 ) ) ;
#8554 = ADVANCED_FACE ( 'NONE', ( #30947 ), #17184, .F. ) ;
#8555 = VERTEX_POINT ( 'NONE', #15276 ) ;
#8556 = CARTESIAN_POINT ( 'NONE',  ( 67.72966869545554403, 58.29280778740498192, 3.997461085607385556 ) ) ;
#8557 = CARTESIAN_POINT ( 'NONE',  ( 2.298492929235983695, -33.01280978164516000, 7.773839561854631874 ) ) ;
#8558 = CARTESIAN_POINT ( 'NONE',  ( 85.16823716249373888, 2.433965874742513247, 4.055466505201608562 ) ) ;
#8559 = CIRCLE ( 'NONE', #23705, 0.1000000000000028644 ) ;
#8561 = DIRECTION ( 'NONE',  ( 1.000000000000000000, 0.000000000000000000, 0.000000000000000000 ) ) ;
#8560 = CARTESIAN_POINT ( 'NONE',  ( -71.92837670882107659, -20.91528738869522286, 5.916079783099629452 ) ) ;
#8562 = FACE_OUTER_BOUND ( 'NONE', #30996, .T. ) ;
#8563 = DIRECTION ( 'NONE',  ( 1.000000000000000000, 0.000000000000000000, -0.000000000000000000 ) ) ;
#8564 = CARTESIAN_POINT ( 'NONE',  ( 86.41986477775893150, 1.286830744106879143, 5.024081974984663468 ) ) ;
#8565 = CARTESIAN_POINT ( 'NONE',  ( -70.42514326790677615, -21.65690572916051693, 5.980075040747969695 ) ) ;
#8566 = EDGE_CURVE ( 'NONE', #22017, #32517, #2943, .T. ) ;
#8567 = ORIENTED_EDGE ( 'NONE', *, *, #15859, .T. ) ;
#8568 = CARTESIAN_POINT ( 'NONE',  ( -70.70940173728274658, -21.76495738335424690, 6.009053033063224802 ) ) ;
#8569 = UNCERTAINTY_MEASURE_WITH_UNIT (LENGTH_MEASURE( 1.000000000000000082E-05 ), #1067, 'distance_accuracy_value', 'NONE');
#8570 = EDGE_CURVE ( 'NONE', #23332, #27757, #40379, .T. ) ;
#8571 = ORIENTED_EDGE ( 'NONE', *, *, #624, .F. ) ;
#8572 = CARTESIAN_POINT ( 'NONE',  ( 78.72772338417257743, 65.90741647005499715, -1.973779052376060328 ) ) ;
#8573 = CARTESIAN_POINT ( 'NONE',  ( -1.575827083862257005, -28.33849528819893848, 6.888594555015732368 ) ) ;
#8574 = CARTESIAN_POINT ( 'NONE',  ( 78.62745313524290225, 65.95871297147078849, 1.682919622592493614 ) ) ;
#8575 = CARTESIAN_POINT ( 'NONE',  ( 25.90465186428314581, 0.9472713440299531662, 4.432119623292119392 ) ) ;
#8577 = ORIENTED_EDGE ( 'NONE', *, *, #10590, .T. ) ;
#8576 = DIRECTION ( 'NONE',  ( -0.9848077530122011369, -0.1736481776669699106, 0.000000000000000000 ) ) ;
#8578 = VECTOR ( 'NONE', #15250, 1000.000000000000114 ) ;
#8579 = CARTESIAN_POINT ( 'NONE',  ( 73.56486102181378328, 61.25343517167133456, -3.876585409328608289 ) ) ;
#8580 = CARTESIAN_POINT ( 'NONE',  ( 3.241318133241683608, -32.60070661927110081, 6.887945620086120435 ) ) ;
#8582 = FACE_OUTER_BOUND ( 'NONE', #4411, .T. ) ;
#8581 = DIRECTION ( 'NONE',  ( -0.000000000000000000, -0.000000000000000000, 1.000000000000000000 ) ) ;
#8583 = FACE_OUTER_BOUND ( 'NONE', #9438, .T. ) ;
#8584 = ADVANCED_FACE ( 'NONE', ( #4651 ), #23380, .F. ) ;
#8585 = EDGE_CURVE ( 'NONE', #614, #39861, #14098, .T. ) ;
#8586 = LINE ( 'NONE', #9350, #31786 ) ;
#8587 = CARTESIAN_POINT ( 'NONE',  ( 22.66364520782453340, 4.448174091865554125, -3.201175655495145378 ) ) ;
#8588 = EDGE_LOOP ( 'NONE', ( #29598, #30625, #38658 ) ) ;
#8589 = CARTESIAN_POINT ( 'NONE',  ( 5.199026221951053017, -29.68274962007452444, 7.076385936538754251 ) ) ;
#8590 = EDGE_CURVE ( 'NONE', #15868, #27566, #28256, .T. ) ;
#8591 = CIRCLE ( 'NONE', #21785, 0.1000000000000028644 ) ;
#8592 = CARTESIAN_POINT ( 'NONE',  ( 22.53035139435667844, 7.500704155568330478, 2.500000000000002220 ) ) ;
#8593 = CARTESIAN_POINT ( 'NONE',  ( 4.976842733950424424, -28.33913446795707358, 7.686927408461905920 ) ) ;
#8594 = CARTESIAN_POINT ( 'NONE',  ( 81.43301797337210246, 62.09285590259239740, 2.578835243349299144 ) ) ;
#8595 = CARTESIAN_POINT ( 'NONE',  ( 87.73660070961769009, -1.594395026316068220, -4.241058185374163791 ) ) ;
#8596 = LINE ( 'NONE', #27948, #18067 ) ;
#8597 = ORIENTED_EDGE ( 'NONE', *, *, #24404, .F. ) ;
#8598 = DIRECTION ( 'NONE',  ( -0.000000000000000000, -0.000000000000000000, -1.000000000000000000 ) ) ;
#8599 = CARTESIAN_POINT ( 'NONE',  ( 4.081262659518896108, -27.00449731093159045, 7.006908160621414083 ) ) ;
#8600 = CARTESIAN_POINT ( 'NONE',  ( 14.77855825630049225, -5.586149576324408450, -2.503853264347463803 ) ) ;
#8601 = DIRECTION ( 'NONE',  ( -0.000000000000000000, 1.000000000000000000, -0.000000000000000000 ) ) ;
#8602 = CARTESIAN_POINT ( 'NONE',  ( -2.515717719208200531, -28.88150288888238393, 7.695279973900954751 ) ) ;
#8603 = CARTESIAN_POINT ( 'NONE',  ( 1.899603570617604653, -26.17576915092285361, 6.997764925645181933 ) ) ;
#8604 = ORIENTED_EDGE ( 'NONE', *, *, #32103, .T. ) ;
#8605 = CARTESIAN_POINT ( 'NONE',  ( 2.851715340239886487, -32.85991820161709143, 7.785096263473212375 ) ) ;
#8606 = AXIS2_PLACEMENT_3D ( 'NONE', #34871, #72, #30754 ) ;
#8607 = CARTESIAN_POINT ( 'NONE',  ( 85.75774791330482572, 2.030551832223961295, -3.840166728450957301 ) ) ;
#8608 = ORIENTED_EDGE ( 'NONE', *, *, #14333, .F. ) ;
#8609 = ORIENTED_EDGE ( 'NONE', *, *, #34789, .T. ) ;
#8611 = CARTESIAN_POINT ( 'NONE',  ( 21.74038206013705121, 4.236694097800127068, 2.795633394849727615 ) ) ;
#8610 = CARTESIAN_POINT ( 'NONE',  ( 80.49267809498161341, 64.35807816991642483, -3.549391953833855862 ) ) ;
#8612 = CARTESIAN_POINT ( 'NONE',  ( 17.88044828116697005, -3.178183975948303264, -2.955689043506722236 ) ) ;
#8613 = CARTESIAN_POINT ( 'NONE',  ( 14.65885757255328414, 12.91887598178976937, -2.499999999999998668 ) ) ;
#8614 = ORIENTED_EDGE ( 'NONE', *, *, #3330, .F. ) ;
#8615 = CARTESIAN_POINT ( 'NONE',  ( 3.431434570054124222, -32.49627346798381211, 7.695279973900954751 ) ) ;
#8616 = ORIENTED_EDGE ( 'NONE', *, *, #8216, .T. ) ;
#8617 = ORIENTED_EDGE ( 'NONE', *, *, #1421, .T. ) ;
#8618 = DIRECTION ( 'NONE',  ( 0.6427876096865379196, 0.7660444431189792347, -0.000000000000000000 ) ) ;
#8619 = CARTESIAN_POINT ( 'NONE',  ( 79.66028364141931206, 64.99138685963065143, -3.354617312347329960 ) ) ;
#8620 = B_SPLINE_CURVE_WITH_KNOTS ( 'NONE', 3,
 ( #10462, #19338, #16439, #28814, #13160, #19548, #29015, #29214, #19934, #35413, #38065, #13350, #12955, #3518, #1023, #16041, #32317, #35210, #22644, #3720, #819, #16244, #28608, #19741, #26131, #25925, #416, #13556, #38662, #7181, #22841 ),
 .UNSPECIFIED., .F., .F.,
 ( 4, 3, 3, 3, 3, 3, 3, 3, 3, 3, 4 ),
 ( 1.939479807224432123E-18, 2.999644130997966760E-05, 6.002588995695383646E-05, 8.960886084588199122E-05, 0.0001190604700446493640, 0.0001489538463052688202, 0.0001796139255493963912, 0.0002109707048517053167, 0.0002426195318110302337, 0.0002740640997889996788, 0.0002849778069099796491 ),
 .UNSPECIFIED. ) ;
#8621 = CARTESIAN_POINT ( 'NONE',  ( -58.78362175692702607, 29.48419490076549465, -5.741263644839468938 ) ) ;
#8622 = VERTEX_POINT ( 'NONE', #36346 ) ;
#8624 = CARTESIAN_POINT ( 'NONE',  ( 4.372888262200486764, -27.46807179431958446, 7.768425012602593327 ) ) ;
#8623 = CARTESIAN_POINT ( 'NONE',  ( 23.47273670061042594, 2.435374625252711756, 4.369794992912356513 ) ) ;
#8625 = ORIENTED_EDGE ( 'NONE', *, *, #37467, .T. ) ;
#8626 = ADVANCED_FACE ( 'NONE', ( #35948 ), #26677, .F. ) ;
#8627 = CARTESIAN_POINT ( 'NONE',  ( 82.29984285855074688, 63.07754316838579456, -2.094266784919526447 ) ) ;
#8628 = EDGE_CURVE ( 'NONE', #13813, #36848, #17067, .T. ) ;
#8629 = CARTESIAN_POINT ( 'NONE',  ( -71.90221545680498139, -21.04534801433412028, 3.920659437232132394 ) ) ;
#8630 = VERTEX_POINT ( 'NONE', #23584 ) ;
#8631 =( BOUNDED_CURVE ( )  B_SPLINE_CURVE ( 3, ( #39895, #27335, #18057, #2460 ),
 .UNSPECIFIED., .F., .T. ) 
 B_SPLINE_CURVE_WITH_KNOTS ( ( 4, 4 ),
 ( 4.708531083176467291, 4.895802057644189631 ),
 .UNSPECIFIED. ) 
 CURVE ( )  GEOMETRIC_REPRESENTATION_ITEM ( )  RATIONAL_B_SPLINE_CURVE ( ( 1.000000000000000000, 0.9970795998553221295, 0.9970795998553221295, 1.000000000000000000 ) ) 
 REPRESENTATION_ITEM ( '' )  );
#8633 = CARTESIAN_POINT ( 'NONE',  ( 1.074608721727911442, -26.22801491291194864, 7.695279973900954751 ) ) ;
#8632 = DIRECTION ( 'NONE',  ( 1.000000000000000000, 0.000000000000000000, 0.000000000000000000 ) ) ;
#8634 = DIRECTION ( 'NONE',  ( -0.000000000000000000, -0.000000000000000000, -1.000000000000000000 ) ) ;
#8635 = CARTESIAN_POINT ( 'NONE',  ( 73.74018914705078487, 60.85874216252894087, 3.935025356190109402 ) ) ;
#8636 = ORIENTED_EDGE ( 'NONE', *, *, #28164, .F. ) ;
#8637 = CARTESIAN_POINT ( 'NONE',  ( 23.51549670196803632, 2.969767605084016715, -3.961303977705219914 ) ) ;
#8638 = ORIENTED_EDGE ( 'NONE', *, *, #6339, .T. ) ;
#8639 = EDGE_CURVE ( 'NONE', #9863, #37348, #9970, .T. ) ;
#8640 = CARTESIAN_POINT ( 'NONE',  ( 21.85643539959775694, 5.983772091205654675, 13.40455955530236487 ) ) ;
#8641 = PLANE ( 'NONE',  #25633 ) ;
#8642 = ORIENTED_EDGE ( 'NONE', *, *, #24250, .F. ) ;
#8643 = DIRECTION ( 'NONE',  ( 1.000000000000000000, 1.682730792515357087E-16, -0.000000000000000000 ) ) ;
#8644 = CARTESIAN_POINT ( 'NONE',  ( 81.98137654593483603, 62.63634409986677554, 2.334361474588996899 ) ) ;
#8645 = CARTESIAN_POINT ( 'NONE',  ( 86.49834695356116754, 1.198675839257056230, 5.248227958817050620 ) ) ;
#8646 = CARTESIAN_POINT ( 'NONE',  ( -61.57369240569498459, -49.47615685354814019, -3.769463484964756361 ) ) ;
#8647 = DIRECTION ( 'NONE',  ( 0.000000000000000000, 0.000000000000000000, 1.000000000000000000 ) ) ;
#8648 = CARTESIAN_POINT ( 'NONE',  ( -64.08758708074093136, 38.55573457772739943, 2.999999999999998668 ) ) ;
#8649 = CARTESIAN_POINT ( 'NONE',  ( 15.62809155304131004, -3.765067253224523736, 2.629774229783644834 ) ) ;
#8650 = CARTESIAN_POINT ( 'NONE',  ( 3.481437286441587897, -32.58288071328335178, 7.695279973900954751 ) ) ;
#8651 = CARTESIAN_POINT ( 'NONE',  ( 33.68680002607173662, -3.106704734317021099, -5.464037881042599132 ) ) ;
#8652 = SURFACE_STYLE_FILL_AREA ( #24096 ) ;
#8653 = CARTESIAN_POINT ( 'NONE',  ( 4.634237190056025746, -31.47847444865518085, 6.921725064902947366 ) ) ;
#8654 = DIRECTION ( 'NONE',  ( 0.000000000000000000, 0.000000000000000000, 1.000000000000000000 ) ) ;
#8655 = CARTESIAN_POINT ( 'NONE',  ( 4.304703044124503108, -31.90695999378015557, 7.761113333117553026 ) ) ;
#8656 = CARTESIAN_POINT ( 'NONE',  ( 1.735671467128618861, -33.06975260603037725, 7.707984471951054850 ) ) ;
#8657 = EDGE_LOOP ( 'NONE', ( #40116, #7631, #35354, #22525 ) ) ;
#8658 = CARTESIAN_POINT ( 'NONE',  ( 37.19501073558123494, -2.749265500231607096, 6.000935497143758290 ) ) ;
#8659 = CARTESIAN_POINT ( 'NONE',  ( -71.62860729996657483, -0.06907469158448548141, 3.958999674376896039 ) ) ;
#8660 = CARTESIAN_POINT ( 'NONE',  ( 66.85348068378573316, 57.96691244536589238, -3.999524142431097218 ) ) ;
#8661 = CARTESIAN_POINT ( 'NONE',  ( -66.99872204295122913, 28.48507918597134037, -12.49999999999999645 ) ) ;
#8662 = CYLINDRICAL_SURFACE ( 'NONE', #8214, 0.09010775117052882699 ) ;
#8663 = ORIENTED_EDGE ( 'NONE', *, *, #12031, .T. ) ;
#8664 = CARTESIAN_POINT ( 'NONE',  ( 1.700390093233090871, -29.56993018339339940, 7.800000000000000711 ) ) ;
#8665 = CARTESIAN_POINT ( 'NONE',  ( -72.01455954249333047, 4.687226239598052402, -9.941142508676179546 ) ) ;
#8666 = CARTESIAN_POINT ( 'NONE',  ( -71.92837670882107659, -20.78299143688747819, 5.916079783099621459 ) ) ;
#8667 = DIRECTION ( 'NONE',  ( -0.000000000000000000, -0.000000000000000000, -1.000000000000000000 ) ) ;
#8668 = EDGE_LOOP ( 'NONE', ( #8936, #10975, #28700, #6191 ) ) ;
#8669 = CARTESIAN_POINT ( 'NONE',  ( -1.146144745493847150, -27.71056485836612637, 7.013842709614101167 ) ) ;
#8670 = CARTESIAN_POINT ( 'NONE',  ( -1.699609906766908818, -29.56898895464481569, 7.768009089657827104 ) ) ;
#8671 = ORIENTED_EDGE ( 'NONE', *, *, #39224, .T. ) ;
#8672 = CARTESIAN_POINT ( 'NONE',  ( 23.42902919107597981, 3.774424825821157459, 3.149840774630959128 ) ) ;
#8673 = CARTESIAN_POINT ( 'NONE',  ( 80.03496335128151884, 66.36160760684386162, -1.000000000000000000 ) ) ;
#8674 = CARTESIAN_POINT ( 'NONE',  ( 81.15742489870845588, 61.60174059333854757, 2.174925636353720382 ) ) ;
#8675 = CARTESIAN_POINT ( 'NONE',  ( 1.551251297819356001, -26.64985754041175525, 6.700000000000000178 ) ) ;
#8676 = ORIENTED_EDGE ( 'NONE', *, *, #39358, .T. ) ;
#8677 = CARTESIAN_POINT ( 'NONE',  ( 78.85022303194006099, 62.54057813906803176, -3.766285651913924060 ) ) ;
#8679 = CARTESIAN_POINT ( 'NONE',  ( 14.70693164707954459, -5.039500861583466218, -2.499999999999853895 ) ) ;
#8678 = CARTESIAN_POINT ( 'NONE',  ( 24.12053105157879784, 0.4789250373359598689, 5.097972069152276298 ) ) ;
#8680 = CARTESIAN_POINT ( 'NONE',  ( 81.41366110773520859, 61.69541933536140732, -2.011547652602695191 ) ) ;
#8681 = CARTESIAN_POINT ( 'NONE',  ( 80.07249602437107683, 61.49066053983646185, 2.889371261047465556 ) ) ;
#8682 = VECTOR ( 'NONE', #22919, 1000.000000000000000 ) ;
#8683 = EDGE_LOOP ( 'NONE', ( #14398, #27571, #13564, #4938, #27874 ) ) ;
#8684 = EDGE_CURVE ( 'NONE', #18532, #8010, #22112, .T. ) ;
#8685 = EDGE_CURVE ( 'NONE', #38217, #21520, #5246, .T. ) ;
#8686 = CARTESIAN_POINT ( 'NONE',  ( 36.15253105956762170, -3.657967514016432720, -5.706993152568901273 ) ) ;
#8687 = ADVANCED_FACE ( 'NONE', ( #19759 ), #25741, .F. ) ;
#8688 = AXIS2_PLACEMENT_3D ( 'NONE', #12217, #9532, #22116 ) ;
#8689 = CARTESIAN_POINT ( 'NONE',  ( 78.69020857030076854, 66.05846869611056604, 1.014334479594652283 ) ) ;
#8691 = CARTESIAN_POINT ( 'NONE',  ( -1.694803313432552416, -29.38902479350574382, 6.887945620086119547 ) ) ;
#8690 = DIRECTION ( 'NONE',  ( 0.000000000000000000, 1.000000000000000000, 0.000000000000000000 ) ) ;
#8692 = CARTESIAN_POINT ( 'NONE',  ( 29.60575365153160732, -0.8332953136462766253, 6.005451346670388268 ) ) ;
#8693 = CARTESIAN_POINT ( 'NONE',  ( -1.761599143231102671, -30.08445454308195721, 6.863805608295729499 ) ) ;
#8694 = CYLINDRICAL_SURFACE ( 'NONE', #8805, 0.1000000000000028644 ) ;
#8695 = CARTESIAN_POINT ( 'NONE',  ( -80.88216618113609968, -5.699911949738533323, 1.044490278467241184 ) ) ;
#8696 = CARTESIAN_POINT ( 'NONE',  ( 21.73453909374078563, 0.2390742653956647312, -9.045263263313582769 ) ) ;
#8697 = CARTESIAN_POINT ( 'NONE',  ( -62.86576508122317364, 38.67912974266874926, 6.999999999999999112 ) ) ;
#8698 = DIRECTION ( 'NONE',  ( 0.7394003126383942304, -0.1303762246624207699, 0.6605219282605376829 ) ) ;
#8699 = CARTESIAN_POINT ( 'NONE',  ( -1.694464052375517671, -29.38293999636734810, 7.013842709614101167 ) ) ;
#8700 = DIRECTION ( 'NONE',  ( 1.000000000000000000, 0.000000000000000000, 0.000000000000000000 ) ) ;
#8701 = CARTESIAN_POINT ( 'NONE',  ( 30.84892909652827697, 0.6455663479207958133, -4.592247333245458307 ) ) ;
#8702 = CARTESIAN_POINT ( 'NONE',  ( 3.371024467839934147, -32.63382312644299077, 7.780491323090173772 ) ) ;
#8703 = CARTESIAN_POINT ( 'NONE',  ( 27.14650909609752816, 1.283972158900671623, -4.437200329386957520 ) ) ;
#8704 = CARTESIAN_POINT ( 'NONE',  ( -1.699609906766908818, -29.56993018339339940, 6.949309202340325342 ) ) ;
#8706 = DIRECTION ( 'NONE',  ( 0.5000000000000072164, -0.8660254037844344888, 0.000000000000000000 ) ) ;
#8705 = B_SPLINE_CURVE_WITH_KNOTS ( 'NONE', 3,
 ( #32355, #23277, #16667, #13598, #38702, #23081 ),
 .UNSPECIFIED., .F., .F.,
 ( 4, 2, 4 ),
 ( 4.336808689942017255E-19, 0.001065454728147860767, 0.002130909456295721101 ),
 .UNSPECIFIED. ) ;
#8707 = CYLINDRICAL_SURFACE ( 'NONE', #360, 0.09010775117052928496 ) ;
#8708 = CARTESIAN_POINT ( 'NONE',  ( -75.54006495261842247, 8.454230440140586111, 10.26970949974186986 ) ) ;
#8709 = CARTESIAN_POINT ( 'NONE',  ( 4.934307971444643393, -28.52027331175976244, 7.757178535559533294 ) ) ;
#8710 = CARTESIAN_POINT ( 'NONE',  ( 17.97454669799173033, 51.66243977840390755, -4.000000000000000000 ) ) ;
#8711 = CARTESIAN_POINT ( 'NONE',  ( 23.12838916460015071, 1.463821817805705194, -5.240134305553244332 ) ) ;
#8712 = CARTESIAN_POINT ( 'NONE',  ( -1.522142227221405131, -30.65403601015855273, 6.870716933885662847 ) ) ;
#8713 = VERTEX_POINT ( 'NONE', #10677 ) ;
#8714 = CARTESIAN_POINT ( 'NONE',  ( -4.978675913592189417, -26.64985754041175525, 6.700000000000000178 ) ) ;
#8715 = CARTESIAN_POINT ( 'NONE',  ( 70.06771224146353916, 58.30163689823704942, -3.863726395435713723 ) ) ;
#8716 = CIRCLE ( 'NONE', #2191, 0.1000000000000028644 ) ;
#8717 = VERTEX_POINT ( 'NONE', #19952 ) ;
#8718 = CARTESIAN_POINT ( 'NONE',  ( 85.71231987865445490, 0.7872592507033150389, 5.912482239253596283 ) ) ;
#8719 = CARTESIAN_POINT ( 'NONE',  ( 1.822194502883806022, -33.27093018339341768, 7.754798119455333705 ) ) ;
#8720 = CARTESIAN_POINT ( 'NONE',  ( 69.87460780774588898, 58.79389746341001199, 3.972683913566375402 ) ) ;
#8721 = CARTESIAN_POINT ( 'NONE',  ( -69.92837670882107659, -20.78299143688747819, 5.916079783099621459 ) ) ;
#8723 = CARTESIAN_POINT ( 'NONE',  ( 4.881456320988373676, -30.77031019809703238, 7.784838882742139532 ) ) ;
#8722 = CARTESIAN_POINT ( 'NONE',  ( -0.8685330176923784506, -27.19282394888199050, 6.895394898881665569 ) ) ;
#8724 = CARTESIAN_POINT ( 'NONE',  ( 2.174739121882255599, -32.93667912707378775, 7.759451378593095860 ) ) ;
#8725 = ORIENTED_EDGE ( 'NONE', *, *, #25205, .T. ) ;
#8726 = CARTESIAN_POINT ( 'NONE',  ( 24.76601816127300637, 3.022843676862287499, 3.334302330152292271 ) ) ;
#8727 = SURFACE_STYLE_USAGE ( .BOTH. , #37146 ) ;
#8728 = ORIENTED_EDGE ( 'NONE', *, *, #27334, .F. ) ;
#8729 = CARTESIAN_POINT ( 'NONE',  ( 80.71160662450162704, 61.49558808705153012, -2.436540443961501268 ) ) ;
#8730 = CARTESIAN_POINT ( 'NONE',  ( 23.31126841323469989, 9.638235061640909151, -2.500000000000000444 ) ) ;
#8731 = CARTESIAN_POINT ( 'NONE',  ( 81.54961753534276170, 61.59690320141230302, -1.551099981298398767 ) ) ;
#8732 = B_SPLINE_CURVE_WITH_KNOTS ( 'NONE', 3,
 ( #26405, #29285, #26598, #1099, #23700, #23512, #26206, #29680, #39339, #17304 ),
 .UNSPECIFIED., .F., .F.,
 ( 4, 3, 3, 4 ),
 ( 0.0001585009270395812257, 0.0001815657551981893171, 0.0002118214035944172217, 0.0002170292169044841320 ),
 .UNSPECIFIED. ) ;
#8733 = CARTESIAN_POINT ( 'NONE',  ( 80.91727723835764152, 61.27046310099957793, 1.796258654642569841 ) ) ;
#8734 = CARTESIAN_POINT ( 'NONE',  ( -12.24874870218063627, -26.64985754041175525, 6.800000000000000711 ) ) ;
#8735 = ADVANCED_FACE ( 'NONE', ( #21895 ), #640, .F. ) ;
#8736 = CARTESIAN_POINT ( 'NONE',  ( 4.825889015811430482, -30.92609072608717824, 7.386948897581450346 ) ) ;
#8737 = CARTESIAN_POINT ( 'NONE',  ( 21.85643539959776760, 7.145415623174192987, -7.905327125498018859 ) ) ;
#8738 = VERTEX_POINT ( 'NONE', #38282 ) ;
#8739 = CARTESIAN_POINT ( 'NONE',  ( -79.86284581725708165, 10.49264010779607048, 4.509636572782145691 ) ) ;
#8740 = CARTESIAN_POINT ( 'NONE',  ( 2.357445652190597762, -33.01462870691901941, 7.255881584735164758 ) ) ;
#8741 = CARTESIAN_POINT ( 'NONE',  ( -69.92837670882107659, -20.78299143688747819, 5.916079783099617906 ) ) ;
#8742 = CARTESIAN_POINT ( 'NONE',  ( -73.23469688983234960, 4.928437080168684759, -9.790059002995628035 ) ) ;
#8743 = DIRECTION ( 'NONE',  ( 0.000000000000000000, 0.000000000000000000, 1.000000000000000000 ) ) ;
#8744 = CARTESIAN_POINT ( 'NONE',  ( 36.71952137777376635, -3.460392053857834327, -5.859972560675125841 ) ) ;
#8745 = CARTESIAN_POINT ( 'NONE',  ( 4.907453385184882499, -30.69897626116466682, 7.692469944509198854 ) ) ;
#8746 = CARTESIAN_POINT ( 'NONE',  ( 15.16058069087244853, 11.94051475997482648, 2.549013982532239098 ) ) ;
#8747 = CARTESIAN_POINT ( 'NONE',  ( 3.477237270422150139, -26.55450084266673727, 6.894806418505347700 ) ) ;
#8748 = CARTESIAN_POINT ( 'NONE',  ( 29.06645441453732559, -3.924731372528510676, 4.240759432255150507 ) ) ;
#8749 = CARTESIAN_POINT ( 'NONE',  ( 5.058692241207612739, -29.03907551127521103, 7.785172627573962778 ) ) ;
#8750 = CARTESIAN_POINT ( 'NONE',  ( -4.890026461918809630, -25.50263309590217276, -2.500000000000002220 ) ) ;
#8751 = AXIS2_PLACEMENT_3D ( 'NONE', #3295, #22215, #16016 ) ;
#8752 = DIRECTION ( 'NONE',  ( 0.000000000000000000, 0.000000000000000000, 1.000000000000000000 ) ) ;
#8753 = CARTESIAN_POINT ( 'NONE',  ( 1.126346108378571076, -33.02253567017740465, 7.674970859709602244 ) ) ;
#8754 = CARTESIAN_POINT ( 'NONE',  ( 24.77204021038152959, 2.610204331802961963, -3.937606257336461635 ) ) ;
#8755 = ORIENTED_EDGE ( 'NONE', *, *, #22243, .F. ) ;
#8756 = CARTESIAN_POINT ( 'NONE',  ( -69.50551526817780257, -47.60185046458123281, 5.828975448080927713 ) ) ;
#8757 = CARTESIAN_POINT ( 'NONE',  ( 67.13660786288076565, 58.10023080654656980, 3.998533043703386802 ) ) ;
#8758 = EDGE_CURVE ( 'NONE', #2006, #16194, #10269, .T. ) ;
#8759 = CARTESIAN_POINT ( 'NONE',  ( 0.2633542768278205881, -25.48582225135028878, 6.954324564059724878 ) ) ;
#8760 = AXIS2_PLACEMENT_3D ( 'NONE', #5505, #27935, #40478 ) ;
#8761 = CARTESIAN_POINT ( 'NONE',  ( 88.42327724305060599, -1.151963697325209202, 3.685007885677881401 ) ) ;
#8763 = CARTESIAN_POINT ( 'NONE',  ( 33.60333658342298691, -1.218927361606251702, -5.451011392246272180 ) ) ;
#8762 = CARTESIAN_POINT ( 'NONE',  ( 29.20860690094596634, 2.240472738085125037, 1.050758983225395848 ) ) ;
#8764 = ORIENTED_EDGE ( 'NONE', *, *, #11281, .T. ) ;
#8765 = DIRECTION ( 'NONE',  ( 1.000000000000000000, 0.000000000000000000, 0.000000000000000000 ) ) ;
#8766 = CARTESIAN_POINT ( 'NONE',  ( 3.438683469850188690, -26.53211252316276259, 7.635761828346582014 ) ) ;
#8767 = ORIENTED_EDGE ( 'NONE', *, *, #3492, .F. ) ;
#8768 = CARTESIAN_POINT ( 'NONE',  ( -69.93541594206888590, -20.90143516061696616, 3.917265324091089518 ) ) ;
#8769 = ADVANCED_FACE ( 'NONE', ( #39902 ), #39285, .F. ) ;
#8770 = VERTEX_POINT ( 'NONE', #36410 ) ;
#8771 = CARTESIAN_POINT ( 'NONE',  ( 78.83217078968475278, 65.79276158749699732, -2.259810845157019354 ) ) ;
#8772 = CARTESIAN_POINT ( 'NONE',  ( 8.290806648384990041, -33.63722727088462250, 27.90461065042423527 ) ) ;
#8773 = CARTESIAN_POINT ( 'NONE',  ( 79.76446817951413948, 64.32424044856642809, 3.638935937159315515 ) ) ;
#8775 = ORIENTED_EDGE ( 'NONE', *, *, #3716, .F. ) ;
#8774 = DIRECTION ( 'NONE',  ( 0.000000000000000000, 0.000000000000000000, -1.000000000000000000 ) ) ;
#8776 = CARTESIAN_POINT ( 'NONE',  ( -75.45330471031414277, 33.71485196875532608, 21.52833696633422988 ) ) ;
#8777 = CARTESIAN_POINT ( 'NONE',  ( 74.49653936242856389, 60.69398666642196360, -3.911020515999844793 ) ) ;
#8778 = CARTESIAN_POINT ( 'NONE',  ( 3.235878913814441038, -32.60345520914638939, 7.013842709614101167 ) ) ;
#8779 = EDGE_CURVE ( 'NONE', #11908, #37911, #4717, .T. ) ;
#8781 = DIRECTION ( 'NONE',  ( 1.000000000000000000, 1.165409145176969993E-16, 0.000000000000000000 ) ) ;
#8780 = CARTESIAN_POINT ( 'NONE',  ( 4.651604549657131216, -31.25822317698004227, 7.635761828346577573 ) ) ;
#8782 = CARTESIAN_POINT ( 'NONE',  ( -4.248748702180636272, -26.64985754041175525, 6.700000000000000178 ) ) ;
#8783 = DIRECTION ( 'NONE',  ( -0.000000000000000000, -0.000000000000000000, -1.000000000000000000 ) ) ;
#8784 = CARTESIAN_POINT ( 'NONE',  ( 22.88660608767791160, 4.282592626049536833, -3.128843504308600920 ) ) ;
#8785 = VERTEX_POINT ( 'NONE', #2051 ) ;
#8786 = LINE ( 'NONE', #12079, #16286 ) ;
#8787 = AXIS2_PLACEMENT_3D ( 'NONE', #16922, #704, #32402 ) ;
#8788 = CARTESIAN_POINT ( 'NONE',  ( -0.9576111974470827848, -31.84699608905852131, 7.700536657684214248 ) ) ;
#8789 = CIRCLE ( 'NONE', #10762, 1.000000000000002220 ) ;
#8790 = CARTESIAN_POINT ( 'NONE',  ( 4.982636580400577664, -28.35466971852313733, 7.643192810543823157 ) ) ;
#8791 = CARTESIAN_POINT ( 'NONE',  ( 81.39159673219469937, 61.52361671445412128, 1.704083397384870358 ) ) ;
#8792 = CARTESIAN_POINT ( 'NONE',  ( 85.28131701390645958, 1.700283277630491030, -5.218886290300497777 ) ) ;
#8793 = DIRECTION ( 'NONE',  ( -0.000000000000000000, -0.000000000000000000, -1.000000000000000000 ) ) ;
#8794 = VERTEX_POINT ( 'NONE', #17251 ) ;
#8795 = DIRECTION ( 'NONE',  ( 0.8831583674551003460, -0.4690749385695657803, 0.000000000000000000 ) ) ;
#8796 = CARTESIAN_POINT ( 'NONE',  ( 4.662690227536056220, -31.23869556963216709, 7.703977250142846955 ) ) ;
#8798 = ADVANCED_FACE ( 'NONE', ( #20546 ), #33130, .F. ) ;
#8797 = EDGE_LOOP ( 'NONE', ( #30429, #12531, #2645, #1218, #22221 ) ) ;
#8799 = CARTESIAN_POINT ( 'NONE',  ( -68.98442902999595105, 21.93515443114010210, 12.49999999999999645 ) ) ;
#8800 = CARTESIAN_POINT ( 'NONE',  ( 26.27016240683699877, -3.098343122671453731, -4.267664985417156664 ) ) ;
#8801 = CARTESIAN_POINT ( 'NONE',  ( 35.45227351365613089, -1.918039355012105762, -5.739582716917785987 ) ) ;
#8802 = DIRECTION ( 'NONE',  ( 0.000000000000000000, -0.7126435865141261816, -0.7015262779114429526 ) ) ;
#8803 = CARTESIAN_POINT ( 'NONE',  ( 1.903485573815023146, -26.17600145318010973, 6.988553391373221402 ) ) ;
#8804 = CARTESIAN_POINT ( 'NONE',  ( 36.78876423199966439, -3.039631217886890724, 5.948174416665469089 ) ) ;
#8805 = AXIS2_PLACEMENT_3D ( 'NONE', #23935, #2144, #18166 ) ;
#8806 = CARTESIAN_POINT ( 'NONE',  ( 88.35060396620406209, -0.8818671507646100860, -0.7863509125847466530 ) ) ;
#8807 = ORIENTED_EDGE ( 'NONE', *, *, #6441, .F. ) ;
#8808 = ORIENTED_EDGE ( 'NONE', *, *, #29421, .F. ) ;
#8810 = CARTESIAN_POINT ( 'NONE',  ( 37.01095259801031290, -2.247694374308371046, 5.912577408341228136 ) ) ;
#8809 = CARTESIAN_POINT ( 'NONE',  ( 79.05590852586871620, 65.97304283769159383, -2.079311677127757108 ) ) ;
#8811 = EDGE_CURVE ( 'NONE', #8271, #21802, #18134, .T. ) ;
#8812 = EDGE_CURVE ( 'NONE', #36468, #22420, #1848, .T. ) ;
#8813 = CARTESIAN_POINT ( 'NONE',  ( 21.75262081531260350, -3.067555067785914691, -3.510010962324494610 ) ) ;
#8814 = CARTESIAN_POINT ( 'NONE',  ( 14.68773611677202773, 12.90757323259234823, -2.500000034696362672 ) ) ;
#8815 = ORIENTED_EDGE ( 'NONE', *, *, #25812, .F. ) ;
#8816 = ADVANCED_FACE ( 'NONE', ( #8394 ), #33344, .T. ) ;
#8817 = CARTESIAN_POINT ( 'NONE',  ( 0.9689046511080217083, -32.99263803653528271, 7.750000000000000888 ) ) ;
#8818 = CIRCLE ( 'NONE', #1616, 0.1000000000000028644 ) ;
#8819 = ORIENTED_EDGE ( 'NONE', *, *, #5963, .F. ) ;
#8820 = ORIENTED_EDGE ( 'NONE', *, *, #28455, .T. ) ;
#8821 = FACE_OUTER_BOUND ( 'NONE', #5646, .T. ) ;
#8822 = CARTESIAN_POINT ( 'NONE',  ( 80.77858121287650306, 63.01782502344087078, -3.459421039841290568 ) ) ;
#8823 = LINE ( 'NONE', #5757, #22777 ) ;
#8824 = ORIENTED_EDGE ( 'NONE', *, *, #20485, .F. ) ;
#8826 = CARTESIAN_POINT ( 'NONE',  ( 4.378905692300169683, -27.47575740248258569, 7.759451378593096749 ) ) ;
#8825 = CARTESIAN_POINT ( 'NONE',  ( 24.45417550923406935, 2.604819814871429884, 3.970987390700944086 ) ) ;
#8827 = EDGE_LOOP ( 'NONE', ( #29431, #36786, #2860, #19796 ) ) ;
#8828 = CARTESIAN_POINT ( 'NONE',  ( 81.63785901438869530, 61.64013749223433081, -1.421876342974254248 ) ) ;
#8829 = CARTESIAN_POINT ( 'NONE',  ( -2.954197855305039422, -12.43481156997016157, -1.000000000000000000 ) ) ;
#8830 = ADVANCED_FACE ( 'NONE', ( #20968 ), #30033, .F. ) ;
#8831 = VERTEX_POINT ( 'NONE', #39689 ) ;
#8832 = PRODUCT_DEFINITION_SHAPE ( 'NONE', 'NONE',  #40723 ) ;
#8834 = CARTESIAN_POINT ( 'NONE',  ( 85.15856829264210148, 2.703578820932674542, -0.6845625252714587772 ) ) ;
#8833 = CARTESIAN_POINT ( 'NONE',  ( 4.882903053830506934, -28.37343059892649677, 7.691066658568946224 ) ) ;
#8835 = DIRECTION ( 'NONE',  ( -0.000000000000000000, -0.000000000000000000, 1.000000000000000000 ) ) ;
#8836 = CARTESIAN_POINT ( 'NONE',  ( 74.68367562674023930, 60.27297886100710400, 3.815996826674382447 ) ) ;
#8837 = CARTESIAN_POINT ( 'NONE',  ( 23.91035688797384751, 2.995239222824085168, -3.797843349976805172 ) ) ;
#8838 = CIRCLE ( 'NONE', #39764, 0.1000000000000028644 ) ;
#8839 = CARTESIAN_POINT ( 'NONE',  ( 21.85643539959775694, 3.570402768353612810, -13.15459721397892423 ) ) ;
#8840 = VECTOR ( 'NONE', #4084, 1000.000000000000000 ) ;
#8841 = CARTESIAN_POINT ( 'NONE',  ( -22.34874870218063947, -26.64985754041175525, 6.700000000000000178 ) ) ;
#8842 = ORIENTED_EDGE ( 'NONE', *, *, #5864, .T. ) ;
#8843 = CARTESIAN_POINT ( 'NONE',  ( 3.357996495870312792, -32.53848892694827555, 6.894806418505347700 ) ) ;
#8844 = VERTEX_POINT ( 'NONE', #1442 ) ;
#8845 = CARTESIAN_POINT ( 'NONE',  ( 81.37441939350044606, 61.42019823254032218, 1.301239782962658964 ) ) ;
#8846 = CARTESIAN_POINT ( 'NONE',  ( 88.00102923632725549, -0.4892082223494365611, 4.076460784956554839 ) ) ;
#8847 = B_SPLINE_CURVE_WITH_KNOTS ( 'NONE', 3,
 ( #38831, #10026, #22410, #3686, #32285, #10625, #22609, #32087, #13736, #3892, #16407, #23200, #20101, #17001, #13924, #28982, #785, #13315, #25888 ),
 .UNSPECIFIED., .F., .F.,
 ( 4, 3, 3, 3, 3, 3, 4 ),
 ( 1.084202172485504434E-18, 2.546128104244520487E-05, 5.711050680483435320E-05, 8.113074941675352508E-05, 0.0001053129305727020908, 0.0001360598016347060505, 0.0001612931755702085880 ),
 .UNSPECIFIED. ) ;
#8848 = CARTESIAN_POINT ( 'NONE',  ( -4.890026461918807854, -25.50263309590217276, -6.000000000000001776 ) ) ;
#8849 = AXIS2_PLACEMENT_3D ( 'NONE', #38498, #31333, #3157 ) ;
#8850 = CARTESIAN_POINT ( 'NONE',  ( 2.477556199703359940, -25.36946941773652853, 7.695279973900954751 ) ) ;
#8851 = FACE_OUTER_BOUND ( 'NONE', #32897, .T. ) ;
#8852 = CARTESIAN_POINT ( 'NONE',  ( 21.53525890830123046, 7.395493054481637074, 0.9774100666432447015 ) ) ;
#8853 = CARTESIAN_POINT ( 'NONE',  ( 35.86956930648597108, -2.085467868944065550, -5.804711817725769940 ) ) ;
#8854 = CARTESIAN_POINT ( 'NONE',  ( 5.100341873444426355, -29.59048384115356711, 7.779495906702013741 ) ) ;
#8855 = CARTESIAN_POINT ( 'NONE',  ( 4.677559685796697231, -31.41019271375740374, 6.863784140767622333 ) ) ;
#8856 = CARTESIAN_POINT ( 'NONE',  ( -29.07867591359219617, -26.64985754041175525, 6.800000000000000711 ) ) ;
#8857 = EDGE_CURVE ( 'NONE', #6774, #29061, #24980, .T. ) ;
#8858 = CARTESIAN_POINT ( 'NONE',  ( -72.46964309959683703, 39.11862660440054640, 12.50000000000000000 ) ) ;
#8859 = CARTESIAN_POINT ( 'NONE',  ( 1.717829174068238984, -33.06988673718940674, 7.750000000000000888 ) ) ;
#8860 = EDGE_CURVE ( 'NONE', #2937, #5311, #17859, .T. ) ;
#8861 = ORIENTED_EDGE ( 'NONE', *, *, #20884, .T. ) ;
#8862 = CARTESIAN_POINT ( 'NONE',  ( 36.87708760085472903, -3.319687905980674536, 5.920000889922525822 ) ) ;
#8863 = LINE ( 'NONE', #28213, #19870 ) ;
#8864 = CARTESIAN_POINT ( 'NONE',  ( 66.99315907379003932, 58.03889713220680591, -3.999016414675010012 ) ) ;
#8865 = DIRECTION ( 'NONE',  ( 0.000000000000000000, 0.000000000000000000, 1.000000000000000000 ) ) ;
#8866 = EDGE_CURVE ( 'NONE', #774, #16334, #18384, .T. ) ;
#8867 = DIRECTION ( 'NONE',  ( 0.000000000000000000, -0.6662082868431821181, -0.7457657263118708801 ) ) ;
#8868 = CIRCLE ( 'NONE', #23374, 0.1000000000000028644 ) ;
#8869 = ORIENTED_EDGE ( 'NONE', *, *, #6850, .T. ) ;
#8870 = CIRCLE ( 'NONE', #388, 0.1000000000000028644 ) ;
#8871 = CARTESIAN_POINT ( 'NONE',  ( 4.666500650180242182, -31.42793668606411117, 7.750000000000000888 ) ) ;
#8872 = CARTESIAN_POINT ( 'NONE',  ( -75.29779855868427774, -5.030202623681788054, -9.000969684516388014 ) ) ;
#8873 = CARTESIAN_POINT ( 'NONE',  ( 15.84007060359406083, 10.41087468735547716, 2.678624129882808180 ) ) ;
#8874 = CIRCLE ( 'NONE', #5602, 7.999999999999986677 ) ;
#8875 = VERTEX_POINT ( 'NONE', #29824 ) ;
#8876 = DIRECTION ( 'NONE',  ( -1.000000000000000000, 0.000000000000000000, 0.000000000000000000 ) ) ;
#8877 = CARTESIAN_POINT ( 'NONE',  ( 5.029851253234809860, -28.49072197104846182, 7.751599049952172749 ) ) ;
#8878 = EDGE_LOOP ( 'NONE', ( #3088, #34509, #27256, #19959 ) ) ;
#8879 = CARTESIAN_POINT ( 'NONE',  ( 24.68756320289947936, 2.996584696271434201, 3.466125977230326782 ) ) ;
#8880 = CARTESIAN_POINT ( 'NONE',  ( 82.45631153319118312, 62.87735296625317005, -1.000000000000000000 ) ) ;
#8881 = CARTESIAN_POINT ( 'NONE',  ( 80.68955802291256418, 62.97990070207239199, 3.482375488376183270 ) ) ;
#8882 = CARTESIAN_POINT ( 'NONE',  ( -0.1645870765518833712, -32.41279934783806738, 7.006423389747792108 ) ) ;
#8883 = ORIENTED_EDGE ( 'NONE', *, *, #6993, .T. ) ;
#8884 = CARTESIAN_POINT ( 'NONE',  ( 76.72614680668752385, 63.26816225425363172, -3.643081266322632406 ) ) ;
#8886 = DIRECTION ( 'NONE',  ( 0.000000000000000000, 0.000000000000000000, 1.000000000000000000 ) ) ;
#8885 = CARTESIAN_POINT ( 'NONE',  ( 3.867374209161352994, -32.31247832666930719, 7.771081512783697853 ) ) ;
#8887 = CARTESIAN_POINT ( 'NONE',  ( 0.5037982502477853508, -26.38745190989316214, 7.695279973900954751 ) ) ;
#8888 = CARTESIAN_POINT ( 'NONE',  ( 79.40189760861154866, 66.01232247510107243, -2.246767365022174001 ) ) ;
#8889 = CARTESIAN_POINT ( 'NONE',  ( 78.71019189666364468, 60.57837954350641496, 2.701592190111063552 ) ) ;
#8890 = ORIENTED_EDGE ( 'NONE', *, *, #35540, .F. ) ;
#8891 = DIRECTION ( 'NONE',  ( 1.000000000000000000, 0.000000000000000000, 0.000000000000000000 ) ) ;
#8892 = CARTESIAN_POINT ( 'NONE',  ( 81.75239774439276630, 65.41456323740531786, 1.882325606868447299 ) ) ;
#8895 = ORIENTED_EDGE ( 'NONE', *, *, #37764, .F. ) ;
#8894 = CARTESIAN_POINT ( 'NONE',  ( 5.694018316346522113, -26.44898221431133578, 6.954324564059724878 ) ) ;
#8893 = CARTESIAN_POINT ( 'NONE',  ( -64.85784325972055342, 34.81586596186931359, 6.466735817496056526 ) ) ;
#8896 = CARTESIAN_POINT ( 'NONE',  ( 31.79760674661912745, -3.928098387035230843, -4.516596916592202859 ) ) ;
#8897 = CARTESIAN_POINT ( 'NONE',  ( -1.419070666119118362, -31.15705752543471618, 6.989977667959445640 ) ) ;
#8898 = CARTESIAN_POINT ( 'NONE',  ( -1.265720463714046895, -27.71192368072266277, 7.750000000000000888 ) ) ;
#8899 = CARTESIAN_POINT ( 'NONE',  ( -64.47965924086506107, 36.51034344918481622, 5.743161323598027224 ) ) ;
#8900 = CARTESIAN_POINT ( 'NONE',  ( 21.99536180190331791, 0.2400875630283233197, -7.664209021738525252 ) ) ;
#8901 = DIRECTION ( 'NONE',  ( -0.000000000000000000, 1.000000000000000000, -0.000000000000000000 ) ) ;
#8902 = EDGE_CURVE ( 'NONE', #14684, #22934, #7989, .T. ) ;
#8903 = AXIS2_PLACEMENT_3D ( 'NONE', #34781, #5731, #3084 ) ;
#8904 = CARTESIAN_POINT ( 'NONE',  ( -26.24874870218063450, -25.49307895267003587, 6.700000000000000178 ) ) ;
#8905 = VECTOR ( 'NONE', #13336, 1000.000000000000000 ) ;
#8906 = CARTESIAN_POINT ( 'NONE',  ( -14.97867591359219119, -24.55319635012989110, 6.800000000000000711 ) ) ;
#8907 = CARTESIAN_POINT ( 'NONE',  ( 36.87700637240019574, -3.319742436231731819, -5.919978869301625757 ) ) ;
#8908 = CARTESIAN_POINT ( 'NONE',  ( 3.448281132886812372, -32.59848922884697231, 7.767720160662273443 ) ) ;
#8909 = DIRECTION ( 'NONE',  ( -1.000000000000000000, 0.000000000000000000, 0.000000000000000000 ) ) ;
#8910 = CARTESIAN_POINT ( 'NONE',  ( -0.08052498442271191492, -26.55690155986885514, 7.700536657684214248 ) ) ;
#8911 = CARTESIAN_POINT ( 'NONE',  ( 0.4087657880184312753, -32.81786754902258707, 7.771081512783700518 ) ) ;
#8912 = DIRECTION ( 'NONE',  ( -0.4999999999999918954, -0.8660254037844432595, -0.000000000000000000 ) ) ;
#8913 = CARTESIAN_POINT ( 'NONE',  ( 4.626733377823518012, -27.83888570657239470, 7.695279973900954751 ) ) ;
#8914 = VECTOR ( 'NONE', #23608, 1000.000000000000000 ) ;
#8915 = PLANE ( 'NONE',  #9657 ) ;
#8916 = CARTESIAN_POINT ( 'NONE',  ( 21.43086650153212247, 7.999394493581059251, 2.743190574498553413 ) ) ;
#8917 = CARTESIAN_POINT ( 'NONE',  ( 22.27214042976725494, 1.964039760382519040, -5.564636450190440620 ) ) ;
#8918 = ORIENTED_EDGE ( 'NONE', *, *, #16229, .F. ) ;
#8919 = ORIENTED_EDGE ( 'NONE', *, *, #10458, .T. ) ;
#8920 = CARTESIAN_POINT ( 'NONE',  ( 70.76671532128065678, 59.91573877893261368, -3.942344351592494966 ) ) ;
#8921 = EDGE_CURVE ( 'NONE', #38495, #1346, #18068, .T. ) ;
#8922 = ORIENTED_EDGE ( 'NONE', *, *, #2297, .T. ) ;
#8923 = DIRECTION ( 'NONE',  ( -0.000000000000000000, -0.000000000000000000, -1.000000000000000000 ) ) ;
#8924 = ADVANCED_FACE ( 'NONE', ( #12307, #30657 ), #2467, .F. ) ;
#8925 = CARTESIAN_POINT ( 'NONE',  ( -1.420557875848984741, -25.57630196027997727, 6.954324564059724878 ) ) ;
#8926 = LINE ( 'NONE', #21300, #22866 ) ;
#8927 = CARTESIAN_POINT ( 'NONE',  ( -1.418010585399023471, -28.21509543055201519, 6.929923840112064859 ) ) ;
#8928 = CARTESIAN_POINT ( 'NONE',  ( 4.905245326634070757, -30.70523247011419699, 7.730758795053810140 ) ) ;
#8929 = ITEM_DEFINED_TRANSFORMATION ( 'NONE', 'NONE', #39950,  #30744 ) ;
#8930 = CARTESIAN_POINT ( 'NONE',  ( -14.44874870218064089, -26.64985754041175525, 6.700000000000000178 ) ) ;
#8931 = VERTEX_POINT ( 'NONE', #27549 ) ;
#8932 = CARTESIAN_POINT ( 'NONE',  ( 23.75454047524076273, 3.573438420936730253, 3.145647371460261965 ) ) ;
#8933 = AXIS2_PLACEMENT_3D ( 'NONE', #5067, #29975, #35965 ) ;
#8934 = CIRCLE ( 'NONE', #28011, 4.500000000000003553 ) ;
#8935 = ORIENTED_EDGE ( 'NONE', *, *, #14435, .F. ) ;
#8936 = ORIENTED_EDGE ( 'NONE', *, *, #25950, .F. ) ;
#8937 = CARTESIAN_POINT ( 'NONE',  ( 78.62541471602109766, 65.39282990155331277, -2.732428818688202199 ) ) ;
#8938 = CARTESIAN_POINT ( 'NONE',  ( 21.85642363622424256, 10.16974155675050895, -2.500000000000000444 ) ) ;
#8939 = CARTESIAN_POINT ( 'NONE',  ( 81.63129934975491153, 61.79668339569251145, -1.832274617051100618 ) ) ;
#8940 = CARTESIAN_POINT ( 'NONE',  ( 79.24578529683977024, 64.32976145010150049, 3.589982250315052692 ) ) ;
#8941 = AXIS2_PLACEMENT_3D ( 'NONE', #21020, #39951, #8647 ) ;
#8942 = CARTESIAN_POINT ( 'NONE',  ( 4.435220079103089574, -27.54985462435614352, 6.949473656533212917 ) ) ;
#8943 = CARTESIAN_POINT ( 'NONE',  ( 2.896981936218417264, -32.75240845689362601, 7.695279973900954751 ) ) ;
#8944 = CARTESIAN_POINT ( 'NONE',  ( 21.85643539959775339, 5.487231995601864476, 10.01193108169250578 ) ) ;
#8945 = ORIENTED_EDGE ( 'NONE', *, *, #5799, .F. ) ;
#8946 = CARTESIAN_POINT ( 'NONE',  ( -72.89934385729463884, 3.418700917153234098, 9.863801266169547333 ) ) ;
#8947 = CARTESIAN_POINT ( 'NONE',  ( 4.301450302647315205, -31.91148321001355370, 7.754798119455333705 ) ) ;
#8948 = DIRECTION ( 'NONE',  ( 0.000000000000000000, 0.000000000000000000, -1.000000000000000000 ) ) ;
#8949 = CARTESIAN_POINT ( 'NONE',  ( 1.650073881887274441, -32.96957273148993295, 7.785868773668302545 ) ) ;
#8950 = CARTESIAN_POINT ( 'NONE',  ( 30.69044931928128150, -3.119424076483234387, -4.996384886243276924 ) ) ;
#8951 = CARTESIAN_POINT ( 'NONE',  ( 36.20119281512496912, -3.652236176559757741, -5.717025003991615506 ) ) ;
#8952 = APPLICATION_CONTEXT ( 'automotive_design' ) ;
#8953 = CARTESIAN_POINT ( 'NONE',  ( 3.721376283916915106, -32.30408730072721823, 6.969307238440509700 ) ) ;
#8954 = CARTESIAN_POINT ( 'NONE',  ( 15.23756541667567177, 11.44821579467915917, 2.584588623821235220 ) ) ;
#8955 = LINE ( 'NONE', #34321, #16174 ) ;
#8956 = CARTESIAN_POINT ( 'NONE',  ( -14.44874870218064089, -26.64985754041175525, 6.800000000000000711 ) ) ;
#8957 = CARTESIAN_POINT ( 'NONE',  ( -69.92844875602597199, -0.6521111472992819902, 3.916091961299970059 ) ) ;
#8958 = CARTESIAN_POINT ( 'NONE',  ( -70.92837670882107659, 28.72470171467712063, 0.000000000000000000 ) ) ;
#8959 = CARTESIAN_POINT ( 'NONE',  ( 24.58814725198859463, 2.979487925962025052, -3.568875956100880042 ) ) ;
#8960 = ORIENTED_EDGE ( 'NONE', *, *, #16666, .F. ) ;
#8961 = CIRCLE ( 'NONE', #4387, 2.000000000000000000 ) ;
#8962 = CARTESIAN_POINT ( 'NONE',  ( 67.49481586879284123, 58.02828806359071478, 3.995059460290581121 ) ) ;
#8963 = CARTESIAN_POINT ( 'NONE',  ( 36.64797015977908501, -3.154251671283775593, 5.926200096577949772 ) ) ;
#8964 = CARTESIAN_POINT ( 'NONE',  ( 4.951209458787976914, -30.83330630559114383, 7.782861076432731728 ) ) ;
#8965 = AXIS2_PLACEMENT_3D ( 'NONE', #39744, #18318, #6552 ) ;
#8966 = EDGE_CURVE ( 'NONE', #28414, #8713, #15773, .T. ) ;
#8967 = CARTESIAN_POINT ( 'NONE',  ( -60.81661347076553170, 25.20155461598435309, 9.800414904976365804 ) ) ;
#8968 = CARTESIAN_POINT ( 'NONE',  ( 86.69901843299427924, 0.4902165918510832388, 5.965927736749048194 ) ) ;
#8969 = EDGE_CURVE ( 'NONE', #5530, #33055, #14991, .T. ) ;
#8972 = CARTESIAN_POINT ( 'NONE',  ( 35.89239603134597445, -2.095832607348167453, -5.808274480206606860 ) ) ;
#8971 = AXIS2_PLACEMENT_3D ( 'NONE', #30800, #2806, #27681 ) ;
#8970 = DIRECTION ( 'NONE',  ( 1.000000000000000000, 0.000000000000000000, 0.000000000000000000 ) ) ;
#8973 = CARTESIAN_POINT ( 'NONE',  ( -1.554008717359405489, -30.55426820241236996, 6.895222827070025318 ) ) ;
#8974 = EDGE_LOOP ( 'NONE', ( #2386, #20118, #15802, #36932 ) ) ;
#8975 = CARTESIAN_POINT ( 'NONE',  ( 24.55420261656340486, 2.734525497827099638, 3.876975801173430103 ) ) ;
#8976 = CARTESIAN_POINT ( 'NONE',  ( 0.6964302473834028673, -32.82569116364354045, 7.139196562012269709 ) ) ;
#8977 = EDGE_LOOP ( 'NONE', ( #12312, #38255, #33167, #35120 ) ) ;
#8978 = CARTESIAN_POINT ( 'NONE',  ( -70.14820770166069508, -21.41850222705690143, 3.949606264851799775 ) ) ;
#8979 = UNCERTAINTY_MEASURE_WITH_UNIT (LENGTH_MEASURE( 1.000000000000000082E-05 ), #27662, 'distance_accuracy_value', 'NONE');
#8980 = VERTEX_POINT ( 'NONE', #37220 ) ;
#8981 = ORIENTED_EDGE ( 'NONE', *, *, #21406, .T. ) ;
#8982 = CARTESIAN_POINT ( 'NONE',  ( 78.91366476310541600, 65.65666373793331445, -2.561782662428539137 ) ) ;
#8983 = CARTESIAN_POINT ( 'NONE',  ( 2.896246704383601323, -32.76027228102909561, 7.257242401810563237 ) ) ;
#8984 = CARTESIAN_POINT ( 'NONE',  ( 81.03127633846482070, 61.72971393008359797, 2.526545245021025288 ) ) ;
#8986 = VERTEX_POINT ( 'NONE', #9215 ) ;
#8985 = CARTESIAN_POINT ( 'NONE',  ( 14.72021916802316710, 13.05558383789457189, 2.500000000000000444 ) ) ;
#8988 = VECTOR ( 'NONE', #780, 1000.000000000000000 ) ;
#8987 = CARTESIAN_POINT ( 'NONE',  ( 74.25112698293331448, 59.69246930110610805, -3.692213121326705760 ) ) ;
#8989 = CARTESIAN_POINT ( 'NONE',  ( -58.97367982820826171, 28.25997590259050440, 6.371614496329753408 ) ) ;
#8990 =( BOUNDED_CURVE ( )  B_SPLINE_CURVE ( 3, ( #11215, #7938, #21124, #17804 ),
 .UNSPECIFIED., .F., .F. ) 
 B_SPLINE_CURVE_WITH_KNOTS ( ( 4, 4 ),
 ( 1.381924640371169577, 1.574767692156077148 ),
 .UNSPECIFIED. ) 
 CURVE ( )  GEOMETRIC_REPRESENTATION_ITEM ( )  RATIONAL_B_SPLINE_CURVE ( ( 1.000000000000000000, 0.9969033633783033199, 0.9969033633783033199, 1.000000000000000000 ) ) 
 REPRESENTATION_ITEM ( '' )  );
#8992 = CARTESIAN_POINT ( 'NONE',  ( 27.05168840568772737, -4.558788516904208166, 3.571571921055567866 ) ) ;
#8991 = FACE_OUTER_BOUND ( 'NONE', #36882, .T. ) ;
#8993 = CYLINDRICAL_SURFACE ( 'NONE', #27485, 0.09010775117052950700 ) ;
#8994 = AXIS2_PLACEMENT_3D ( 'NONE', #23025, #4099, #23417 ) ;
#8995 = DIRECTION ( 'NONE',  ( 1.000000000000000000, 1.385724075720358314E-16, -0.000000000000000000 ) ) ;
#8996 = ADVANCED_FACE ( 'NONE', ( #31063 ), #6355, .F. ) ;
#8997 = VECTOR ( 'NONE', #26192, 1000.000000000000000 ) ;
#8998 = CARTESIAN_POINT ( 'NONE',  ( 22.03617269645906518, 5.395735386727952054, -3.201102023609922131 ) ) ;
#8999 = VERTEX_POINT ( 'NONE', #2671 ) ;
#9000 = CARTESIAN_POINT ( 'NONE',  ( 2.044608497525232327, -26.08006147301429323, 7.501983001166817822 ) ) ;
#9001 = CIRCLE ( 'NONE', #27399, 6.172764123155108251 ) ;
#9002 = CARTESIAN_POINT ( 'NONE',  ( -78.62055188009620110, -5.380212206548604215, -6.429298165712081570 ) ) ;
#9003 = DIRECTION ( 'NONE',  ( 1.000000000000000000, -0.000000000000000000, -0.000000000000000000 ) ) ;
#9004 = CARTESIAN_POINT ( 'NONE',  ( 79.87861596566079925, 65.47018085071599103, 3.015642068896304817 ) ) ;
#9005 = CARTESIAN_POINT ( 'NONE',  ( 88.33724419093491065, -2.316998127210522007, 1.237639510709749091 ) ) ;
#9006 = CARTESIAN_POINT ( 'NONE',  ( 3.435265683109236967, -26.53015935524666347, 7.750000000000001776 ) ) ;
#9007 = VERTEX_POINT ( 'NONE', #40103 ) ;
#9008 = CARTESIAN_POINT ( 'NONE',  ( 2.882800830503455369, -26.27570657257135878, 7.638132480492517473 ) ) ;
#9009 = DIRECTION ( 'NONE',  ( -0.1736481776669206722, -0.9848077530122096857, -0.000000000000000000 ) ) ;
#9010 = EDGE_CURVE ( 'NONE', #27482, #39459, #30926, .T. ) ;
#9011 = CARTESIAN_POINT ( 'NONE',  ( -24.44874870218064089, -26.64985754041175525, 6.800000000000000711 ) ) ;
#9012 = CARTESIAN_POINT ( 'NONE',  ( 33.97726142433466379, -3.803478383426091458, -5.244974327395966363 ) ) ;
#9013 = DIRECTION ( 'NONE',  ( 0.7864880931482284288, 0.000000000000000000, -0.6176054398530371747 ) ) ;
#9014 = CARTESIAN_POINT ( 'NONE',  ( 85.59323660014052848, 0.9850445873831121801, 5.800130443767659294 ) ) ;
#9015 = CARTESIAN_POINT ( 'NONE',  ( -0.4543040637718891994, -26.93983748258725797, 7.784838882742138644 ) ) ;
#9016 = ORIENTED_EDGE ( 'NONE', *, *, #10230, .F. ) ;
#9017 = CARTESIAN_POINT ( 'NONE',  ( 36.99213799685487203, -2.719433212406895173, 5.979915811284242544 ) ) ;
#9018 = CARTESIAN_POINT ( 'NONE',  ( 4.279060409011795407, -31.78590715249458754, 7.784838882742138644 ) ) ;
#9019 = LINE ( 'NONE', #30665, #36418 ) ;
#9020 = EDGE_CURVE ( 'NONE', #29749, #36272, #2690, .T. ) ;
#9021 = ORIENTED_EDGE ( 'NONE', *, *, #3905, .F. ) ;
#9023 = CARTESIAN_POINT ( 'NONE',  ( 14.67630592591299532, -4.947493968569943945, 2.499999999999956035 ) ) ;
#9022 = CARTESIAN_POINT ( 'NONE',  ( 81.30779604900573077, 61.65202803940792364, -2.079311677127713587 ) ) ;
#9024 = DIRECTION ( 'NONE',  ( -0.000000000000000000, 1.000000000000000000, -0.000000000000000000 ) ) ;
#9025 = DIRECTION ( 'NONE',  ( -1.000000000000000000, 0.000000000000000000, 0.000000000000000000 ) ) ;
#9026 = CARTESIAN_POINT ( 'NONE',  ( 3.472176508934365913, -32.58834150085273507, 7.651421919295145813 ) ) ;
#9027 = CARTESIAN_POINT ( 'NONE',  ( 14.62016757377762843, 13.26415307787954490, -2.488228758613686864 ) ) ;
#9028 = CIRCLE ( 'NONE', #20200, 2.500000000000000444 ) ;
#9029 = ORIENTED_EDGE ( 'NONE', *, *, #9667, .T. ) ;
#9030 = DIRECTION ( 'NONE',  ( 1.000000000000000000, 0.000000000000000000, -0.000000000000000000 ) ) ;
#9031 = ORIENTED_EDGE ( 'NONE', *, *, #9858, .T. ) ;
#9032 = ORIENTED_EDGE ( 'NONE', *, *, #37591, .F. ) ;
#9033 = CARTESIAN_POINT ( 'NONE',  ( 81.10109024085375040, 61.27893947540407993, -1.252362053669520359 ) ) ;
#9034 = CARTESIAN_POINT ( 'NONE',  ( -58.64967482348269101, 27.97946873212456609, -5.671478272894442618 ) ) ;
#9035 = ORIENTED_EDGE ( 'NONE', *, *, #11696, .T. ) ;
#9037 = CARTESIAN_POINT ( 'NONE',  ( 34.15825286562033369, -0.5798779905139902491, 5.173835020267440576 ) ) ;
#9036 = CARTESIAN_POINT ( 'NONE',  ( 24.92005442864145692, 2.530202585715988217, 3.974294703006678642 ) ) ;
#9038 = ORIENTED_EDGE ( 'NONE', *, *, #11639, .T. ) ;
#9039 = CARTESIAN_POINT ( 'NONE',  ( 81.44289297360079161, 64.86039221060740090, -2.864610283900680621 ) ) ;
#9040 = CARTESIAN_POINT ( 'NONE',  ( -1.635225080001443621, -33.52415522258557701, 7.635761828346577573 ) ) ;
#9041 = ORIENTED_EDGE ( 'NONE', *, *, #31351, .F. ) ;
#9043 = DIRECTION ( 'NONE',  ( 1.000000000000000000, 0.000000000000000000, 0.000000000000000000 ) ) ;
#9042 = CARTESIAN_POINT ( 'NONE',  ( 4.888398419654542693, -28.38813185588637111, 7.643333865083955736 ) ) ;
#9044 = LINE ( 'NONE', #22248, #35635 ) ;
#9045 = CARTESIAN_POINT ( 'NONE',  ( 0.4869470754961160996, -26.28701135364670805, 7.750000000000001776 ) ) ;
#9046 = CARTESIAN_POINT ( 'NONE',  ( 73.68879688780705806, 59.40709336146452557, 3.677837812263893280 ) ) ;
#9047 = ADVANCED_FACE ( 'NONE', ( #15190 ), #40302, .F. ) ;
#9048 = CARTESIAN_POINT ( 'NONE',  ( 21.85761542531931667, 3.396825223608685995, -4.782081994692843452 ) ) ;
#9049 = ORIENTED_EDGE ( 'NONE', *, *, #38297, .F. ) ;
#9050 = VECTOR ( 'NONE', #3783, 1000.000000000000227 ) ;
#9051 = CARTESIAN_POINT ( 'NONE',  ( 21.85643539959774273, 11.87467848218428834, -0.9583437110454642305 ) ) ;
#9052 = CARTESIAN_POINT ( 'NONE',  ( -58.55403975902957114, 30.31577878493534328, -5.141676377603731751 ) ) ;
#9053 = VERTEX_POINT ( 'NONE', #34784 ) ;
#9054 = CARTESIAN_POINT ( 'NONE',  ( -55.09640557796760874, 31.27756524517855041, -1.408921623440186677 ) ) ;
#9055 = CARTESIAN_POINT ( 'NONE',  ( 79.08571093829937126, 66.16712123189805084, 1.622497907168705122 ) ) ;
#9056 = CARTESIAN_POINT ( 'NONE',  ( 88.25986434197210428, -0.7799440980648532085, -3.332403339731401015 ) ) ;
#9057 = ORIENTED_EDGE ( 'NONE', *, *, #40617, .T. ) ;
#9058 = CARTESIAN_POINT ( 'NONE',  ( 3.936759689487521641, -26.87759828911498516, 7.750000000000000888 ) ) ;
#9059 = EDGE_CURVE ( 'NONE', #6937, #27683, #38781, .T. ) ;
#9060 = ADVANCED_FACE ( 'NONE', ( #32290 ), #3990, .T. ) ;
#9061 = CARTESIAN_POINT ( 'NONE',  ( -0.9270654228314927359, -27.41204290387628006, 7.691066658568940007 ) ) ;
#9062 = CARTESIAN_POINT ( 'NONE',  ( 23.84525472439710114, -3.061681620743719190, 3.851870993270792187 ) ) ;
#9063 = ADVANCED_FACE ( 'NONE', ( #4088 ), #3897, .F. ) ;
#9064 = CARTESIAN_POINT ( 'NONE',  ( 24.98419795007806599, 3.112932432632140145, 2.907112638396472715 ) ) ;
#9065 = CARTESIAN_POINT ( 'NONE',  ( 36.79834255099314078, -2.555168371936516358, -5.949669344996932452 ) ) ;
#9066 = CARTESIAN_POINT ( 'NONE',  ( 5.100205970968322511, -29.53454346407160358, 7.680992449362115337 ) ) ;
#9067 = B_SPLINE_CURVE_WITH_KNOTS ( 'NONE', 3,
 ( #23958, #27470, #5862, #2381 ),
 .UNSPECIFIED., .F., .F.,
 ( 4, 4 ),
 ( 0.1795419177415450984, 0.3391172959757620120 ),
 .UNSPECIFIED. ) ;
#9068 = CARTESIAN_POINT ( 'NONE',  ( -68.92837670882107659, -42.87473357531881391, 0.000000000000000000 ) ) ;
#9069 = CARTESIAN_POINT ( 'NONE',  ( -15.07867591359219439, -26.64985754041175525, 6.700000000000000178 ) ) ;
#9070 = CARTESIAN_POINT ( 'NONE',  ( 1.732227763654782704, -33.06978601425814190, 7.724038915126860694 ) ) ;
#9071 = ADVANCED_FACE ( 'NONE', ( #25893 ), #11835, .F. ) ;
#9072 = ORIENTED_EDGE ( 'NONE', *, *, #14164, .T. ) ;
#9073 = CARTESIAN_POINT ( 'NONE',  ( 34.13640354093743667, -3.787416915700777764, 5.295493011275766548 ) ) ;
#9074 = CIRCLE ( 'NONE', #1207, 0.1000000000000028644 ) ;
#9075 = CARTESIAN_POINT ( 'NONE',  ( -71.82557191872977853, -0.3413572496726843264, 3.932540834694423726 ) ) ;
#9076 = ORIENTED_EDGE ( 'NONE', *, *, #16362, .F. ) ;
#9077 = CARTESIAN_POINT ( 'NONE',  ( 66.96362040430034313, 58.12048686563063882, -3.996315564296189837 ) ) ;
#9078 = CARTESIAN_POINT ( 'NONE',  ( -71.92837670882106238, -36.87473357531881391, 1.732050807568877637 ) ) ;
#9079 = VERTEX_POINT ( 'NONE', #16215 ) ;
#9080 = CARTESIAN_POINT ( 'NONE',  ( 87.29047730454419707, 0.3089174322584790633, -4.712845393775586977 ) ) ;
#9081 = CARTESIAN_POINT ( 'NONE',  ( -72.53275211461026117, 6.278950858466555651, -9.872183956496360935 ) ) ;
#9082 = CARTESIAN_POINT ( 'NONE',  ( -71.92837670882107659, -20.91541689163215523, 5.916079783099619682 ) ) ;
#9083 = ORIENTED_EDGE ( 'NONE', *, *, #39130, .F. ) ;
#9084 = FACE_OUTER_BOUND ( 'NONE', #2168, .T. ) ;
#9085 = DIRECTION ( 'NONE',  ( -0.000000000000000000, -1.000000000000000000, -0.000000000000000000 ) ) ;
#9086 = EDGE_LOOP ( 'NONE', ( #20552, #39708, #5410, #30730, #28705, #34228 ) ) ;
#9087 = B_SPLINE_CURVE_WITH_KNOTS ( 'NONE', 3,
 ( #3317, #30888, #6379, #40130, #21203, #27577, #33777, #11910, #2700, #15218, #15417, #15837 ),
 .UNSPECIFIED., .F., .F.,
 ( 4, 2, 2, 2, 1, 1, 4 ),
 ( 0.000000000000000000, 0.3310684008954036806, 0.4966026013431050767, 0.5172943763990670574, 0.5379861514550290380, 0.5793697015669526662, 0.6621368017907995895 ),
 .UNSPECIFIED. ) ;
#9088 = CARTESIAN_POINT ( 'NONE',  ( 22.88251133645001190, 4.300788154828764753, 3.108290358268387177 ) ) ;
#9089 = CARTESIAN_POINT ( 'NONE',  ( 82.39191784114034078, 64.57324092874033283, -1.480606629406893804 ) ) ;
#9090 = FACE_OUTER_BOUND ( 'NONE', #3968, .T. ) ;
#9091 = CIRCLE ( 'NONE', #7767, 4.357836081054403010 ) ;
#9092 = EDGE_CURVE ( 'NONE', #1802, #22985, #592, .T. ) ;
#9093 = CARTESIAN_POINT ( 'NONE',  ( 78.81037980241194418, 65.98117473861063331, 1.881209715725460807 ) ) ;
#9094 = CARTESIAN_POINT ( 'NONE',  ( -0.1647035100567555144, -32.41271505934994934, 6.903372536218456368 ) ) ;
#9095 = ORIENTED_EDGE ( 'NONE', *, *, #12832, .T. ) ;
#9096 = CARTESIAN_POINT ( 'NONE',  ( 76.55173188639216164, 63.61528062424579133, -3.435658781974418208 ) ) ;
#9097 = DIRECTION ( 'NONE',  ( -0.000000000000000000, -1.000000000000000000, -0.000000000000000000 ) ) ;
#9098 = CARTESIAN_POINT ( 'NONE',  ( 0.6393374818712781460, -26.33972546746960575, 7.768425012602592439 ) ) ;
#9099 = CARTESIAN_POINT ( 'NONE',  ( 80.52090910898354537, 64.76150916408994362, -3.396356880839462633 ) ) ;
#9100 = CARTESIAN_POINT ( 'NONE',  ( 76.55173188639217585, 63.61528062424576291, 3.435658781974429754 ) ) ;
#9101 = VERTEX_POINT ( 'NONE', #993 ) ;
#9102 = CARTESIAN_POINT ( 'NONE',  ( 1.682951012397970292, -26.06997362959739206, 7.750000000000000888 ) ) ;
#9103 = AXIS2_PLACEMENT_3D ( 'NONE', #18793, #3191, #15707 ) ;
#9104 = CARTESIAN_POINT ( 'NONE',  ( -58.28298022874874107, 31.18432397053788563, 4.639529439632331886 ) ) ;
#9105 = CARTESIAN_POINT ( 'NONE',  ( 82.47197227462061164, 63.49890707693140257, 1.793694987645559680 ) ) ;
#9107 = FACE_OUTER_BOUND ( 'NONE', #6867, .T. ) ;
#9106 = CARTESIAN_POINT ( 'NONE',  ( -64.08758708074094557, 43.19434570387343086, 2.104943988446417169 ) ) ;
#9108 = AXIS2_PLACEMENT_3D ( 'NONE', #37156, #21931, #2807 ) ;
#9109 = CARTESIAN_POINT ( 'NONE',  ( 33.86666996155606313, -5.260714354287511441, -2.203027216165969637 ) ) ;
#9110 = EDGE_CURVE ( 'NONE', #11306, #1015, #13130, .T. ) ;
#9111 = CARTESIAN_POINT ( 'NONE',  ( -1.381908803976582778, -31.22810341674602697, 6.863784140767622333 ) ) ;
#9112 = CARTESIAN_POINT ( 'NONE',  ( -63.41460867333827167, 35.63977781315514193, -6.822401110719517270 ) ) ;
#9113 = CARTESIAN_POINT ( 'NONE',  ( 1.514465823680740453, -33.06498843269217502, 6.921725064902952695 ) ) ;
#9114 = CARTESIAN_POINT ( 'NONE',  ( 24.73558894963412769, 0.6121252408484304519, -4.779902904745515713 ) ) ;
#9115 = EDGE_CURVE ( 'NONE', #18951, #4028, #38637, .T. ) ;
#9116 = DIRECTION ( 'NONE',  ( 0.000000000000000000, 0.000000000000000000, 1.000000000000000000 ) ) ;
#9117 = FACE_OUTER_BOUND ( 'NONE', #4706, .T. ) ;
#9118 = CARTESIAN_POINT ( 'NONE',  ( 78.50997293154887302, 60.39266868650268094, 2.556923618988971914 ) ) ;
#9119 = CARTESIAN_POINT ( 'NONE',  ( 33.44004484032286229, -3.434887717533713580, -5.408154456503273977 ) ) ;
#9120 = CARTESIAN_POINT ( 'NONE',  ( 21.67022219558699803, 4.173608694407422881, -3.080183803507759333 ) ) ;
#9121 = CARTESIAN_POINT ( 'NONE',  ( 67.59755685981747320, 57.89445231122055446, -3.999999999999877875 ) ) ;
#9122 = DIRECTION ( 'NONE',  ( 0.000000000000000000, 0.000000000000000000, 1.000000000000000000 ) ) ;
#9123 = DIRECTION ( 'NONE',  ( 1.000000000000000000, 0.000000000000000000, 0.000000000000000000 ) ) ;
#9124 = LINE ( 'NONE', #15094, #39642 ) ;
#9125 = CARTESIAN_POINT ( 'NONE',  ( -18.44874870218064089, -26.64985754041175525, 6.700000000000000178 ) ) ;
#9126 = CARTESIAN_POINT ( 'NONE',  ( 4.638101942922436827, -27.85824998890764448, 7.635761828346577573 ) ) ;
#9127 = CARTESIAN_POINT ( 'NONE',  ( -64.08758708074093136, 36.14363715547679590, -3.800414904976364028 ) ) ;
#9128 = VECTOR ( 'NONE', #32250, 1000.000000000000000 ) ;
#9129 = CARTESIAN_POINT ( 'NONE',  ( 2.829498134096899431, -26.36288870688320074, 7.691066658568949777 ) ) ;
#9130 = CARTESIAN_POINT ( 'NONE',  ( 24.03622579959568029, 1.870140213503554527, -4.518823370007700291 ) ) ;
#9131 = EDGE_LOOP ( 'NONE', ( #10423, #7126, #11894, #34602 ) ) ;
#9132 = LINE ( 'NONE', #28071, #11971 ) ;
#9133 = CARTESIAN_POINT ( 'NONE',  ( 69.99634961962405555, 58.48381665884328839, -3.916752429509929190 ) ) ;
#9134 = EDGE_LOOP ( 'NONE', ( #16550, #7961, #39049, #21917 ) ) ;
#9135 = CARTESIAN_POINT ( 'NONE',  ( 5.056857618328627346, -29.02759656560906976, 6.894806418505346812 ) ) ;
#9136 = DIRECTION ( 'NONE',  ( 0.000000000000000000, 1.000000000000000000, 0.000000000000000000 ) ) ;
#9137 = CARTESIAN_POINT ( 'NONE',  ( 5.007779359891471493, -28.42486414215694168, 6.875671892026061549 ) ) ;
#9138 = CARTESIAN_POINT ( 'NONE',  ( 4.863529718378640787, -30.81674521050610949, 7.778050822775630202 ) ) ;
#9139 = CARTESIAN_POINT ( 'NONE',  ( 5.030132119480741792, -30.25761027875940812, 7.774064877406528851 ) ) ;
#9140 = ORIENTED_EDGE ( 'NONE', *, *, #20394, .T. ) ;
#9141 = CARTESIAN_POINT ( 'NONE',  ( 22.18551630692656218, 5.282241039200648025, 3.062960712820621101 ) ) ;
#9142 = FACE_OUTER_BOUND ( 'NONE', #20732, .T. ) ;
#9143 = ORIENTED_EDGE ( 'NONE', *, *, #8403, .F. ) ;
#9144 = CARTESIAN_POINT ( 'NONE',  ( 80.62600653171161014, 61.47375110407241294, -2.475680338657084256 ) ) ;
#9145 = CARTESIAN_POINT ( 'NONE',  ( -1.678079929080388721, -29.95195194214872814, 6.949473656533220023 ) ) ;
#9146 = CARTESIAN_POINT ( 'NONE',  ( 80.82569761265823161, 65.28806468744758718, -2.919551171211518970 ) ) ;
#9147 = CARTESIAN_POINT ( 'NONE',  ( 79.14523234120532891, 64.60782394083949498, 3.482780605906210525 ) ) ;
#9148 = EDGE_CURVE ( 'NONE', #20444, #13284, #35182, .T. ) ;
#9149 = DIRECTION ( 'NONE',  ( -0.7660444431189813441, 0.6427876096865353661, -0.000000000000000000 ) ) ;
#9150 = EDGE_CURVE ( 'NONE', #17955, #6604, #24343, .T. ) ;
#9151 = B_SPLINE_SURFACE_WITH_KNOTS ( 'NONE', 3, 3, ( 
 ( #4840, #24182, #1978, #17370, #29948, #14496, #27263, #36946, #18602, #5659, #21518, #9340, #2387 ),
 ( #40635, #2597, #18200, #34494, #28083, #37144, #37346, #27674, #37543, #12013, #19031, #18815, #34091 ),
 ( #34703, #105, #30992, #34300, #25210, #2797, #40421, #3008, #24806, #9141, #11802, #15733, #27479 ),
 ( #8726, #15116, #30790, #5867, #15525, #28285, #40229, #14912, #21715, #40032, #27875, #21918, #12638 ),
 ( #21306, #12438, #24590, #8932, #24386, #33882, #37739, #15321, #12228, #6068, #9548, #31187, #25005 ),
 ( #6268, #6479, #31389, #3213, #22129, #16529, #16720, #29106, #13657, #909, #26226, #13446, #28493 ),
 ( #1124, #514, #7271, #10147, #22738, #34905, #35699, #10553, #26021, #16329, #38761, #9955, #19834 ),
 ( #38352, #38551, #9757, #22538, #23130, #35301, #35101, #10361, #6877, #22936, #22337, #7471, #31593 ),
 ( #19432, #32007, #3417, #15929, #303, #12841, #3812, #28903, #32810, #30312, #20423, #30115, #29509 ),
 ( #36488, #4598, #1716, #14045, #39155, #4792, #14246, #33004, #35897, #23719, #4994, #11150, #10747 ),
 ( #14446, #1318, #17519, #17322, #29901, #29700, #26820, #39775, #36286, #24120, #36688, #23328, #20029 ),
 ( #32610, #7674, #33427, #2125, #23912, #4407, #5196, #17127, #20622, #8062, #33208, #13857, #17728 ),
 ( #1924, #26424, #20228, #1512, #23532, #27017, #14642, #26620, #16931, #39564, #10950, #11347, #8260 ),
 ( #27214, #36098, #20831, #11549, #8672, #8468, #5398, #34440, #21461, #14851, #21052, #3162, #5607 ),
 ( #18550, #17939, #55, #31134, #39980, #36893, #9088, #6218, #21664, #31338, #34242, #15680, #6014 ),
 ( #37294, #21864, #21252, #12386, #27818, #40370, #11752, #12585, #28228, #2952, #34036, #9285, #18145 ),
 ( #8879, #15267, #15468, #2330, #30734, #18763, #2744, #2538, #28029, #11958, #24745, #27417, #25151 ),
 ( #33623, #15063, #30520, #24329, #33824, #12174, #40576, #27621, #40177, #24535, #37089, #5809, #30938 ),
 ( #18348, #24954, #37490, #35453, #25561, #13603, #9491, #22077, #18979, #3965, #458, #9908, #31543 ),
 ( #16484, #37686, #28440, #16284, #248, #12786, #9706, #25361, #37899, #19179, #22285, #29057, #864 ),
 ( #34854, #13397, #31743, #3557, #22489, #35053, #25970, #19384, #31954, #38503, #36239, #35650, #23280 ),
 ( #7825, #20180, #4552, #10904, #20374, #13999, #1270, #29856, #11101, #4742, #4357, #23086, #20571 ),
 ( #23673, #26570, #39107, #35847, #32956, #5148, #1667, #30263, #2082, #29459, #26175, #13809, #26377 ),
 ( #23480, #8211, #20785, #39516, #39311, #10701, #36048, #7420, #11297, #17275, #32558, #7626, #38909 ),
 ( #19978, #14200, #32763, #17077, #33158, #38708, #29654, #8018, #1465, #26774, #17472, #4944, #30064 ),
 ( #1876, #14399, #26970, #10504, #23862, #33379, #17683, #30472, #17891, #24069, #8421, #14595, #36642 ),
 ( #33576, #27166, #39723, #5353, #20997, #11504, #19025, #16132, #32403, #31589, #7064, #19428, #6475 ),
 ( #13441, #25806, #4196, #3805, #903, #16714, #19828, #31999, #16325, #28898, #13241, #4006, #6873 ),
 ( #19633, #32207, #38346, #705, #22732, #10354, #16524, #15924, #7265, #10142, #35296, #9543, #12836 ),
 ( #19225, #25407, #29100, #29304, #26016, #38546, #22926, #35495, #37945, #12632, #13042, #3413, #25202 ),
 ( #37734, #28488, #31790, #22124, #34698, #6677, #296, #9753, #22332, #34900, #3606, #28696, #508 ),
 ( #25604, #38147, #9950, #22533, #35097, #40323, #33776, #27369, #22026, #24484, #31088, #37441, #36842 ),
 ( #9239, #18091, #15013, #27976, #12537, #40524, #9443, #12333, #34600, #24907, #24282, #15416, #5 ),
 ( #31291, #5959, #18504, #30684, #31492, #6378, #21816, #12116, #28180, #37040, #3113, #27771, #34194 ),
 ( #21202, #8825, #25109, #21614, #21410, #34398, #30887, #2898, #5553, #3316, #18926, #39930, #33985 ),
 ( #6169, #11705, #18710, #15631, #37638, #8623, #40129, #2491, #24694, #27576, #11909, #5759, #18299 ),
 ( #9036, #2699, #15217, #37244, #38259, #3714, #31695, #19538, #812, #35206, #34805, #12738, #10255 ),
 ( #13344, #16240, #28809, #25513, #10056, #35603, #32118, #19929, #32507, #6582, #15836, #3512, #19128 ),
 ( #613, #38657, #10454, #29207, #29008, #411, #13153, #25317, #1019, #25715, #22238, #38059, #22638 ),
 ( #28392, #23036, #12950, #3921, #25918, #37848, #7372, #38453, #16034, #28602, #16434, #13551, #22836 ),
 ( #35405, #200, #7178, #9653, #19737, #26127, #9861, #32311, #6977, #4108, #22435, #35005, #6779 ),
 ( #16624, #19333, #31903, #39258, #10653, #39457, #11246, #17419, #33103, #14344, #2025, #8158, #7576 ),
 ( #20519, #7968, #1227, #4506, #4888, #10852, #17028, #30004, #39665, #36188, #20730, #33315, #36386 ),
 ( #14541, #4695, #26915, #13761, #1418, #5095, #29603, #26721, #39053, #23429, #29801, #11049, #32905 ),
 ( #1822, #23810, #23624, #23232, #26325, #17628, #38862, #30208, #17227, #1613, #13954, #27115, #24015 ),
 ( #8368, #20940, #35798, #4307, #32711, #20129, #26520, #14148, #11449, #36591, #16829, #29413, #35994 ),
 ( #7775, #20323, #34499, #39877, #15532, #11654, #13053, #27317, #9553, #36790, #12443, #311, #33526 ),
 ( #31600, #33720, #8575, #25416, #19038, #28089, #28291, #18042, #28499, #2443, #9964, #9764, #25010 ),
 ( #3423, #31803, #37957, #21154, #28707, #22136, #37748, #30417, #5499, #34710, #40640, #30635, #6486 ),
 ( #12848, #34914, #37549, #9344, #19237, #520, #15739, #111, #21925, #5297, #22344, #3617, #6273 ),
 ( #17834, #2224, #14746, #25218, #18821, #31394, #24229, #6689, #16145, #25615, #3223, #12644, #38158 ),
 ( #15934, #4208, #1519, #38767, #26627, #39161, #13253, #22545, #10155, #715, #32216, #10367, #4605 ),
 ( #35903, #35704, #7079, #22944, #32013, #7684, #35506, #28909, #4018, #25822, #14052, #16338, #10563 ),
 ( #919, #29516, #35107, #16536, #20037, #22744, #38359, #13864, #7480, #29113, #16728, #19645, #16938 ),
 ( #6885, #38959, #13454, #4413, #19438, #20233, #38557, #13663, #17134, #7278, #19842, #32618, #3821 ),
 ( #29314, #26026, #32817, #35309, #32413, #1130, #26233, #1325, #23137, #26432, #10755, #23334, #29709 ),
 ( #2131, #39987, #15071, #18153, #30323, #17734, #27221, #11556, #2337, #5203, #17330, #5406, #17945 ),
 ( #24129, #11156, #23727, #10956, #7881, #36901, #23920, #29908, #23540, #5613, #8068, #14649, #21058 ),
 ( #2545, #33630, #1723, #39366, #36694, #8678, #8475, #33832, #30528, #30741, #14857, #20431, #39784 ),
 ( #36293, #27427, #11758, #24337, #14253, #27627, #36105, #21260, #36496, #33010, #20629, #4799, #11354 ),
 ( #26825, #33216, #5001, #17526, #30121, #1933, #14454, #27025, #39570, #8267, #20838, #33433, #6638 ) ),
 .UNSPECIFIED., .F., .F., .F.,
 ( 4, 3, 3, 3, 3, 3, 3, 3, 3, 3, 3, 3, 3, 3, 3, 3, 3, 3, 3, 3, 4 ),
 ( 4, 3, 3, 3, 4 ),
 ( 0.01398653888977024161, 0.01402123637946461540, 0.01403858512431180317, 0.01405593386915899093, 0.01412532884854774198, 0.01426411880732524062, 0.01454169872488023790, 0.01509685855999023593, 0.01620717823021022852, 0.01676233806532022655, 0.01731749790043022458, 0.01787265773554021914, 0.01842781757065021717, 0.01953813724087020975, 0.02064845691109020581, 0.02175877658131019840, 0.02231393641642019643, 0.02259151633397519371, 0.02273030629275269235, 0.02279970127214143993, 0.02286909625153019099 ),
 ( 0.000000000000000000, 0.2500000000000000000, 0.5000000000000000000, 0.7500000000000000000, 1.000000000000000000 ),
 .UNSPECIFIED. ) ;
#9152 = CARTESIAN_POINT ( 'NONE',  ( 2.754382185031206465, -32.80243705429514733, 7.761597726988848756 ) ) ;
#9153 = CARTESIAN_POINT ( 'NONE',  ( 21.85643539959773207, -8.152057848754798997, -9.377623736650162911 ) ) ;
#9154 = VERTEX_POINT ( 'NONE', #17812 ) ;
#9155 = CARTESIAN_POINT ( 'NONE',  ( -74.65391122663345413, 7.539060228346531112, 9.329047404371412000 ) ) ;
#9156 = CARTESIAN_POINT ( 'NONE',  ( -1.799583860900191734, -29.58343279012807159, 7.635761828346577573 ) ) ;
#9157 = EDGE_CURVE ( 'NONE', #10884, #7860, #9323, .T. ) ;
#9158 = CARTESIAN_POINT ( 'NONE',  ( -70.92837670882107659, -65.19654454972992141, -6.000000000000002665 ) ) ;
#9159 = EDGE_CURVE ( 'NONE', #27685, #14002, #9890, .T. ) ;
#9160 = CARTESIAN_POINT ( 'NONE',  ( 1.619884156912658746, -32.96898955208958171, 7.782034975670476307 ) ) ;
#9161 = VECTOR ( 'NONE', #17485, 1000.000000000000000 ) ;
#9162 = CARTESIAN_POINT ( 'NONE',  ( 32.88580308198496738, -3.566010387612386090, -5.242313469937768033 ) ) ;
#9163 = CARTESIAN_POINT ( 'NONE',  ( 37.11022902811986768, -2.403443262945340830, -5.951558886896759937 ) ) ;
#9164 = CARTESIAN_POINT ( 'NONE',  ( 3.726385264851022061, -32.30037768601651749, 6.988553391373224954 ) ) ;
#9165 = CARTESIAN_POINT ( 'NONE',  ( 3.967303130966486790, -27.03592930924035187, 7.768425012602596880 ) ) ;
#9166 = DIRECTION ( 'NONE',  ( 0.3757233601570931225, 0.9267318687906784813, 0.000000000000000000 ) ) ;
#9167 = B_SPLINE_CURVE_WITH_KNOTS ( 'NONE', 3,
 ( #31015, #28108, #15138, #18223, #3244, #18847, #15961, #31620, #37570, #9365 ),
 .UNSPECIFIED., .F., .F.,
 ( 4, 3, 3, 4 ),
 ( 2.742838647325547832E-18, 3.025570593003418284E-05, 6.051145698344212605E-05, 6.468151674594278821E-05 ),
 .UNSPECIFIED. ) ;
#9168 = CARTESIAN_POINT ( 'NONE',  ( -66.12008681484671513, 35.44165918782573499, -8.117242773420016988 ) ) ;
#9169 = DIRECTION ( 'NONE',  ( 0.000000000000000000, -0.000000000000000000, -1.000000000000000000 ) ) ;
#9170 = B_SPLINE_CURVE_WITH_KNOTS ( 'NONE', 3,
 ( #39215, #30382, #11208, #7530, #11409, #2186, #36152, #23186, #17382, #14102, #7930, #29963, #14304, #39418, #26874, #23975, #23773, #36350, #20089, #33272, #27081, #32666, #4466, #5054, #23588, #39626, #7733, #14506, #11003, #26479, #23384 ),
 .UNSPECIFIED., .F., .F.,
 ( 4, 3, 3, 3, 3, 3, 3, 3, 3, 3, 4 ),
 ( 1.226634733346699349E-18, 2.999644130997555441E-05, 6.002588995694558974E-05, 8.960886084587723428E-05, 0.0001190604700446452712, 0.0001489538463052706904, 0.0001796139255493956052, 0.0002109707048517044494, 0.0002426195318110353836, 0.0002740640997890060756, 0.0002849778069099853954 ),
 .UNSPECIFIED. ) ;
#9171 = CARTESIAN_POINT ( 'NONE',  ( 17.21125213350858374, 14.40030432582220321, -2.500000000000000000 ) ) ;
#9172 = CARTESIAN_POINT ( 'NONE',  ( 22.07014027993533745, 0.3234589711692046343, -7.440383244949039465 ) ) ;
#9173 = CARTESIAN_POINT ( 'NONE',  ( 36.58489777812268784, -1.843467954662745711, -5.775056006311750423 ) ) ;
#9174 = CARTESIAN_POINT ( 'NONE',  ( 24.50653798433103248, 2.969344662950985203, -3.630665793498612626 ) ) ;
#9175 = ORIENTED_EDGE ( 'NONE', *, *, #6398, .T. ) ;
#9176 = CARTESIAN_POINT ( 'NONE',  ( 67.14253272251396254, 58.08395421452478757, 3.998868826385352460 ) ) ;
#9177 = CARTESIAN_POINT ( 'NONE',  ( 34.12768836152103802, -3.289258482637194891, 5.532849168731702960 ) ) ;
#9178 = CARTESIAN_POINT ( 'NONE',  ( 4.981062705491726916, -30.77339773246524857, 7.773839561854630986 ) ) ;
#9179 = AXIS2_PLACEMENT_3D ( 'NONE', #30636, #30005, #33722 ) ;
#9180 = DIRECTION ( 'NONE',  ( -0.000000000000000000, 1.000000000000000000, -0.000000000000000000 ) ) ;
#9181 = CARTESIAN_POINT ( 'NONE',  ( 87.20660408302002509, 0.2574974038930863407, -5.635807106906071340 ) ) ;
#9183 = CARTESIAN_POINT ( 'NONE',  ( 21.63111991302532289, 6.952063906928881210, 2.990424737892750429 ) ) ;
#9182 = CARTESIAN_POINT ( 'NONE',  ( -70.92837670882201451, -21.78299143689573469, 6.000000000001379341 ) ) ;
#9184 = ORIENTED_EDGE ( 'NONE', *, *, #20166, .T. ) ;
#9185 = CARTESIAN_POINT ( 'NONE',  ( 24.71424333793793693, 2.641769286553297125, 3.922768386337302626 ) ) ;
#9186 = CARTESIAN_POINT ( 'NONE',  ( -63.99293516169446150, 35.89893413629672381, -46.17089178453873188 ) ) ;
#9187 = ORIENTED_EDGE ( 'NONE', *, *, #23836, .T. ) ;
#9188 = CARTESIAN_POINT ( 'NONE',  ( -70.60020594839741648, -21.73402473355089271, 6.003896035474983073 ) ) ;
#9189 = CIRCLE ( 'NONE', #6599, 2.500000000000002220 ) ;
#9190 = ORIENTED_EDGE ( 'NONE', *, *, #40021, .T. ) ;
#9191 = CARTESIAN_POINT ( 'NONE',  ( 78.57794565308390133, 65.91709162046845449, -1.743126864185871705 ) ) ;
#9192 = CARTESIAN_POINT ( 'NONE',  ( -1.698180065124302196, -29.47090112884363222, 7.774064877406529739 ) ) ;
#9193 = CARTESIAN_POINT ( 'NONE',  ( 80.83598165300548999, 61.89502789394175863, 2.843122152733552177 ) ) ;
#9195 = ORIENTED_EDGE ( 'NONE', *, *, #15997, .T. ) ;
#9194 = CARTESIAN_POINT ( 'NONE',  ( -1.326714576903637033, -31.11803783986836791, 6.882085323592684212 ) ) ;
#9196 = CARTESIAN_POINT ( 'NONE',  ( -0.02954975575422185557, -26.53738454105226197, 7.778495531946296282 ) ) ;
#9198 = CARTESIAN_POINT ( 'NONE',  ( -73.07498068578524908, 39.58105274722134226, 12.49999999999999645 ) ) ;
#9197 = DIRECTION ( 'NONE',  ( 0.1736481776669404897, -0.9848077530122062440, -0.000000000000000000 ) ) ;
#9199 = CARTESIAN_POINT ( 'NONE',  ( 2.562099542307729738, -33.75548367670988625, 7.754798119455333705 ) ) ;
#9200 = CARTESIAN_POINT ( 'NONE',  ( 33.89869710337333686, -5.476906865792886769, -0.08692379071555116077 ) ) ;
#9201 = CARTESIAN_POINT ( 'NONE',  ( 23.14461240764244110, 3.993051640458494589, -3.167054870709993697 ) ) ;
#9202 = ORIENTED_EDGE ( 'NONE', *, *, #6443, .F. ) ;
#9203 = EDGE_CURVE ( 'NONE', #19738, #20650, #33415, .T. ) ;
#9204 = EDGE_CURVE ( 'NONE', #10597, #10909, #15669, .T. ) ;
#9205 = EDGE_CURVE ( 'NONE', #35449, #29219, #23049, .T. ) ;
#9206 = CARTESIAN_POINT ( 'NONE',  ( -77.88159744744395141, -5.098111721919734940, -7.193586285049241802 ) ) ;
#9207 = DIRECTION ( 'NONE',  ( -0.000000000000000000, -0.000000000000000000, -1.000000000000000000 ) ) ;
#9208 = CARTESIAN_POINT ( 'NONE',  ( 79.33055955479062504, 65.97011375961720603, 2.296576099417798833 ) ) ;
#9209 = CARTESIAN_POINT ( 'NONE',  ( 87.30284416890829391, -1.044652313481390760, -5.185858056390752147 ) ) ;
#9210 = CARTESIAN_POINT ( 'NONE',  ( 1.686887486498408029, -26.16995699532097319, 7.635761828346577573 ) ) ;
#9211 = ORIENTED_EDGE ( 'NONE', *, *, #22710, .F. ) ;
#9212 = FACE_OUTER_BOUND ( 'NONE', #14784, .T. ) ;
#9213 = CARTESIAN_POINT ( 'NONE',  ( 3.446800832104334855, -26.65272994776861637, 6.889465824494256374 ) ) ;
#9214 = ORIENTED_EDGE ( 'NONE', *, *, #17230, .T. ) ;
#9215 = CARTESIAN_POINT ( 'NONE',  ( -12.87867591359218977, -24.55319635012989110, 6.800000000000000711 ) ) ;
#9216 = TOROIDAL_SURFACE ( 'NONE', #14471, 67.42751648247021024, 3.000000000000000000 ) ;
#9217 = CARTESIAN_POINT ( 'NONE',  ( 26.27924180621979033, -3.292740819196297686, -4.154355880966675407 ) ) ;
#9218 = CARTESIAN_POINT ( 'NONE',  ( -68.33309634912853880, 36.51831931741240567, -8.800414904976365804 ) ) ;
#9219 = PLANE ( 'NONE',  #21381 ) ;
#9220 = CARTESIAN_POINT ( 'NONE',  ( -0.3956209610833227308, -26.89285385646818582, 7.761597726988853196 ) ) ;
#9221 = CARTESIAN_POINT ( 'NONE',  ( 32.77968338845805363, -0.9315752336664611111, 5.322460391044158357 ) ) ;
#9222 = DIRECTION ( 'NONE',  ( 1.000000000000000000, 0.000000000000000000, 0.000000000000000000 ) ) ;
#9223 = ORIENTED_EDGE ( 'NONE', *, *, #4492, .T. ) ;
#9225 = DIRECTION ( 'NONE',  ( -0.000000000000000000, -0.000000000000000000, -1.000000000000000000 ) ) ;
#9224 = CARTESIAN_POINT ( 'NONE',  ( 81.32777602152022212, 61.82240453612693187, -2.372413575842100997 ) ) ;
#9226 = CARTESIAN_POINT ( 'NONE',  ( 18.75851303975696993, -2.772082833101076282, 3.134117654843073364 ) ) ;
#9227 = CARTESIAN_POINT ( 'NONE',  ( -12.99139449055068241, -10.90558813203967148, -6.000000000000000000 ) ) ;
#9228 = DIRECTION ( 'NONE',  ( -0.000000000000000000, -1.000000000000000000, -0.000000000000000000 ) ) ;
#9229 = EDGE_LOOP ( 'NONE', ( #20121, #22176 ) ) ;
#9230 = AXIS2_PLACEMENT_3D ( 'NONE', #33191, #4977, #17505 ) ;
#9231 = CARTESIAN_POINT ( 'NONE',  ( -1.648904451518951042, -28.98487051485360411, 7.763628509615286610 ) ) ;
#9232 = CARTESIAN_POINT ( 'NONE',  ( -0.4832139993529582234, -26.85040468425802018, 7.782861076432729952 ) ) ;
#9233 = VERTEX_POINT ( 'NONE', #37572 ) ;
#9234 = VERTEX_POINT ( 'NONE', #31017 ) ;
#9235 = CARTESIAN_POINT ( 'NONE',  ( 81.09516781258611218, 61.58556622376320888, -2.215902410107941645 ) ) ;
#9236 =( BOUNDED_CURVE ( )  B_SPLINE_CURVE ( 3, ( #32634, #39588, #11373, #23939 ),
 .UNSPECIFIED., .F., .T. ) 
 B_SPLINE_CURVE_WITH_KNOTS ( ( 4, 4 ),
 ( 4.748221474220557958, 4.941946782021392259 ),
 .UNSPECIFIED. ) 
 CURVE ( )  GEOMETRIC_REPRESENTATION_ITEM ( )  RATIONAL_B_SPLINE_CURVE ( ( 1.000000000000000000, 0.9968749865767494445, 0.9968749865767494445, 1.000000000000000000 ) ) 
 REPRESENTATION_ITEM ( '' )  );
#9237 = CARTESIAN_POINT ( 'NONE',  ( -9.439742135462632078, 51.66544268451064426, 1.000000000000000000 ) ) ;
#9238 = ORIENTED_EDGE ( 'NONE', *, *, #20266, .T. ) ;
#9240 = CARTESIAN_POINT ( 'NONE',  ( 36.08394752551300400, -1.509676803322822503, 5.633451637947094248 ) ) ;
#9239 = CARTESIAN_POINT ( 'NONE',  ( 24.54955273022989104, 2.736081411429597487, 3.876714146131560401 ) ) ;
#9241 = VERTEX_POINT ( 'NONE', #33699 ) ;
#9242 = CARTESIAN_POINT ( 'NONE',  ( 81.15665777833298478, 65.46403653819187696, -2.541832380859318619 ) ) ;
#9243 = AXIS2_PLACEMENT_3D ( 'NONE', #33233, #8698, #23742 ) ;
#9244 = FACE_OUTER_BOUND ( 'NONE', #38250, .T. ) ;
#9246 = CARTESIAN_POINT ( 'NONE',  ( -42.83131703149249603, -32.06993018339340296, 6.800000000000000711 ) ) ;
#9245 = CARTESIAN_POINT ( 'NONE',  ( -69.95461280117120850, -0.5204835624159770413, 5.920672442023852788 ) ) ;
#9247 = LINE ( 'NONE', #15639, #17196 ) ;
#9248 = FACE_OUTER_BOUND ( 'NONE', #26263, .T. ) ;
#9249 = CARTESIAN_POINT ( 'NONE',  ( 73.49116904989887189, 59.86802450872643533, 3.864208391251975350 ) ) ;
#9250 = CARTESIAN_POINT ( 'NONE',  ( 22.04453315957904991, 3.307593561896943868, -4.656839850646330881 ) ) ;
#9251 = ORIENTED_EDGE ( 'NONE', *, *, #6993, .F. ) ;
#9252 = CARTESIAN_POINT ( 'NONE',  ( 21.85643539959777826, -3.868027658932458479, -14.06783426539529458 ) ) ;
#9254 = ADVANCED_FACE ( 'NONE', ( #2826 ), #27506, .F. ) ;
#9253 = CARTESIAN_POINT ( 'NONE',  ( 17.12093179650376129, 14.48834468576525047, 3.790908043361841617 ) ) ;
#9255 = VERTEX_POINT ( 'NONE', #5478 ) ;
#9256 = DIRECTION ( 'NONE',  ( 0.000000000000000000, 0.000000000000000000, 1.000000000000000000 ) ) ;
#9257 = CARTESIAN_POINT ( 'NONE',  ( 81.30277405988996975, 64.78683171160542997, 3.017922835037553320 ) ) ;
#9258 = CARTESIAN_POINT ( 'NONE',  ( 87.73528170195316989, -0.1907079786014589107, -4.255344914058586170 ) ) ;
#9259 = ORIENTED_EDGE ( 'NONE', *, *, #19722, .T. ) ;
#9260 = CIRCLE ( 'NONE', #8606, 4.357836081054403010 ) ;
#9261 = CARTESIAN_POINT ( 'NONE',  ( 3.557203646265561847, -26.60307234877650018, 7.751599049952199394 ) ) ;
#9262 = CARTESIAN_POINT ( 'NONE',  ( 21.52115149856448539, -2.719794669569747469, 3.565294201003603280 ) ) ;
#9263 = CARTESIAN_POINT ( 'NONE',  ( 21.58862418887968460, 7.202556094215188054, 2.923978954502209682 ) ) ;
#9264 = CARTESIAN_POINT ( 'NONE',  ( 36.78955161406895513, -3.042595920340447346, -5.948297306680297325 ) ) ;
#9265 = CARTESIAN_POINT ( 'NONE',  ( 5.098960251590484383, -29.66895923794316658, 7.774064877406529739 ) ) ;
#9266 = CARTESIAN_POINT ( 'NONE',  ( 22.01622206693788897, 4.835086392017111656, 3.641232820207879417 ) ) ;
#9267 = CIRCLE ( 'NONE', #35601, 0.1000000000000028644 ) ;
#9268 = CARTESIAN_POINT ( 'NONE',  ( -2.954197855305039422, -12.43481156997016157, -1.000000000000000000 ) ) ;
#9269 = CARTESIAN_POINT ( 'NONE',  ( -1.259118276085812171, -31.24364169136941882, 7.782167645815905033 ) ) ;
#9270 = VECTOR ( 'NONE', #7166, 999.9999999999998863 ) ;
#9271 = ORIENTED_EDGE ( 'NONE', *, *, #33288, .F. ) ;
#9272 = EDGE_LOOP ( 'NONE', ( #28139, #19471, #19436, #14663 ) ) ;
#9273 = CARTESIAN_POINT ( 'NONE',  ( 34.63594631419880443, -0.7840636577548021346, 5.277534085818968990 ) ) ;
#9274 = CARTESIAN_POINT ( 'NONE',  ( -71.62860729996657483, -0.06907469158448548141, 5.971043812772921733 ) ) ;
#9275 = ORIENTED_EDGE ( 'NONE', *, *, #15019, .T. ) ;
#9276 = EDGE_CURVE ( 'NONE', #36200, #38679, #7357, .T. ) ;
#9277 = CARTESIAN_POINT ( 'NONE',  ( 66.55417948260128469, 57.87814544581552667, -3.999688274315071901 ) ) ;
#9278 = ORIENTED_EDGE ( 'NONE', *, *, #15718, .F. ) ;
#9279 = CARTESIAN_POINT ( 'NONE',  ( -56.05592576813391048, 30.85738657449499200, 3.898523360614989386 ) ) ;
#9280 = CARTESIAN_POINT ( 'NONE',  ( -76.25573767795857805, -5.662030444549658981, -8.470992006596512525 ) ) ;
#9281 = CARTESIAN_POINT ( 'NONE',  ( 69.01538019125142398, 59.48397956797946762, 3.903581769792375145 ) ) ;
#9282 = FACE_BOUND ( 'NONE', #21815, .T. ) ;
#9283 = CARTESIAN_POINT ( 'NONE',  ( -28.97867591359219475, -26.64985754041175525, 6.800000000000000711 ) ) ;
#9284 = ORIENTED_EDGE ( 'NONE', *, *, #12792, .F. ) ;
#9285 = CARTESIAN_POINT ( 'NONE',  ( 21.84668416186902817, 5.868252050249999741, 3.176222544669724090 ) ) ;
#9286 = CARTESIAN_POINT ( 'NONE',  ( 81.01700449632683387, 66.08979032036403112, -1.386429027374526335 ) ) ;
#9287 = CARTESIAN_POINT ( 'NONE',  ( -22.24874870218063450, -26.64985754041175525, 6.700000000000000178 ) ) ;
#9288 = EDGE_CURVE ( 'NONE', #33732, #23016, #32908, .T. ) ;
#9289 = CARTESIAN_POINT ( 'NONE',  ( 81.02339296473685692, 62.20010510126473235, 2.956864960647747065 ) ) ;
#9290 = CARTESIAN_POINT ( 'NONE',  ( -1.751823616877372869, -28.99354058093586772, 7.724038915126862470 ) ) ;
#9291 = VERTEX_POINT ( 'NONE', #27293 ) ;
#9292 = CARTESIAN_POINT ( 'NONE',  ( 77.35950424652850188, 60.48040194676352144, -3.253266109310609888 ) ) ;
#9294 = DIRECTION ( 'NONE',  ( 0.000000000000000000, 1.000000000000000000, 0.000000000000000000 ) ) ;
#9293 = CARTESIAN_POINT ( 'NONE',  ( 2.365931152121737213, -26.13377987989076345, 6.873189335546979528 ) ) ;
#9295 = CARTESIAN_POINT ( 'NONE',  ( 17.88216549226283192, 8.679122384522569789, -2.924350684386651356 ) ) ;
#9296 = CARTESIAN_POINT ( 'NONE',  ( 81.27876882982985762, 62.57402737888430266, -3.057227112800022795 ) ) ;
#9297 = CARTESIAN_POINT ( 'NONE',  ( 79.13122682291692911, 61.20693062157217668, 3.102003663616994533 ) ) ;
#9298 = ORIENTED_EDGE ( 'NONE', *, *, #38120, .F. ) ;
#9299 = DIRECTION ( 'NONE',  ( -0.000000000000000000, -1.000000000000000000, -0.000000000000000000 ) ) ;
#9300 = AXIS2_PLACEMENT_3D ( 'NONE', #10478, #23059, #16459 ) ;
#9302 = EDGE_CURVE ( 'NONE', #4011, #5538, #34527, .T. ) ;
#9301 = LINE ( 'NONE', #31759, #11788 ) ;
#9303 = CARTESIAN_POINT ( 'NONE',  ( 81.78811924970003133, 65.04137315806649156, 2.360008641314786715 ) ) ;
#9305 = DIRECTION ( 'NONE',  ( -0.8660254037844345998, -0.5000000000000071054, -0.000000000000000000 ) ) ;
#9304 = CARTESIAN_POINT ( 'NONE',  ( 4.274037619018428380, -31.94193077376366574, 6.887547729233693516 ) ) ;
#9306 = CARTESIAN_POINT ( 'NONE',  ( 29.20850709934801159, 2.242166301403143880, -0.5075834600922535245 ) ) ;
#9307 = CARTESIAN_POINT ( 'NONE',  ( -1.416991000366785602, -31.16114644904380526, 6.998987538705435441 ) ) ;
#9308 = CARTESIAN_POINT ( 'NONE',  ( -62.77981399768980708, 36.45869984972385680, -4.735036014756413891 ) ) ;
#9309 = CARTESIAN_POINT ( 'NONE',  ( -62.74554520265134272, 35.90271204080874412, 5.263896983009515473 ) ) ;
#9310 = CARTESIAN_POINT ( 'NONE',  ( 26.72022203379254890, 0.9438563279275373752, -4.381701199652399126 ) ) ;
#9311 = DIRECTION ( 'NONE',  ( 0.000000000000000000, 0.000000000000000000, 1.000000000000000000 ) ) ;
#9312 = CARTESIAN_POINT ( 'NONE',  ( 1.666437316484441933, -26.07009487170356721, 7.714178352335856026 ) ) ;
#9313 = B_SPLINE_CURVE_WITH_KNOTS ( 'NONE', 3,
 ( #32958, #19981, #7630, #35455, #29261, #1467, #26777, #14001, #13399, #26572 ),
 .UNSPECIFIED., .F., .F.,
 ( 4, 3, 3, 4 ),
 ( 0.0001585009270395759944, 0.0001815657551981854682, 0.0002118214035944135625, 0.0002170292169044765425 ),
 .UNSPECIFIED. ) ;
#9314 = CARTESIAN_POINT ( 'NONE',  ( 0.5160167997142889318, -32.86344804452599533, 7.635761828346576685 ) ) ;
#9315 = DIRECTION ( 'NONE',  ( -0.000000000000000000, -0.000000000000000000, -1.000000000000000000 ) ) ;
#9316 = CARTESIAN_POINT ( 'NONE',  ( 25.69802509246645172, 2.595865368573306409, -3.649276983290203447 ) ) ;
#9317 = CARTESIAN_POINT ( 'NONE',  ( 81.01435898429377858, 61.24732411474661831, -1.383612818681232426 ) ) ;
#9318 = CARTESIAN_POINT ( 'NONE',  ( 32.22182423589296008, -3.776180706330447112, 4.844886202978563539 ) ) ;
#9319 = CARTESIAN_POINT ( 'NONE',  ( -0.9173357114122402400, -31.73963204593200516, 7.779495906702015517 ) ) ;
#9320 = FACE_OUTER_BOUND ( 'NONE', #40575, .T. ) ;
#9321 = CARTESIAN_POINT ( 'NONE',  ( -6.448748702180637338, -26.64985754041175525, 6.800000000000000711 ) ) ;
#9322 = CARTESIAN_POINT ( 'NONE',  ( 1.664531801855456017, -26.17011927939601890, 7.691066658568947112 ) ) ;
#9323 = B_SPLINE_CURVE_WITH_KNOTS ( 'NONE', 3,
 ( #4864, #29580, #30397, #5272, #26891, #11022, #27094, #35971, #2003, #26698, #17398, #20705, #20105, #23404, #39643, #20497 ),
 .UNSPECIFIED., .F., .F.,
 ( 4, 2, 2, 2, 2, 2, 2, 4 ),
 ( 0.000000000000000000, 0.0004252485765279650489, 0.0008504971530559300979, 0.001275745729583895038, 0.001700994306111860196, 0.002126242882639825353, 0.002551491459167790077, 0.003401988612223739907 ),
 .UNSPECIFIED. ) ;
#9324 = EDGE_CURVE ( 'NONE', #28414, #5730, #9369, .T. ) ;
#9325 = CARTESIAN_POINT ( 'NONE',  ( -1.453346889880533954, -28.29951960356443408, 7.761597726988851420 ) ) ;
#9326 = DIRECTION ( 'NONE',  ( 0.000000000000000000, -0.000000000000000000, -1.000000000000000000 ) ) ;
#9327 = ORIENTED_EDGE ( 'NONE', *, *, #7628, .F. ) ;
#9328 = CARTESIAN_POINT ( 'NONE',  ( 69.43824574602471955, 58.18893279706789201, -3.907754234428237439 ) ) ;
#9329 = EDGE_LOOP ( 'NONE', ( #30157, #30991, #26917 ) ) ;
#9330 = CARTESIAN_POINT ( 'NONE',  ( -89.20959394718985891, -30.27593629695115496, 6.864216812889196717 ) ) ;
#9331 = CARTESIAN_POINT ( 'NONE',  ( 0.04278369059588756074, -26.60137143983851615, 6.894806418505345924 ) ) ;
#9332 = CARTESIAN_POINT ( 'NONE',  ( 5.010720015369884095, -28.43335788139641807, 6.870737987065012042 ) ) ;
#9333 = EDGE_CURVE ( 'NONE', #1149, #12703, #40057, .T. ) ;
#9334 = EDGE_CURVE ( 'NONE', #36858, #17221, #13705, .T. ) ;
#9335 = CARTESIAN_POINT ( 'NONE',  ( 4.853254720949315093, -30.84250634616293851, 7.759451378593095860 ) ) ;
#9336 = AXIS2_PLACEMENT_3D ( 'NONE', #9475, #22063, #32156 ) ;
#9337 = CARTESIAN_POINT ( 'NONE',  ( 5.053699547558291094, -30.13146740640211974, 7.730758795053805699 ) ) ;
#9338 = VERTEX_POINT ( 'NONE', #35531 ) ;
#9339 = EDGE_CURVE ( 'NONE', #28028, #34419, #944, .T. ) ;
#9340 = CARTESIAN_POINT ( 'NONE',  ( 21.82753364412623043, 5.984910655522465817, 3.124155445945005383 ) ) ;
#9341 = FACE_OUTER_BOUND ( 'NONE', #28842, .T. ) ;
#9342 = ORIENTED_EDGE ( 'NONE', *, *, #30841, .T. ) ;
#9343 = CARTESIAN_POINT ( 'NONE',  ( 79.84787171156668251, 62.37423782317880239, -3.536670452273173559 ) ) ;
#9345 = CARTESIAN_POINT ( 'NONE',  ( -1.003265571170591786, -27.34726367792503510, 7.710604733652634657 ) ) ;
#9344 = CARTESIAN_POINT ( 'NONE',  ( 25.35072175385260707, 0.7578666051937779091, 4.606083722016952819 ) ) ;
#9346 = CARTESIAN_POINT ( 'NONE',  ( 81.34095870999071565, 61.40448684960411896, -1.344573736155065813 ) ) ;
#9347 = CARTESIAN_POINT ( 'NONE',  ( 80.06304181921890972, 62.74582375469539386, 3.589982250315065127 ) ) ;
#9348 = ORIENTED_EDGE ( 'NONE', *, *, #22760, .T. ) ;
#9349 = CARTESIAN_POINT ( 'NONE',  ( 4.434542230703401700, -27.54893547855059310, 6.939395833800437785 ) ) ;
#9350 = CARTESIAN_POINT ( 'NONE',  ( -70.92837670882107659, 28.72470171467712063, -3.784187430299790211 ) ) ;
#9351 = FACE_OUTER_BOUND ( 'NONE', #19539, .T. ) ;
#9352 = CARTESIAN_POINT ( 'NONE',  ( 21.85643539959778536, -7.083161344002194326, -10.43125315386002860 ) ) ;
#9353 = DIRECTION ( 'NONE',  ( -0.000000000000000000, -0.000000000000000000, 1.000000000000000000 ) ) ;
#9354 = VERTEX_POINT ( 'NONE', #19060 ) ;
#9355 = CARTESIAN_POINT ( 'NONE',  ( -73.66952994497191298, 5.999622647709867529, 9.674874949366538246 ) ) ;
#9356 = CARTESIAN_POINT ( 'NONE',  ( 36.07013428979532677, -3.674804590447603658, 5.686060082110223846 ) ) ;
#9357 = EDGE_LOOP ( 'NONE', ( #3062, #30595 ) ) ;
#9358 = DIRECTION ( 'NONE',  ( 0.9267318687906771491, -0.3757233601570964532, -0.000000000000000000 ) ) ;
#9359 = CARTESIAN_POINT ( 'NONE',  ( 1.736346942945643512, -32.96974004645320377, 7.703977250142847844 ) ) ;
#9360 = CARTESIAN_POINT ( 'NONE',  ( 1.651639975615219580, -32.96958066925694908, 6.894806418505345036 ) ) ;
#9361 = CARTESIAN_POINT ( 'NONE',  ( 37.10469866122600990, -3.126968154306207115, -5.976136871014097629 ) ) ;
#9362 = CARTESIAN_POINT ( 'NONE',  ( 3.813621333521583168, -32.23345227369436827, 6.866852738645443210 ) ) ;
#9363 = CARTESIAN_POINT ( 'NONE',  ( 3.357996495870312792, -32.53848892694827555, 6.894806418505347700 ) ) ;
#9364 = CARTESIAN_POINT ( 'NONE',  ( -27.07867591359219972, -24.55319635012989110, 6.700000000000000178 ) ) ;
#9365 = CARTESIAN_POINT ( 'NONE',  ( 4.327908163969746980, -31.72774129374395713, 7.695279973900954751 ) ) ;
#9366 = CARTESIAN_POINT ( 'NONE',  ( 5.751251297819365504, -26.64985754041175525, 6.700000000000000178 ) ) ;
#9367 = CIRCLE ( 'NONE', #4788, 3.499999999999999556 ) ;
#9368 = EDGE_CURVE ( 'NONE', #10291, #36291, #19669, .T. ) ;
#9369 = LINE ( 'NONE', #30610, #20399 ) ;
#9370 = CARTESIAN_POINT ( 'NONE',  ( 25.85236391290114710, 0.9906390358642165328, -4.433872417139598454 ) ) ;
#9371 = CYLINDRICAL_SURFACE ( 'NONE', #5629, 64.42751648247021024 ) ;
#9372 = CARTESIAN_POINT ( 'NONE',  ( 24.72152762843544593, 2.637715318777088758, -3.924694980037289227 ) ) ;
#9373 = ORIENTED_EDGE ( 'NONE', *, *, #34809, .F. ) ;
#9374 = CARTESIAN_POINT ( 'NONE',  ( 67.17215761800675011, 58.00255761909972563, 3.998533043703387690 ) ) ;
#9375 = CARTESIAN_POINT ( 'NONE',  ( 37.02720035777826268, -2.689369851865129224, 5.985388140692741388 ) ) ;
#9376 = CARTESIAN_POINT ( 'NONE',  ( -1.664990407196974553, -30.05394385900508070, 7.768425012602593327 ) ) ;
#9377 = ADVANCED_FACE ( 'NONE', ( #19863 ), #31623, .F. ) ;
#9378 = CARTESIAN_POINT ( 'NONE',  ( -68.98442902999595105, 21.93515443114010210, 9.800414904976365804 ) ) ;
#9380 = ADVANCED_FACE ( 'NONE', ( #29139 ), #22967, .F. ) ;
#9379 = CARTESIAN_POINT ( 'NONE',  ( 86.75210013534866960, -0.2795847087395720298, -5.842668109216860195 ) ) ;
#9381 = CARTESIAN_POINT ( 'NONE',  ( 35.97396611704095193, -3.154454633011662068, -5.821005464859283940 ) ) ;
#9382 = ORIENTED_EDGE ( 'NONE', *, *, #16102, .F. ) ;
#9383 = CARTESIAN_POINT ( 'NONE',  ( 25.86470230964163619, 2.040241906511436998, 4.181023058831703665 ) ) ;
#9384 = CARTESIAN_POINT ( 'NONE',  ( -70.66582705103253659, -21.75666374495045474, 5.995465708869195609 ) ) ;
#9385 = ADVANCED_FACE ( 'NONE', ( #16366 ), #22567, .F. ) ;
#9386 = ORIENTED_EDGE ( 'NONE', *, *, #16134, .F. ) ;
#9387 = CARTESIAN_POINT ( 'NONE',  ( 3.958376580442097392, -26.90712677766138938, 7.778495531946297170 ) ) ;
#9388 = UNCERTAINTY_MEASURE_WITH_UNIT (LENGTH_MEASURE( 1.000000000000000082E-05 ), #29902, 'distance_accuracy_value', 'NONE');
#9389 = VERTEX_POINT ( 'NONE', #15765 ) ;
#9390 = CARTESIAN_POINT ( 'NONE',  ( 80.93996669421788681, 61.38942684853014953, -2.064111563736698240 ) ) ;
#9391 = FACE_OUTER_BOUND ( 'NONE', #19485, .T. ) ;
#9392 = CARTESIAN_POINT ( 'NONE',  ( 80.98923082824005348, 61.23822351929057106, 1.409197735201532131 ) ) ;
#9396 = ORIENTED_EDGE ( 'NONE', *, *, #22057, .F. ) ;
#9395 = VERTEX_POINT ( 'NONE', #34734 ) ;
#9394 = CARTESIAN_POINT ( 'NONE',  ( 0.2020707124235944507, -34.04266111819475782, 7.754798119455333705 ) ) ;
#9393 = AXIS2_PLACEMENT_3D ( 'NONE', #27816, #15678, #18346 ) ;
#9397 = CARTESIAN_POINT ( 'NONE',  ( -58.48742492228146261, 29.43916413120543396, 5.126953147108460840 ) ) ;
#9398 = LINE ( 'NONE', #27936, #5199 ) ;
#9399 = CARTESIAN_POINT ( 'NONE',  ( -71.05882934118332628, -21.78299143688722239, 9.999999999999980460 ) ) ;
#9400 = CARTESIAN_POINT ( 'NONE',  ( 3.477237270422150139, -26.55450084266673727, 6.894806418505347700 ) ) ;
#9401 = CARTESIAN_POINT ( 'NONE',  ( 23.14002857363139753, 4.041596889213259658, -3.091365628204219007 ) ) ;
#9402 = ORIENTED_EDGE ( 'NONE', *, *, #33345, .F. ) ;
#9403 = CARTESIAN_POINT ( 'NONE',  ( -60.75950795826495465, 23.17721540975219696, 15.50000000000000000 ) ) ;
#9404 = CIRCLE ( 'NONE', #23887, 2.500000000000002220 ) ;
#9405 = DIRECTION ( 'NONE',  ( -0.9995570907297059993, -0.02975940812527387222, 2.753298341658001615E-16 ) ) ;
#9406 = DIRECTION ( 'NONE',  ( 0.000000000000000000, -0.000000000000000000, 1.000000000000000000 ) ) ;
#9407 = CARTESIAN_POINT ( 'NONE',  ( 80.86168855680165279, 64.16696250863010675, 3.456914256421386167 ) ) ;
#9408 = CARTESIAN_POINT ( 'NONE',  ( 85.51010218477300384, 1.603708918324822541, 5.381112834985590787 ) ) ;
#9409 = CARTESIAN_POINT ( 'NONE',  ( -20.24874870218063805, -26.64985754041175525, 6.700000000000000178 ) ) ;
#9410 = VERTEX_POINT ( 'NONE', #28732 ) ;
#9411 = DIRECTION ( 'NONE',  ( 1.000000000000000000, 0.000000000000000000, -0.000000000000000000 ) ) ;
#9412 = DIRECTION ( 'NONE',  ( 1.000000000000000000, -0.000000000000000000, 0.000000000000000000 ) ) ;
#9413 = VERTEX_POINT ( 'NONE', #3643 ) ;
#9414 = EDGE_CURVE ( 'NONE', #24982, #36231, #21716, .T. ) ;
#9415 = DIRECTION ( 'NONE',  ( 0.000000000000000000, 0.000000000000000000, 1.000000000000000000 ) ) ;
#9416 = CARTESIAN_POINT ( 'NONE',  ( 0.5083189215984570408, 0.5999999999999995337, 3.960569937088435299 ) ) ;
#9417 = CARTESIAN_POINT ( 'NONE',  ( -1.611334115997590688, -28.41660772738555707, 7.255881584735162981 ) ) ;
#9418 = CARTESIAN_POINT ( 'NONE',  ( 85.57589026689105083, 1.015016660241817359, 5.782947816673639885 ) ) ;
#9419 = ORIENTED_EDGE ( 'NONE', *, *, #11873, .F. ) ;
#9420 = CARTESIAN_POINT ( 'NONE',  ( 36.63317992190049210, -3.078756398745077227, 5.923891722253738834 ) ) ;
#9421 = AXIS2_PLACEMENT_3D ( 'NONE', #12429, #94, #34481 ) ;
#9422 = CARTESIAN_POINT ( 'NONE',  ( 87.79476240240137486, -0.2575195244695515639, -3.704994186184041194 ) ) ;
#9423 = ORIENTED_EDGE ( 'NONE', *, *, #32930, .F. ) ;
#9425 = DIRECTION ( 'NONE',  ( -0.000000000000000000, -1.000000000000000000, -0.000000000000000000 ) ) ;
#9424 = CARTESIAN_POINT ( 'NONE',  ( 80.17018276713265834, 64.56786917328069819, -3.540619799101245579 ) ) ;
#9426 = PLANE ( 'NONE',  #28739 ) ;
#9427 = CARTESIAN_POINT ( 'NONE',  ( -61.00670947824507806, 24.84364830758654108, 8.800414904976364028 ) ) ;
#9428 = EDGE_CURVE ( 'NONE', #36848, #2698, #38586, .T. ) ;
#9429 = ORIENTED_EDGE ( 'NONE', *, *, #19381, .T. ) ;
#9430 = CARTESIAN_POINT ( 'NONE',  ( 26.41406563113697104, -4.824719389755182775, -3.358585079837815623 ) ) ;
#9431 = ADVANCED_FACE ( 'NONE', ( #25847 ), #22369, .T. ) ;
#9432 = ORIENTED_EDGE ( 'NONE', *, *, #7304, .T. ) ;
#9433 = LINE ( 'NONE', #27013, #12323 ) ;
#9434 = AXIS2_PLACEMENT_3D ( 'NONE', #29581, #6956, #13739 ) ;
#9435 = AXIS2_PLACEMENT_3D ( 'NONE', #307, #31597, #3614 ) ;
#9436 = EDGE_CURVE ( 'NONE', #21757, #8555, #17742, .T. ) ;
#9438 = EDGE_LOOP ( 'NONE', ( #34567, #6371, #37261, #19880 ) ) ;
#9437 = ORIENTED_EDGE ( 'NONE', *, *, #37007, .T. ) ;
#9439 = CARTESIAN_POINT ( 'NONE',  ( 79.76203521409539121, 64.68678814937342736, -3.489836119548951121 ) ) ;
#9440 = B_SPLINE_CURVE_WITH_KNOTS ( 'NONE', 3,
 ( #24308, #18122, #30717, #20603 ),
 .UNSPECIFIED., .F., .F.,
 ( 4, 4 ),
 ( 0.000000000000000000, 6.391136169993328150E-06 ),
 .UNSPECIFIED. ) ;
#9441 = CARTESIAN_POINT ( 'NONE',  ( 35.96670479602093451, -3.154862874710424592, 5.819872160098396918 ) ) ;
#9442 = ORIENTED_EDGE ( 'NONE', *, *, #24500, .F. ) ;
#9444 = CARTESIAN_POINT ( 'NONE',  ( -12.24874870218063627, -26.64985754041175525, 6.700000000000000178 ) ) ;
#9443 = CARTESIAN_POINT ( 'NONE',  ( 23.11908726903853406, 2.858206452918472529, 4.238382280009368230 ) ) ;
#9445 = ORIENTED_EDGE ( 'NONE', *, *, #22485, .T. ) ;
#9446 = LINE ( 'NONE', #25517, #28800 ) ;
#9447 = CIRCLE ( 'NONE', #1588, 0.1000000000000028644 ) ;
#9448 = CARTESIAN_POINT ( 'NONE',  ( 4.744409466245708806, -31.29734294690251417, 7.737115613922532553 ) ) ;
#9450 = CARTESIAN_POINT ( 'NONE',  ( 86.14814696281284512, 1.592037090359822882, -4.564681075395820464 ) ) ;
#9449 = DIRECTION ( 'NONE',  ( 0.000000000000000000, 0.000000000000000000, -1.000000000000000000 ) ) ;
#9451 = CARTESIAN_POINT ( 'NONE',  ( -1.597336938230447867, -25.58391321841518007, 7.695279973900954751 ) ) ;
#9452 = CARTESIAN_POINT ( 'NONE',  ( 74.25112698293331448, 59.69246930110610805, 3.692213121326705760 ) ) ;
#9453 = CARTESIAN_POINT ( 'NONE',  ( 23.47264373427338313, 3.111346557503597676, -3.866181119602032368 ) ) ;
#9454 = ORIENTED_EDGE ( 'NONE', *, *, #35743, .T. ) ;
#9455 = CARTESIAN_POINT ( 'NONE',  ( 21.85643539959778536, -9.383538770078029501, -13.42257110913290141 ) ) ;
#9456 = CYLINDRICAL_SURFACE ( 'NONE', #29559, 3.399999999999999911 ) ;
#9457 = VERTEX_POINT ( 'NONE', #13275 ) ;
#9458 = CARTESIAN_POINT ( 'NONE',  ( -54.89808584415116144, 31.42838494644043124, -1.178527023292115006 ) ) ;
#9459 = CARTESIAN_POINT ( 'NONE',  ( 81.83449460947102239, 63.17368474096263498, 2.819252638153798340 ) ) ;
#9460 = CARTESIAN_POINT ( 'NONE',  ( 88.11777217834651310, -0.6203394357796320202, -3.242821525125987758 ) ) ;
#9461 = ORIENTED_EDGE ( 'NONE', *, *, #1726, .F. ) ;
#9462 = CARTESIAN_POINT ( 'NONE',  ( 14.61802080322508424, 12.62870316935584647, 2.500000000000000000 ) ) ;
#9463 = CARTESIAN_POINT ( 'NONE',  ( 33.94289416639321644, -3.572325359806576284, 5.436201825232916285 ) ) ;
#9464 = AXIS2_PLACEMENT_3D ( 'NONE', #5390, #2321, #9749 ) ;
#9465 = CARTESIAN_POINT ( 'NONE',  ( 34.77293049090385324, -3.164284130107499315, -5.633554808244025658 ) ) ;
#9466 = CARTESIAN_POINT ( 'NONE',  ( 5.100263068043492609, -29.54054047169235986, 7.661510568013095934 ) ) ;
#9467 = LINE ( 'NONE', #28419, #27902 ) ;
#9468 = CARTESIAN_POINT ( 'NONE',  ( 4.392721987511531978, -31.80629977964779442, 7.749999999999998224 ) ) ;
#9469 = TOROIDAL_SURFACE ( 'NONE', #27198, 114.6618724293813898, 3.000000000000000000 ) ;
#9470 = CARTESIAN_POINT ( 'NONE',  ( 8.290806648384990041, -33.63722727088462250, -2.499999999999998668 ) ) ;
#9471 = ORIENTED_EDGE ( 'NONE', *, *, #2873, .T. ) ;
#9472 = ORIENTED_EDGE ( 'NONE', *, *, #11089, .T. ) ;
#9473 = CARTESIAN_POINT ( 'NONE',  ( 37.21105169095337573, -2.744044523102963318, 6.000898145687354912 ) ) ;
#9474 =( BOUNDED_CURVE ( )  B_SPLINE_CURVE ( 3, ( #38367, #13064, #10164, #25625 ),
 .UNSPECIFIED., .F., .T. ) 
 B_SPLINE_CURVE_WITH_KNOTS ( ( 4, 4 ),
 ( 1.381924640371167801, 1.574767692156076482 ),
 .UNSPECIFIED. ) 
 CURVE ( )  GEOMETRIC_REPRESENTATION_ITEM ( )  RATIONAL_B_SPLINE_CURVE ( ( 1.000000000000000000, 0.9969033633783032089, 0.9969033633783032089, 1.000000000000000000 ) ) 
 REPRESENTATION_ITEM ( '' )  );
#9475 = CARTESIAN_POINT ( 'NONE',  ( 6.400024429904298984, -31.46803969333911866, 6.954324564059724878 ) ) ;
#9476 = EDGE_LOOP ( 'NONE', ( #9031, #13337, #40354, #22529 ) ) ;
#9477 = CARTESIAN_POINT ( 'NONE',  ( 66.42792150476888935, 57.77419247997853091, -4.000000000000011546 ) ) ;
#9478 = CARTESIAN_POINT ( 'NONE',  ( 86.59338513520690128, -0.7688615754554688486, -5.609335628161745468 ) ) ;
#9479 = ADVANCED_FACE ( 'NONE', ( #3848 ), #9582, .T. ) ;
#9480 = VERTEX_POINT ( 'NONE', #547 ) ;
#9481 = CARTESIAN_POINT ( 'NONE',  ( -57.02355111755381500, 29.45914411650387166, 1.982879248426694607 ) ) ;
#9483 = EDGE_CURVE ( 'NONE', #34557, #28485, #23039, .T. ) ;
#9482 = CARTESIAN_POINT ( 'NONE',  ( -80.16840965959801224, -6.651026884041253417, -3.846849152753851087 ) ) ;
#9484 = LINE ( 'NONE', #16479, #19397 ) ;
#9485 = DIRECTION ( 'NONE',  ( 0.000000000000000000, 0.000000000000000000, 1.000000000000000000 ) ) ;
#9486 = B_SPLINE_CURVE_WITH_KNOTS ( 'NONE', 3,
 ( #8220, #37049, #27780, #23869, #33783, #15023, #27586, #17479, #5560, #8023, #39522, #21419, #18101, #1883, #27377, #33583, #20791, #36851, #14809, #39940, #36648, #24289, #30897, #20579, #26977, #4952, #30692, #40138, #2499, #36445, #24494 ),
 .UNSPECIFIED., .F., .F.,
 ( 4, 3, 3, 3, 3, 3, 3, 3, 3, 3, 4 ),
 ( 8.673617379884035472E-19, 3.077658087705547241E-05, 6.152638666999100904E-05, 9.267501192706544444E-05, 0.0001241882240135173282, 0.0001556618703051625174, 0.0001866161554452157713, 0.0002167966385860940542, 0.0002463805737537739116, 0.0002758761370306490207, 0.0002847094172289989233 ),
 .UNSPECIFIED. ) ;
#9487 = VERTEX_POINT ( 'NONE', #16559 ) ;
#9488 = FACE_BOUND ( 'NONE', #39871, .T. ) ;
#9489 = CARTESIAN_POINT ( 'NONE',  ( 3.900618212833813825, -32.29189216196311918, 6.870737987065012042 ) ) ;
#9490 = ORIENTED_EDGE ( 'NONE', *, *, #11698, .T. ) ;
#9491 = CARTESIAN_POINT ( 'NONE',  ( 22.89740935448892500, 4.239003498654196456, 3.174338064556351924 ) ) ;
#9492 = CARTESIAN_POINT ( 'NONE',  ( 78.69031774315028827, 66.05854625464691310, -1.008685033153519983 ) ) ;
#9494 = AXIS2_PLACEMENT_3D ( 'NONE', #38343, #22730, #36091 ) ;
#9493 = CARTESIAN_POINT ( 'NONE',  ( 81.19486284036338475, 61.45157923659407828, 1.862141363775751568 ) ) ;
#9495 = AXIS2_PLACEMENT_3D ( 'NONE', #19450, #19246, #18833 ) ;
#9496 = DIRECTION ( 'NONE',  ( -1.000000000000000000, 1.789409696614061553E-15, 0.000000000000000000 ) ) ;
#9497 = ORIENTED_EDGE ( 'NONE', *, *, #20088, .T. ) ;
#9498 = CARTESIAN_POINT ( 'NONE',  ( 78.14662766244079251, 60.27555255246366528, -2.661196496289815805 ) ) ;
#9499 = B_SPLINE_CURVE_WITH_KNOTS ( 'NONE', 3,
 ( #27389, #40151, #9261, #34009 ),
 .UNSPECIFIED., .F., .F.,
 ( 4, 4 ),
 ( 0.000000000000000000, 6.391136169992404037E-06 ),
 .UNSPECIFIED. ) ;
#9500 = CARTESIAN_POINT ( 'NONE',  ( 14.64821644803149425, 12.77550546983412438, -2.492606463805589811 ) ) ;
#9502 = FACE_OUTER_BOUND ( 'NONE', #14136, .T. ) ;
#9501 = CARTESIAN_POINT ( 'NONE',  ( 2.343537225896455745, -33.01033157941493101, 7.695279973900954751 ) ) ;
#9503 = CARTESIAN_POINT ( 'NONE',  ( 19.21949373037735853, 7.325913195097914610, -3.173010411643660600 ) ) ;
#9504 = CARTESIAN_POINT ( 'NONE',  ( 81.24750358194775401, 61.36520210808431841, -1.450104216466346907 ) ) ;
#9505 = CARTESIAN_POINT ( 'NONE',  ( 77.99575034756946934, 63.53025565730434465, 3.710351296122897491 ) ) ;
#9506 = ORIENTED_EDGE ( 'NONE', *, *, #11092, .T. ) ;
#9507 = VECTOR ( 'NONE', #29504, 999.9999999999998863 ) ;
#9508 = CARTESIAN_POINT ( 'NONE',  ( -24.87867591359218977, -24.55319635012989110, 6.800000000000000711 ) ) ;
#9509 = CARTESIAN_POINT ( 'NONE',  ( 0.5342690456537854127, -32.86995697391282079, 7.720710062488888248 ) ) ;
#9510 = CARTESIAN_POINT ( 'NONE',  ( 79.87389178145707547, 66.27500989097907791, 1.700667878122441801 ) ) ;
#9512 = DIRECTION ( 'NONE',  ( -0.9880385148181951571, 0.000000000000000000, -0.1542073060391599970 ) ) ;
#9511 = CARTESIAN_POINT ( 'NONE',  ( 4.256713912089230334, -31.96058041568350916, 6.980586498568968068 ) ) ;
#9513 = CARTESIAN_POINT ( 'NONE',  ( 27.87470673840761037, 2.608020033772324275, -0.5247038454205935620 ) ) ;
#9514 = EDGE_CURVE ( 'NONE', #9410, #3866, #35338, .T. ) ;
#9515 = DIRECTION ( 'NONE',  ( 0.000000000000000000, 0.000000000000000000, 1.000000000000000000 ) ) ;
#9516 = FACE_OUTER_BOUND ( 'NONE', #10797, .T. ) ;
#9517 = CARTESIAN_POINT ( 'NONE',  ( -64.58420500176730172, 36.29544061437457003, 5.991211914497711177 ) ) ;
#9518 = CARTESIAN_POINT ( 'NONE',  ( 4.697119935056596418, -31.35014961918641063, 7.785096263473213263 ) ) ;
#9519 = CARTESIAN_POINT ( 'NONE',  ( -0.6299129325132426516, -32.04575989041425998, 7.006423389747790331 ) ) ;
#9520 = LINE ( 'NONE', #6455, #25620 ) ;
#9521 = CARTESIAN_POINT ( 'NONE',  ( 34.78019789095738901, -3.716936043298515457, -5.478546665663536430 ) ) ;
#9522 = CARTESIAN_POINT ( 'NONE',  ( 3.442434176459446160, -26.65012155745640499, 6.894806418505343260 ) ) ;
#9523 = CARTESIAN_POINT ( 'NONE',  ( 1.715724685556488494, -33.06989670050605667, 7.637894019485640840 ) ) ;
#9524 = CARTESIAN_POINT ( 'NONE',  ( 14.74700808699402899, -4.436407246566614226, -2.508025288350517634 ) ) ;
#9525 = DIRECTION ( 'NONE',  ( 0.000000000000000000, 1.000000000000000000, 0.000000000000000000 ) ) ;
#9526 = CARTESIAN_POINT ( 'NONE',  ( 0.9074459145065832955, -26.15392167357531505, 7.139344958878411695 ) ) ;
#9527 = CARTESIAN_POINT ( 'NONE',  ( -63.03213158086148837, 38.26878225442760595, -4.032857076800603124 ) ) ;
#9528 = ADVANCED_FACE ( 'NONE', ( #10392 ), #28528, .F. ) ;
#9529 = CIRCLE ( 'NONE', #39079, 5.950000000000010836 ) ;
#9530 = CARTESIAN_POINT ( 'NONE',  ( -1.506684114051581647, -28.44091511309124343, 7.695279973900954751 ) ) ;
#9531 = AXIS2_PLACEMENT_3D ( 'NONE', #14115, #35964, #35575 ) ;
#9532 = DIRECTION ( 'NONE',  ( -0.000000000000000000, -0.000000000000000000, 1.000000000000000000 ) ) ;
#9534 = ORIENTED_EDGE ( 'NONE', *, *, #34294, .F. ) ;
#9533 = VECTOR ( 'NONE', #692, 1000.000000000000000 ) ;
#9535 = EDGE_LOOP ( 'NONE', ( #25708, #22393, #23264, #37698 ) ) ;
#9536 = CARTESIAN_POINT ( 'NONE',  ( -53.21549048184568420, -38.28842912540938670, 4.000000000000000000 ) ) ;
#9537 = CARTESIAN_POINT ( 'NONE',  ( 68.77554901931263487, 58.16923054873410592, -3.957896739784567686 ) ) ;
#9538 = VECTOR ( 'NONE', #27572, 1000.000000000000000 ) ;
#9539 = ORIENTED_EDGE ( 'NONE', *, *, #36865, .F. ) ;
#9540 = DIRECTION ( 'NONE',  ( -0.000000000000000000, -1.000000000000000000, -0.000000000000000000 ) ) ;
#9542 = EDGE_CURVE ( 'NONE', #18906, #33368, #28715, .T. ) ;
#9541 = DIRECTION ( 'NONE',  ( 0.000000000000000000, 1.000000000000000000, 0.000000000000000000 ) ) ;
#9543 = CARTESIAN_POINT ( 'NONE',  ( 22.02762008288383200, 3.976027453218988317, 4.186289093362514535 ) ) ;
#9544 = CARTESIAN_POINT ( 'NONE',  ( 5.043486035277081392, -28.53373062621871981, 6.895394898881670009 ) ) ;
#9545 = CARTESIAN_POINT ( 'NONE',  ( 1.081163097807408935, -26.22679299245623952, 7.730758795053809251 ) ) ;
#9546 = CARTESIAN_POINT ( 'NONE',  ( 5.045119861038438458, -30.18056701569746281, 7.779495906702012853 ) ) ;
#9547 = ORIENTED_EDGE ( 'NONE', *, *, #7574, .T. ) ;
#9548 = CARTESIAN_POINT ( 'NONE',  ( 21.98934069226735133, 5.611891575985531233, 3.092273232226271595 ) ) ;
#9549 = DIRECTION ( 'NONE',  ( 0.9982280052159038242, 0.000000000000000000, 0.05950503846463438273 ) ) ;
#9550 = DIRECTION ( 'NONE',  ( 1.000000000000000000, 0.000000000000000000, 0.000000000000000000 ) ) ;
#9551 = VERTEX_POINT ( 'NONE', #20662 ) ;
#9552 = CARTESIAN_POINT ( 'NONE',  ( 80.39617744327613025, 62.02891139109912189, -3.151254463355007918 ) ) ;
#9554 = CARTESIAN_POINT ( 'NONE',  ( -1.677244393547275392, -29.95926971864756538, 6.988553391373224066 ) ) ;
#9553 = CARTESIAN_POINT ( 'NONE',  ( 22.71567147354432237, 0.3624905230350064511, 6.349376209889807221 ) ) ;
#9555 = CARTESIAN_POINT ( 'NONE',  ( 79.06287735990343890, 66.15384612320052327, -1.644402879615785684 ) ) ;
#9556 = CARTESIAN_POINT ( 'NONE',  ( 79.42292528565204179, 64.10449580132842584, 3.686141857899477348 ) ) ;
#9557 = ORIENTED_EDGE ( 'NONE', *, *, #39077, .F. ) ;
#9558 = EDGE_CURVE ( 'NONE', #2658, #20612, #39169, .T. ) ;
#9559 = AXIS2_PLACEMENT_3D ( 'NONE', #13977, #19955, #32737 ) ;
#9560 = AXIS2_PLACEMENT_3D ( 'NONE', #21767, #34350, #34147 ) ;
#9561 = CARTESIAN_POINT ( 'NONE',  ( -1.586324960283478580, -30.75679626155069712, 7.773839561854631874 ) ) ;
#9563 = EDGE_LOOP ( 'NONE', ( #12441, #23352, #6780, #35383 ) ) ;
#9562 = CARTESIAN_POINT ( 'NONE',  ( 4.361462012329716309, -31.84340686930758935, 6.894806418505347700 ) ) ;
#9564 = CARTESIAN_POINT ( 'NONE',  ( 21.85643539959776049, -3.145688729744653411, 12.47482453294728266 ) ) ;
#9565 = CARTESIAN_POINT ( 'NONE',  ( 1.139664070701874143, -33.03161420323011299, 7.255881584735162093 ) ) ;
#9566 = ORIENTED_EDGE ( 'NONE', *, *, #8264, .T. ) ;
#9567 = CARTESIAN_POINT ( 'NONE',  ( -75.35262966362313364, 8.291683080040980869, 9.005052742938818966 ) ) ;
#9568 = CARTESIAN_POINT ( 'NONE',  ( 36.07971702944216474, -3.672696443019492829, 5.688510560309873121 ) ) ;
#9569 = ORIENTED_EDGE ( 'NONE', *, *, #27926, .F. ) ;
#9570 = VECTOR ( 'NONE', #20305, 1000.000000000000000 ) ;
#9571 = FACE_BOUND ( 'NONE', #1093, .T. ) ;
#9572 = CARTESIAN_POINT ( 'NONE',  ( 3.435265683109236967, -26.53015935524666347, 7.750000000000001776 ) ) ;
#9573 = CARTESIAN_POINT ( 'NONE',  ( 36.68636550425712528, -1.913427295981317888, -5.802400637960247742 ) ) ;
#9574 = CARTESIAN_POINT ( 'NONE',  ( -1.553683706606911130, -30.55532538593644176, 7.013842709614101167 ) ) ;
#9575 = DIRECTION ( 'NONE',  ( 0.000000000000000000, 0.000000000000000000, 1.000000000000000000 ) ) ;
#9576 = CARTESIAN_POINT ( 'NONE',  ( 22.37810747204872897, 5.219580669678665963, 3.555984268806748894 ) ) ;
#9577 = DIRECTION ( 'NONE',  ( -0.000000000000000000, -0.000000000000000000, 1.000000000000000000 ) ) ;
#9578 = CARTESIAN_POINT ( 'NONE',  ( -7.890026461918810519, -29.56993018339340651, 6.000000000000000000 ) ) ;
#9579 = ADVANCED_FACE ( 'NONE', ( #32436 ), #1544, .F. ) ;
#9580 = CARTESIAN_POINT ( 'NONE',  ( -59.87552183813129147, 24.84364830758654108, -9.681005660250225020 ) ) ;
#9581 = EDGE_CURVE ( 'NONE', #25156, #25120, #11384, .T. ) ;
#9582 = CYLINDRICAL_SURFACE ( 'NONE', #5271, 3.399999999999999911 ) ;
#9583 = CARTESIAN_POINT ( 'NONE',  ( 24.35854945548016914, 1.282877579546743307, -4.712861751322592774 ) ) ;
#9584 = CARTESIAN_POINT ( 'NONE',  ( 31.38981853733673688, -3.758192538165083807, -4.681675008679978767 ) ) ;
#9585 = LINE ( 'NONE', #19673, #26871 ) ;
#9586 = EDGE_LOOP ( 'NONE', ( #21719, #25247 ) ) ;
#9587 = CARTESIAN_POINT ( 'NONE',  ( 67.51854282697247811, 57.96351248157043301, 3.990882853436548139 ) ) ;
#9588 = CARTESIAN_POINT ( 'NONE',  ( 29.13956619203430520, 0.4692469261591867280, 4.754332065975193977 ) ) ;
#9589 = CARTESIAN_POINT ( 'NONE',  ( 3.325856478880445000, -25.14347697372913615, 7.635761828346577573 ) ) ;
#9590 = VECTOR ( 'NONE', #18599, 1000.000000000000000 ) ;
#9591 = CARTESIAN_POINT ( 'NONE',  ( 85.73014479007146349, 1.298542115207370173, 5.666065989068760800 ) ) ;
#9592 = EDGE_CURVE ( 'NONE', #33929, #8738, #14077, .T. ) ;
#9593 = CARTESIAN_POINT ( 'NONE',  ( 21.67220405017981122, 6.675115239655725397, 3.070808856021292499 ) ) ;
#9594 = VERTEX_POINT ( 'NONE', #26454 ) ;
#9595 = CARTESIAN_POINT ( 'NONE',  ( 24.60366954196197042, 2.981655850978834899, 3.555329962009686540 ) ) ;
#9596 = VECTOR ( 'NONE', #14219, 1000.000000000000114 ) ;
#9597 = CARTESIAN_POINT ( 'NONE',  ( 5.200364047366366371, -29.55642757665872722, 7.635761828346577573 ) ) ;
#9598 = CARTESIAN_POINT ( 'NONE',  ( 0.03153883250375685843, -32.53218194000729113, 7.691066658568948000 ) ) ;
#9599 = VERTEX_POINT ( 'NONE', #13692 ) ;
#9600 = DIRECTION ( 'NONE',  ( 0.000000000000000000, 0.000000000000000000, 1.000000000000000000 ) ) ;
#9601 = B_SPLINE_CURVE_WITH_KNOTS ( 'NONE', 3,
 ( #39852, #5471, #36361, #8128, #30602, #11824, #27089, #11421, #20699, #4663, #8544, #2411, #33282, #20910, #23596, #14713, #27500, #27287, #17199, #5063, #24199, #21125, #29766, #30176, #26691, #2195, #17596, #1997, #14315, #39635, #24408 ),
 .UNSPECIFIED., .F., .F.,
 ( 4, 3, 3, 3, 3, 3, 3, 3, 3, 3, 4 ),
 ( 1.226634733346699349E-18, 2.999644130997734673E-05, 6.002588995694668750E-05, 8.960886084587991768E-05, 0.0001190604700446490252, 0.0001489538463052708802, 0.0001796139255493970418, 0.0002109707048517072412, 0.0002426195318110355734, 0.0002740640997890037987, 0.0002849778069099845822 ),
 .UNSPECIFIED. ) ;
#9602 = ORIENTED_EDGE ( 'NONE', *, *, #15605, .F. ) ;
#9603 = CARTESIAN_POINT ( 'NONE',  ( 80.97051285240276286, 61.23143294393121039, -1.429680343939067955 ) ) ;
#9604 = CARTESIAN_POINT ( 'NONE',  ( 80.61389980387333765, 62.62535450461751907, 3.411701596789205926 ) ) ;
#9607 = EDGE_LOOP ( 'NONE', ( #22493, #32848, #12088, #20513, #15602 ) ) ;
#9606 = EDGE_LOOP ( 'NONE', ( #25485, #22065, #30408, #23677, #31376 ) ) ;
#9605 = CARTESIAN_POINT ( 'NONE',  ( -0.8622465457266019762, -27.33543793757026918, 6.880147297696980857 ) ) ;
#9608 = LINE ( 'NONE', #13297, #29469 ) ;
#9609 = CARTESIAN_POINT ( 'NONE',  ( 0.04256582245634059347, -26.49275466612191110, 7.771081512783703182 ) ) ;
#9610 = CARTESIAN_POINT ( 'NONE',  ( -0.5240808859923175023, -32.27210411901214826, 7.720710062488896241 ) ) ;
#9611 = PLANE ( 'NONE',  #13673 ) ;
#9612 = CARTESIAN_POINT ( 'NONE',  ( 1.700390093233090871, -29.56993018339339940, 7.800000000000000711 ) ) ;
#9613 = CARTESIAN_POINT ( 'NONE',  ( 24.05436622899220822, 3.340017053445958783, -3.241057297173068452 ) ) ;
#9614 = ORIENTED_EDGE ( 'NONE', *, *, #15999, .F. ) ;
#9615 = EDGE_LOOP ( 'NONE', ( #21517, #27075, #5568, #1859 ) ) ;
#9616 = CARTESIAN_POINT ( 'NONE',  ( -0.9352292415849461360, -31.71783863626873767, 6.894806418505345924 ) ) ;
#9617 = CARTESIAN_POINT ( 'NONE',  ( -65.33937732661031816, 36.44481994370828914, 7.201454646438380180 ) ) ;
#9618 = ADVANCED_FACE ( 'NONE', ( #10587 ), #4233, .F. ) ;
#9619 = CARTESIAN_POINT ( 'NONE',  ( -79.08083519856748467, -5.497992658161905410, -5.845328771210035690 ) ) ;
#9620 = CARTESIAN_POINT ( 'NONE',  ( 5.005904147265696658, -30.36590558413950802, 6.959317978105167057 ) ) ;
#9621 = CARTESIAN_POINT ( 'NONE',  ( 79.27186652256901311, 65.93364065454110801, 2.332991218130493039 ) ) ;
#9622 = CARTESIAN_POINT ( 'NONE',  ( 87.51701825761838904, -2.015745416966476800, -3.511549023785576651 ) ) ;
#9623 = CARTESIAN_POINT ( 'NONE',  ( -58.99872204295123623, 28.48507918597134037, -46.17089178453873188 ) ) ;
#9624 = EDGE_LOOP ( 'NONE', ( #21860, #37898, #2487, #37598 ) ) ;
#9625 = CARTESIAN_POINT ( 'NONE',  ( -64.09291719262364495, 35.65918410775120861, -4.099820839135469797 ) ) ;
#9626 = DIRECTION ( 'NONE',  ( -2.699830798738917390E-13, 1.000000000000000000, 0.000000000000000000 ) ) ;
#9627 =( GEOMETRIC_REPRESENTATION_CONTEXT ( 3 ) GLOBAL_UNCERTAINTY_ASSIGNED_CONTEXT ( ( #39873 ) ) GLOBAL_UNIT_ASSIGNED_CONTEXT ( ( #2598, #27480, #5247 ) ) REPRESENTATION_CONTEXT ( 'NONE', 'WORKASPACE' ) );
#9628 = AXIS2_PLACEMENT_3D ( 'NONE', #24300, #3482, #11725 ) ;
#9629 = ADVANCED_FACE ( 'NONE', ( #23950 ), #10781, .F. ) ;
#9630 = PRODUCT_RELATED_PRODUCT_CATEGORY ( 'part', '', ( #26257 ) ) ;
#9631 = CARTESIAN_POINT ( 'NONE',  ( 1.687546834072821023, -26.16994927825320971, 7.756377446753164762 ) ) ;
#9632 = FACE_OUTER_BOUND ( 'NONE', #12685, .T. ) ;
#9633 = DIRECTION ( 'NONE',  ( -1.000000000000000000, 0.000000000000000000, 0.000000000000000000 ) ) ;
#9634 = CARTESIAN_POINT ( 'NONE',  ( 85.58015388280458069, 1.007655178167426335, 5.787227695588894605 ) ) ;
#9635 = AXIS2_PLACEMENT_3D ( 'NONE', #16683, #13613, #10516 ) ;
#9636 = VERTEX_POINT ( 'NONE', #8297 ) ;
#9637 = CARTESIAN_POINT ( 'NONE',  ( 36.14155268336735816, -3.142484588683069902, 5.847161401630891042 ) ) ;
#9638 = CARTESIAN_POINT ( 'NONE',  ( 87.09859342968812257, 0.5244505078549105415, -5.068689133590885909 ) ) ;
#9639 = VERTEX_POINT ( 'NONE', #16758 ) ;
#9641 = CARTESIAN_POINT ( 'NONE',  ( 14.75078054601031674, -5.140699092989589047, 2.499999999999999556 ) ) ;
#9640 = CARTESIAN_POINT ( 'NONE',  ( 81.17453961776598703, 62.25628865055540473, -2.899379378185768630 ) ) ;
#9642 = CARTESIAN_POINT ( 'NONE',  ( 2.921117467371362242, -32.85015253290869452, 7.651421919295145813 ) ) ;
#9643 = ORIENTED_EDGE ( 'NONE', *, *, #26729, .F. ) ;
#9644 = CARTESIAN_POINT ( 'NONE',  ( -1.642565866964522225, -28.94973227290090989, 7.782167645815903256 ) ) ;
#9645 = CARTESIAN_POINT ( 'NONE',  ( -0.4769030174555436985, -26.84268727337696703, 7.780491323090171996 ) ) ;
#9646 = VERTEX_POINT ( 'NONE', #7504 ) ;
#9647 = CARTESIAN_POINT ( 'NONE',  ( -80.55887061931086635, -6.632148677064343190, 2.726002644713694245 ) ) ;
#9648 = CIRCLE ( 'NONE', #5712, 3.784187430299790211 ) ;
#9649 = ORIENTED_EDGE ( 'NONE', *, *, #7946, .F. ) ;
#9650 = CARTESIAN_POINT ( 'NONE',  ( 79.44161963160777873, 65.18980684700308359, -3.197674131580387602 ) ) ;
#9651 = CARTESIAN_POINT ( 'NONE',  ( 36.06236019073843835, -3.149134278961357225, 5.834801497878530085 ) ) ;
#9652 = AXIS2_PLACEMENT_3D ( 'NONE', #1685, #23099, #20589 ) ;
#9654 = CARTESIAN_POINT ( 'NONE',  ( 37.20488407139969667, -2.771826426831375034, 5.999999980036296421 ) ) ;
#9653 = CARTESIAN_POINT ( 'NONE',  ( 24.64370639163859522, 1.605171026338595430, 4.497401421240313724 ) ) ;
#9656 = ORIENTED_EDGE ( 'NONE', *, *, #5344, .T. ) ;
#9655 = VERTEX_POINT ( 'NONE', #20067 ) ;
#9657 = AXIS2_PLACEMENT_3D ( 'NONE', #5849, #16118, #38536 ) ;
#9658 = CARTESIAN_POINT ( 'NONE',  ( 81.73829655978374831, 61.84901640042586024, -1.708467252431210115 ) ) ;
#9659 = CARTESIAN_POINT ( 'NONE',  ( -75.45330471031414277, 33.71485196875532608, 12.50000000000000000 ) ) ;
#9661 = DIRECTION ( 'NONE',  ( 0.000000000000000000, 0.000000000000000000, 1.000000000000000000 ) ) ;
#9660 = CARTESIAN_POINT ( 'NONE',  ( -22.97867591359219119, -26.64985754041175525, 6.800000000000000711 ) ) ;
#9662 = DIRECTION ( 'NONE',  ( 0.000000000000000000, 0.7126435865141257375, 0.7015262779114433966 ) ) ;
#9663 = CARTESIAN_POINT ( 'NONE',  ( -63.16166472087058992, 41.43483297117672493, -4.000000000000000000 ) ) ;
#9664 = CARTESIAN_POINT ( 'NONE',  ( 71.58333764992288195, 61.16654152266917066, 3.647993048544889039 ) ) ;
#9665 = CARTESIAN_POINT ( 'NONE',  ( 24.13014922190525624, 2.944621410230606529, -3.777319215821884235 ) ) ;
#9666 = EDGE_LOOP ( 'NONE', ( #38219, #93, #11869, #32160 ) ) ;
#9667 = EDGE_CURVE ( 'NONE', #9413, #19825, #38040, .T. ) ;
#9668 = VERTEX_POINT ( 'NONE', #39819 ) ;
#9669 = CARTESIAN_POINT ( 'NONE',  ( 21.85643539959774273, 9.172641120068929510, -1.679843024921975347 ) ) ;
#9670 = EDGE_CURVE ( 'NONE', #33153, #28854, #21346, .T. ) ;
#9671 = CARTESIAN_POINT ( 'NONE',  ( 3.554700302571109916, -26.60177950712765593, 7.754798119455333705 ) ) ;
#9672 = CARTESIAN_POINT ( 'NONE',  ( 1.686887486498407140, -26.06995622926011436, 7.635761828346576685 ) ) ;
#9673 = CARTESIAN_POINT ( 'NONE',  ( 81.67965074903510470, 61.82017115420521947, 1.781440269582215352 ) ) ;
#9674 = CARTESIAN_POINT ( 'NONE',  ( 87.15505355144220800, 0.4610318193416703680, -5.246243280819175681 ) ) ;
#9675 = ORIENTED_EDGE ( 'NONE', *, *, #37330, .T. ) ;
#9676 = ADVANCED_FACE ( 'NONE', ( #24576 ), #40213, .F. ) ;
#9677 = CARTESIAN_POINT ( 'NONE',  ( 14.67325355196695646, 12.62073864643243226, 2.499999999998588240 ) ) ;
#9678 = CARTESIAN_POINT ( 'NONE',  ( 21.52542566397378820, -2.894605234475977618, 3.543787706140388849 ) ) ;
#9679 = AXIS2_PLACEMENT_3D ( 'NONE', #24924, #9256, #34413 ) ;
#9680 = EDGE_CURVE ( 'NONE', #20773, #19906, #2781, .T. ) ;
#9681 = CARTESIAN_POINT ( 'NONE',  ( 36.44671748466953431, -2.355057832951331420, -5.894789749312875138 ) ) ;
#9682 = CARTESIAN_POINT ( 'NONE',  ( 5.140321331941717808, -29.00739657781303293, 7.785096263473213263 ) ) ;
#9683 = CARTESIAN_POINT ( 'NONE',  ( 21.81726414084884169, 5.354314201170920384, 3.565644528639963617 ) ) ;
#9684 = B_SPLINE_CURVE_WITH_KNOTS ( 'NONE', 3,
 ( #14744, #8573, #36589, #15164, #12063, #24013, #24642, #33718, #20728, #5497, #33524, #40277, #8365, #2441, #33101, #21358, #40080, #18248, #23808, #14962, #20938, #11858, #30837, #2647, #4886, #27722, #37193, #17417, #5294, #1819, #30415 ),
 .UNSPECIFIED., .F., .F.,
 ( 4, 3, 3, 3, 3, 3, 3, 3, 3, 3, 4 ),
 ( 6.484403375994506654E-05, 8.983333709522423050E-05, 0.0001203539973219388106, 0.0001514144607149688852, 0.0001828916862241641297, 0.0002144221682127289306, 0.0002455195857862220790, 0.0002758614570916278607, 0.0003055381793602574415, 0.0003350143730643698843, 0.0003497271997307904268 ),
 .UNSPECIFIED. ) ;
#9685 = CARTESIAN_POINT ( 'NONE',  ( -1.078675913592196167, -24.55319635012989110, 6.800000000000000711 ) ) ;
#9686 = VERTEX_POINT ( 'NONE', #12425 ) ;
#9687 = CARTESIAN_POINT ( 'NONE',  ( 4.620198719170100610, -31.31197426661971761, 6.894806418505346812 ) ) ;
#9688 = AXIS2_PLACEMENT_3D ( 'NONE', #38526, #19203, #22711 ) ;
#9689 = AXIS2_PLACEMENT_3D ( 'NONE', #38653, #31899, #25910 ) ;
#9690 = B_SPLINE_CURVE_WITH_KNOTS ( 'NONE', 3,
 ( #21879, #6233, #34666, #35069, #9509, #6444, #31354, #3776, #9721, #22505 ),
 .UNSPECIFIED., .F., .F.,
 ( 4, 3, 3, 4 ),
 ( 0.0001585009270395679984, 0.0001815657551981835979, 0.0002118214035944133186, 0.0002170292169044720973 ),
 .UNSPECIFIED. ) ;
#9691 = DIRECTION ( 'NONE',  ( 1.000000000000000000, 0.000000000000000000, -0.000000000000000000 ) ) ;
#9692 = CARTESIAN_POINT ( 'NONE',  ( 30.68797926878130866, -2.925629016318143538, 4.995999375113326479 ) ) ;
#9693 = ORIENTED_EDGE ( 'NONE', *, *, #35111, .F. ) ;
#9694 = CARTESIAN_POINT ( 'NONE',  ( 34.14220566676094393, -3.846217302993689469, 5.236774695382229616 ) ) ;
#9695 = CARTESIAN_POINT ( 'NONE',  ( 4.638101942922436827, -27.85824998890764448, 7.635761828346577573 ) ) ;
#9696 = CARTESIAN_POINT ( 'NONE',  ( 1.756997582572583649, -26.17040145250279437, 6.887041543973315250 ) ) ;
#9697 = B_SPLINE_CURVE_WITH_KNOTS ( 'NONE', 3,
 ( #8666, #9082, #2119, #36886, #27812, #2323, #21245, #21660, #40365, #18139 ),
 .UNSPECIFIED., .F., .F.,
 ( 4, 2, 2, 2, 4 ),
 ( 0.000000000000000000, 0.0003915860703966792910, 0.0007831721407933585821, 0.001174758211190037819, 0.001566344281586717164 ),
 .UNSPECIFIED. ) ;
#9698 = CARTESIAN_POINT ( 'NONE',  ( 66.41209187282781556, 57.81891248311885079, -4.000000000000025757 ) ) ;
#9699 = ORIENTED_EDGE ( 'NONE', *, *, #23579, .F. ) ;
#9700 = FACE_OUTER_BOUND ( 'NONE', #34394, .T. ) ;
#9701 = CARTESIAN_POINT ( 'NONE',  ( -76.19356073596259193, 10.47839387954511814, -8.503801285675736565 ) ) ;
#9702 = VERTEX_POINT ( 'NONE', #18389 ) ;
#9703 = CARTESIAN_POINT ( 'NONE',  ( 3.922483456672744673, -26.86580350659783178, 7.695279973900954751 ) ) ;
#9704 = FILL_AREA_STYLE ('',( #22487 ) ) ;
#9705 = EDGE_LOOP ( 'NONE', ( #32622, #12517, #34614, #1947, #3725, #5973 ) ) ;
#9706 = CARTESIAN_POINT ( 'NONE',  ( 22.90651681474014012, 4.202743079833220818, 3.210710377858703168 ) ) ;
#9707 = CARTESIAN_POINT ( 'NONE',  ( 82.50731566719292687, 63.18365725368101238, -1.509105202935689283 ) ) ;
#9708 = CARTESIAN_POINT ( 'NONE',  ( 80.72314371186318738, 62.66258842508748472, 3.386558198656121732 ) ) ;
#9709 = PLANE ( 'NONE',  #29834 ) ;
#9710 = ORIENTED_EDGE ( 'NONE', *, *, #32336, .F. ) ;
#9711 = CARTESIAN_POINT ( 'NONE',  ( 77.19967638839698054, 62.30393748795767550, -3.856837490695292026 ) ) ;
#9713 = LINE ( 'NONE', #18771, #22387 ) ;
#9712 = CARTESIAN_POINT ( 'NONE',  ( 3.901153242843497626, -32.27259905789637173, 7.785344483711591934 ) ) ;
#9714 = CARTESIAN_POINT ( 'NONE',  ( 16.54063652338793133, 10.02979042668312992, -2.737642957281533729 ) ) ;
#9715 = CARTESIAN_POINT ( 'NONE',  ( 79.29849762269610380, 65.95036606079992225, -2.316472630215912876 ) ) ;
#9716 = CARTESIAN_POINT ( 'NONE',  ( 79.26824131213427904, 60.90178692369119062, 2.725046208697147421 ) ) ;
#9717 = VECTOR ( 'NONE', #29031, 1000.000000000000000 ) ;
#9718 = ORIENTED_EDGE ( 'NONE', *, *, #28547, .T. ) ;
#9719 = VECTOR ( 'NONE', #34543, 1000.000000000000000 ) ;
#9720 = CARTESIAN_POINT ( 'NONE',  ( -9.741734729663692249, 54.65020406074287251, 1.000000000000000000 ) ) ;
#9721 = CARTESIAN_POINT ( 'NONE',  ( 0.5371711504799124848, -32.87097875789517332, 7.697032948437506406 ) ) ;
#9722 = CARTESIAN_POINT ( 'NONE',  ( 81.16905975791091521, 61.30379048835199995, 1.022614849746394938 ) ) ;
#9724 = CARTESIAN_POINT ( 'NONE',  ( 19.55994146243534715, 8.628030923317455247, 2.499999999993585575 ) ) ;
#9723 = FACE_OUTER_BOUND ( 'NONE', #9086, .T. ) ;
#9725 = CARTESIAN_POINT ( 'NONE',  ( 27.31903677934867147, 0.4900422023718347675, -5.740875207198388175 ) ) ;
#9726 = CARTESIAN_POINT ( 'NONE',  ( -1.396386647739597420, -31.20089878032661801, 6.870724624169666228 ) ) ;
#9727 = DIRECTION ( 'NONE',  ( -1.000000000000000000, 0.000000000000000000, 0.000000000000000000 ) ) ;
#9728 = CARTESIAN_POINT ( 'NONE',  ( 1.515152310805649938, -33.06502611812176440, 6.989977667959446528 ) ) ;
#9729 = EDGE_CURVE ( 'NONE', #21194, #28994, #37084, .T. ) ;
#9730 = DIRECTION ( 'NONE',  ( -0.1736481776669340227, 0.9848077530122073542, -0.000000000000000000 ) ) ;
#9731 = CARTESIAN_POINT ( 'NONE',  ( -0.6258329412763763422, -32.04959131907094161, 6.895222827070021765 ) ) ;
#9732 = CARTESIAN_POINT ( 'NONE',  ( -1.242570340174825594, -27.67546881208082965, 7.013842709614101167 ) ) ;
#9733 = EDGE_CURVE ( 'NONE', #6110, #38497, #36724, .T. ) ;
#9734 = CARTESIAN_POINT ( 'NONE',  ( -36.87867591359218977, -24.55319635012989110, 6.700000000000000178 ) ) ;
#9735 = CARTESIAN_POINT ( 'NONE',  ( 35.56295975436646017, -1.640838707923856443, -5.744612369613007807 ) ) ;
#9736 = CARTESIAN_POINT ( 'NONE',  ( 78.20266744111994228, 60.29550935153869062, -2.640515453965961878 ) ) ;
#9737 = CARTESIAN_POINT ( 'NONE',  ( 4.362817617720858188, -27.29804117271309138, 7.730015791551950954 ) ) ;
#9738 =( BOUNDED_CURVE ( )  B_SPLINE_CURVE ( 3, ( #12652, #9565, #22145, #6496 ),
 .UNSPECIFIED., .F., .T. ) 
 B_SPLINE_CURVE_WITH_KNOTS ( ( 4, 4 ),
 ( 1.347909859412854683, 1.534781240595300078 ),
 .UNSPECIFIED. ) 
 CURVE ( )  GEOMETRIC_REPRESENTATION_ITEM ( )  RATIONAL_B_SPLINE_CURVE ( ( 1.000000000000000000, 0.9970920404276226723, 0.9970920404276226723, 1.000000000000000000 ) ) 
 REPRESENTATION_ITEM ( '' )  );
#9739 = DIRECTION ( 'NONE',  ( -0.000000000000000000, -0.000000000000000000, 1.000000000000000000 ) ) ;
#9740 = VECTOR ( 'NONE', #19696, 1000.000000000000000 ) ;
#9741 = CARTESIAN_POINT ( 'NONE',  ( 3.428181999189476858, -32.49819505012106902, 7.721096864323904185 ) ) ;
#9742 = CARTESIAN_POINT ( 'NONE',  ( -81.63024932266884548, 10.48199852196216497, 2.292792362136173434 ) ) ;
#9743 = CARTESIAN_POINT ( 'NONE',  ( -36.24874870218063450, -26.64985754041175525, 6.700000000000000178 ) ) ;
#9744 = AXIS2_PLACEMENT_3D ( 'NONE', #39630, #5260, #2190 ) ;
#9745 = CARTESIAN_POINT ( 'NONE',  ( -1.506257772487957336, -28.43970203156576559, 7.712764235869102869 ) ) ;
#9746 = ORIENTED_EDGE ( 'NONE', *, *, #9334, .T. ) ;
#9747 = CARTESIAN_POINT ( 'NONE',  ( -0.2563090734626436440, -34.23573776596825979, 6.894806418505347700 ) ) ;
#9748 = CARTESIAN_POINT ( 'NONE',  ( 68.75960254727382903, 58.21139355255508008, -3.964410623304020387 ) ) ;
#9749 = DIRECTION ( 'NONE',  ( 0.9396926207859105373, 0.3420201433256629397, 0.000000000000000000 ) ) ;
#9750 = VERTEX_POINT ( 'NONE', #8504 ) ;
#9751 = CARTESIAN_POINT ( 'NONE',  ( -0.5769924795711234289, -32.09451502393404354, 7.754798119455333705 ) ) ;
#9752 = LINE ( 'NONE', #13240, #36429 ) ;
#9753 = CARTESIAN_POINT ( 'NONE',  ( 22.84784676164604278, 3.199131945760815832, 4.124430016485445272 ) ) ;
#9754 = DIRECTION ( 'NONE',  ( 0.000000000000000000, 0.000000000000000000, 1.000000000000000000 ) ) ;
#9755 = DIRECTION ( 'NONE',  ( 1.000000000000000000, 0.000000000000000000, 0.000000000000000000 ) ) ;
#9756 = ORIENTED_EDGE ( 'NONE', *, *, #1780, .T. ) ;
#9757 = CARTESIAN_POINT ( 'NONE',  ( 24.06683628570359446, 3.348910172779726135, 3.206004284675357141 ) ) ;
#9758 = CYLINDRICAL_SURFACE ( 'NONE', #14255, 3.499999999999999556 ) ;
#9759 = CARTESIAN_POINT ( 'NONE',  ( 81.13325097526887930, 61.29068799862990602, 1.183438861787475593 ) ) ;
#9760 = EDGE_LOOP ( 'NONE', ( #23476, #12729, #13998, #5770 ) ) ;
#9761 = CARTESIAN_POINT ( 'NONE',  ( -1.194263764872669054, -31.54948795403056394, 7.501983001166817822 ) ) ;
#9762 = ORIENTED_EDGE ( 'NONE', *, *, #32774, .F. ) ;
#9763 = CARTESIAN_POINT ( 'NONE',  ( 78.24936850314311698, 65.65315377296109034, -2.033355767895869359 ) ) ;
#9765 = CARTESIAN_POINT ( 'NONE',  ( -1.676168523076433159, -29.96849248796560872, 6.903372536218459032 ) ) ;
#9764 = CARTESIAN_POINT ( 'NONE',  ( 21.83335788848096115, 0.3052388310511004454, 8.127432559144740054 ) ) ;
#9766 = CARTESIAN_POINT ( 'NONE',  ( 81.58578928044234146, 61.77466459011638733, -1.878604182848718995 ) ) ;
#9767 = CARTESIAN_POINT ( 'NONE',  ( 80.58155366896997407, 61.83530676836470974, 2.934133054905258664 ) ) ;
#9768 = CARTESIAN_POINT ( 'NONE',  ( -1.582528736513596490, -30.78337320113038444, 7.750000000000000000 ) ) ;
#9769 = CARTESIAN_POINT ( 'NONE',  ( -64.08758708074093136, 43.19434570074267299, 2.104943985153647112 ) ) ;
#9770 = CARTESIAN_POINT ( 'NONE',  ( 22.73811350958456501, -4.924115162416450531, 6.814090253401713149 ) ) ;
#9771 = CARTESIAN_POINT ( 'NONE',  ( 3.300479879060630228, -34.00561972003898603, 7.635761828346577573 ) ) ;
#9772 = ORIENTED_EDGE ( 'NONE', *, *, #6620, .F. ) ;
#9773 = CARTESIAN_POINT ( 'NONE',  ( -73.51040120057371041, 5.657262173908669034, 9.719076197244223891 ) ) ;
#9774 = CARTESIAN_POINT ( 'NONE',  ( 0.4551510633898000480, -26.29166087107455496, 7.255881584735164758 ) ) ;
#9775 = ORIENTED_EDGE ( 'NONE', *, *, #34337, .T. ) ;
#9776 = VECTOR ( 'NONE', #37121, 1000.000000000000000 ) ;
#9777 = DIRECTION ( 'NONE',  ( 0.000000000000000000, 0.000000000000000000, 1.000000000000000000 ) ) ;
#9778 = CARTESIAN_POINT ( 'NONE',  ( 1.585236220975464683, -32.96797956292043352, 7.761597726988851420 ) ) ;
#9779 = EDGE_CURVE ( 'NONE', #11094, #27559, #21088, .T. ) ;
#9780 = CARTESIAN_POINT ( 'NONE',  ( 33.44745999691134131, -3.711946420718001516, -5.220912322284510410 ) ) ;
#9781 = CARTESIAN_POINT ( 'NONE',  ( 35.22195622051280139, -1.045642381572828628, -5.409226251924048157 ) ) ;
#9782 = CARTESIAN_POINT ( 'NONE',  ( 3.764702813991775976, -32.27154237255469127, 6.871394612369937427 ) ) ;
#9783 = CARTESIAN_POINT ( 'NONE',  ( -1.000637662739485290, -31.79578935716557453, 6.894806418505347700 ) ) ;
#9784 = CARTESIAN_POINT ( 'NONE',  ( -16.97867591359219475, -26.64985754041175525, 6.800000000000000711 ) ) ;
#9785 = CARTESIAN_POINT ( 'NONE',  ( -36.97867591359219119, -24.55319635012989110, 6.800000000000000711 ) ) ;
#9786 = DIRECTION ( 'NONE',  ( 0.000000000000000000, 0.000000000000000000, 1.000000000000000000 ) ) ;
#9787 = DIRECTION ( 'NONE',  ( 0.000000000000000000, -0.000000000000000000, -1.000000000000000000 ) ) ;
#9788 = CARTESIAN_POINT ( 'NONE',  ( 22.81751159329827772, 0.7919312097182544807, -5.980481906966360839 ) ) ;
#9789 = CARTESIAN_POINT ( 'NONE',  ( 32.00007467492793012, -3.767639907337460237, -4.802642618328528457 ) ) ;
#9790 = AXIS2_PLACEMENT_3D ( 'NONE', #29266, #35854, #4365 ) ;
#9791 = DIRECTION ( 'NONE',  ( 0.000000000000000000, 0.000000000000000000, 1.000000000000000000 ) ) ;
#9792 = ORIENTED_EDGE ( 'NONE', *, *, #4389, .F. ) ;
#9793 = ORIENTED_EDGE ( 'NONE', *, *, #17136, .F. ) ;
#9794 = CARTESIAN_POINT ( 'NONE',  ( 66.70577848186255210, 57.91700714588437648, 3.999628797553630655 ) ) ;
#9795 = CARTESIAN_POINT ( 'NONE',  ( 3.279379792629018020, -34.01329952344053709, 7.695279973900954751 ) ) ;
#9796 = CARTESIAN_POINT ( 'NONE',  ( 84.55403409623259847, 2.802886334004389024, 2.719422554281196280 ) ) ;
#9797 = ORIENTED_EDGE ( 'NONE', *, *, #3898, .F. ) ;
#9798 = CARTESIAN_POINT ( 'NONE',  ( 24.49724481738078197, 2.968026975615160268, 3.636704260287059398 ) ) ;
#9799 = EDGE_CURVE ( 'NONE', #33660, #30400, #30282, .T. ) ;
#9800 = DIRECTION ( 'NONE',  ( 0.000000000000000000, 0.000000000000000000, 1.000000000000000000 ) ) ;
#9801 = CARTESIAN_POINT ( 'NONE',  ( 25.01091298175105848, 3.329590532566609529, -1.936828115965013142 ) ) ;
#9802 = CARTESIAN_POINT ( 'NONE',  ( 1.169096226813607586, -26.12294996860957852, 7.782861076432730840 ) ) ;
#9803 = ORIENTED_EDGE ( 'NONE', *, *, #33017, .F. ) ;
#9804 = DIRECTION ( 'NONE',  ( -0.000000000000000000, -0.000000000000000000, 1.000000000000000000 ) ) ;
#9805 = UNCERTAINTY_MEASURE_WITH_UNIT (LENGTH_MEASURE( 1.000000000000000082E-05 ), #32556, 'distance_accuracy_value', 'NONE');
#9806 = VERTEX_POINT ( 'NONE', #11787 ) ;
#9807 = CARTESIAN_POINT ( 'NONE',  ( -70.92837670882107659, -45.61702805680359063, 10.00000000000000888 ) ) ;
#9808 = VERTEX_POINT ( 'NONE', #8710 ) ;
#9809 = CARTESIAN_POINT ( 'NONE',  ( 79.35276748299774852, 64.76637986602874264, -3.438247877890630910 ) ) ;
#9810 = LINE ( 'NONE', #40688, #18755 ) ;
#9811 = CARTESIAN_POINT ( 'NONE',  ( 79.14833415808527661, 65.26800409942002545, 3.041370705153016996 ) ) ;
#9813 = ORIENTED_EDGE ( 'NONE', *, *, #10460, .T. ) ;
#9812 = LINE ( 'NONE', #19690, #38771 ) ;
#9814 = ADVANCED_FACE ( 'NONE', ( #33861 ), #18183, .F. ) ;
#9815 = CARTESIAN_POINT ( 'NONE',  ( -0.04750094642060438688, -26.54137113793980873, 7.767720160662274331 ) ) ;
#9816 = CIRCLE ( 'NONE', #13757, 0.1000000000000028644 ) ;
#9817 = CARTESIAN_POINT ( 'NONE',  ( -0.5293678058294215560, -32.26774198379361280, 7.737115613922535218 ) ) ;
#9818 = DIRECTION ( 'NONE',  ( -0.000000000000000000, 1.000000000000000000, -0.000000000000000000 ) ) ;
#9819 = CARTESIAN_POINT ( 'NONE',  ( 21.85643539959776760, 8.744094842958308078, -10.51782716378651550 ) ) ;
#9820 = CARTESIAN_POINT ( 'NONE',  ( 24.71484882724550758, 3.003952457561420708, -3.426556331288557189 ) ) ;
#9821 = ORIENTED_EDGE ( 'NONE', *, *, #19143, .F. ) ;
#9822 = CARTESIAN_POINT ( 'NONE',  ( -2.697268050091675118E-17, 3.729367930467589076, 6.000000000000000000 ) ) ;
#9823 = ORIENTED_EDGE ( 'NONE', *, *, #16324, .T. ) ;
#9824 = CARTESIAN_POINT ( 'NONE',  ( -40.24874870218063450, -25.49307895267003587, 6.700000000000000178 ) ) ;
#9825 = CARTESIAN_POINT ( 'NONE',  ( 4.288407054171600841, -27.36489447023938126, 7.652160403243383868 ) ) ;
#9826 = CARTESIAN_POINT ( 'NONE',  ( -80.34590231409514161, -5.681217598735836205, -3.387305046538306552 ) ) ;
#9827 = EDGE_CURVE ( 'NONE', #5466, #22987, #5152, .T. ) ;
#9828 = CARTESIAN_POINT ( 'NONE',  ( 0.1003003074055170557, -25.13424064674780922, 7.635761828346577573 ) ) ;
#9829 = CARTESIAN_POINT ( 'NONE',  ( 3.300000000000000711, 0.000000000000000000, 0.000000000000000000 ) ) ;
#9830 = CARTESIAN_POINT ( 'NONE',  ( 80.40747942978342166, 64.69963996956802532, 3.448515284080270860 ) ) ;
#9831 = FACE_BOUND ( 'NONE', #16930, .T. ) ;
#9832 = CARTESIAN_POINT ( 'NONE',  ( -0.5692424881582137663, -26.90557721422857895, 7.737115613922536106 ) ) ;
#9833 = ORIENTED_EDGE ( 'NONE', *, *, #11414, .T. ) ;
#9834 = CARTESIAN_POINT ( 'NONE',  ( -1.580908707445344064, -30.78775612134597139, 7.743886751744248897 ) ) ;
#9835 = CARTESIAN_POINT ( 'NONE',  ( 20.26402972545001191, -7.228810192355688002, -2.500000000000000000 ) ) ;
#9836 = VECTOR ( 'NONE', #25586, 1000.000000000000000 ) ;
#9837 = B_SPLINE_CURVE_WITH_KNOTS ( 'NONE', 3,
 ( #4465, #32269, #16783, #38412, #10210, #26283, #22792, #38817, #35361, #10609, #7133, #19693, #13909, #26079, #1379, #1181, #32665, #21114, #30590, #1773, #14922, #40040, #5463, #30166, #21317, #36547, #33891 ),
 .UNSPECIFIED., .F., .F.,
 ( 4, 1, 2, 2, 1, 1, 1, 1, 1, 2, 2, 1, 1, 1, 1, 2, 2, 1, 4 ),
 ( 0.000000000000000000, 0.2324235260548973003, 0.2469499964333282671, 0.2614764668117592894, 0.2905294075686204458, 0.3486352890823428141, 0.4648470521097886055, 0.4938999928666482075, 0.4975316104612538815, 0.4993474192585585780, 0.5011632280558633301, 0.5084264632450831156, 0.5229529336235230197, 0.5810588151372841903, 0.6972705781648077528, 0.7263235189216886711, 0.7553764596785694785, 0.8134823411923304270, 0.9296941042198524352 ),
 .UNSPECIFIED. ) ;
#9838 = CARTESIAN_POINT ( 'NONE',  ( -65.15514661499977933, 34.97220226750606997, 6.888442104241538466 ) ) ;
#9839 = FACE_OUTER_BOUND ( 'NONE', #31241, .T. ) ;
#9840 = CARTESIAN_POINT ( 'NONE',  ( 4.626733377823518012, -27.83888570657239470, 7.695279973900954751 ) ) ;
#9841 = DIRECTION ( 'NONE',  ( 0.000000000000000000, 0.000000000000000000, 1.000000000000000000 ) ) ;
#9842 = CARTESIAN_POINT ( 'NONE',  ( 30.51504204651931929, -0.1407231940035871265, 4.969008339076835590 ) ) ;
#9843 = EDGE_CURVE ( 'NONE', #12335, #6115, #3795, .T. ) ;
#9844 = CARTESIAN_POINT ( 'NONE',  ( 87.61456772748933020, -0.05511631305283664489, -4.124113870075747812 ) ) ;
#9845 = CONICAL_SURFACE ( 'NONE', #21667, 6.406751979251626317, 0.7853981633974482790 ) ;
#9846 = ORIENTED_EDGE ( 'NONE', *, *, #36271, .F. ) ;
#9848 = CARTESIAN_POINT ( 'NONE',  ( -27.07867591359219972, -26.64985754041175525, 6.800000000000000711 ) ) ;
#9847 = CARTESIAN_POINT ( 'NONE',  ( 78.88492378528530935, 66.04028779424463380, -1.804401104814771895 ) ) ;
#9849 = CARTESIAN_POINT ( 'NONE',  ( -70.44490529243154242, -45.69367636896786422, 9.988720588804540057 ) ) ;
#9850 = CARTESIAN_POINT ( 'NONE',  ( -2.878675913592191993, -26.64985754041175525, 6.700000000000000178 ) ) ;
#9851 = ORIENTED_EDGE ( 'NONE', *, *, #26830, .F. ) ;
#9852 = CARTESIAN_POINT ( 'NONE',  ( -1.635022261790646469, -28.91028966882242557, 7.784476445165073422 ) ) ;
#9853 = ORIENTED_EDGE ( 'NONE', *, *, #40675, .F. ) ;
#9854 = CARTESIAN_POINT ( 'NONE',  ( -74.62920569612701627, -4.460155050320008918, 9.295740457114378685 ) ) ;
#9856 = ORIENTED_EDGE ( 'NONE', *, *, #29979, .T. ) ;
#9855 = ORIENTED_EDGE ( 'NONE', *, *, #30502, .T. ) ;
#9857 = CARTESIAN_POINT ( 'NONE',  ( 80.78100857081943786, 62.68361397997274054, -3.372125408468112262 ) ) ;
#9858 = EDGE_CURVE ( 'NONE', #21608, #6003, #29636, .T. ) ;
#9859 = CARTESIAN_POINT ( 'NONE',  ( 5.152950880260274147, -30.14423324962431749, 7.714178352335856026 ) ) ;
#9860 = EDGE_CURVE ( 'NONE', #38473, #6204, #19882, .T. ) ;
#9861 = CARTESIAN_POINT ( 'NONE',  ( 23.51444095708766824, 1.310649503969850915, 5.121933516958420363 ) ) ;
#9863 = VERTEX_POINT ( 'NONE', #25398 ) ;
#9862 = ORIENTED_EDGE ( 'NONE', *, *, #13667, .F. ) ;
#9864 = EDGE_CURVE ( 'NONE', #13694, #2784, #21903, .T. ) ;
#9865 = CARTESIAN_POINT ( 'NONE',  ( 81.39510468133835275, 61.43011602722283016, -1.270639542487658424 ) ) ;
#9866 = CIRCLE ( 'NONE', #36804, 0.1000000000000028644 ) ;
#9867 = CARTESIAN_POINT ( 'NONE',  ( 4.744454306064458393, -28.05544235445824697, 6.949473656533215582 ) ) ;
#9869 = CYLINDRICAL_SURFACE ( 'NONE', #32843, 2.500000000000002220 ) ;
#9868 = CARTESIAN_POINT ( 'NONE',  ( -58.98347169605253981, 28.20694469989773623, -6.383988387381219987 ) ) ;
#9870 = DIRECTION ( 'NONE',  ( 0.9267318687906771491, -0.3757233601570964532, 0.000000000000000000 ) ) ;
#9871 = CARTESIAN_POINT ( 'NONE',  ( 72.57946960881442067, 58.78899945845352448, 3.647993048395011151 ) ) ;
#9872 = CARTESIAN_POINT ( 'NONE',  ( 23.42095263414284290, 3.374540284680194624, -3.661182053110778600 ) ) ;
#9873 = ORIENTED_EDGE ( 'NONE', *, *, #9110, .T. ) ;
#9874 = CARTESIAN_POINT ( 'NONE',  ( -36.44874870218064444, -26.64985754041175525, 6.800000000000000711 ) ) ;
#9875 = ORIENTED_EDGE ( 'NONE', *, *, #35862, .F. ) ;
#9876 = CARTESIAN_POINT ( 'NONE',  ( 21.85643539959776760, 7.145415623174192987, -7.905327125498018859 ) ) ;
#9877 = AXIS2_PLACEMENT_3D ( 'NONE', #21742, #18629, #5270 ) ;
#9878 = DIRECTION ( 'NONE',  ( -0.000000000000000000, -0.000000000000000000, -1.000000000000000000 ) ) ;
#9879 = CARTESIAN_POINT ( 'NONE',  ( 86.00054146471580907, 0.2529338399765344580, 5.999804812770356932 ) ) ;
#9880 = CARTESIAN_POINT ( 'NONE',  ( 80.97210443043506700, 64.61276409569624946, 3.292658836682931245 ) ) ;
#9881 = CARTESIAN_POINT ( 'NONE',  ( 87.43313723349395161, -0.009410480739497543642, 5.495402557179364322 ) ) ;
#9882 = ORIENTED_EDGE ( 'NONE', *, *, #3669, .F. ) ;
#9883 = CARTESIAN_POINT ( 'NONE',  ( 0.4449537687655561458, -32.72967155099453151, 7.774064877406529739 ) ) ;
#9884 = CARTESIAN_POINT ( 'NONE',  ( 14.82998033694128459, -4.532293462924823935, 2.514727759383232897 ) ) ;
#9885 = CARTESIAN_POINT ( 'NONE',  ( 36.42070800990175172, -3.114118155843566438, -5.890730341733725339 ) ) ;
#9886 = CYLINDRICAL_SURFACE ( 'NONE', #37793, 0.09010775117052900740 ) ;
#9887 = FACE_OUTER_BOUND ( 'NONE', #33067, .T. ) ;
#9888 = CARTESIAN_POINT ( 'NONE',  ( 30.57577539112692477, -3.618309187433789376, -4.738484246135796774 ) ) ;
#9889 = ORIENTED_EDGE ( 'NONE', *, *, #26551, .F. ) ;
#9890 = CIRCLE ( 'NONE', #28944, 3.977260115179314770 ) ;
#9891 = DIRECTION ( 'NONE',  ( 0.000000000000000000, 0.000000000000000000, 1.000000000000000000 ) ) ;
#9892 = CARTESIAN_POINT ( 'NONE',  ( 28.18787290715265215, -3.182640706483542470, 4.605797312080136763 ) ) ;
#9893 = ORIENTED_EDGE ( 'NONE', *, *, #27699, .F. ) ;
#9894 = EDGE_LOOP ( 'NONE', ( #20988, #34417, #19653, #37205 ) ) ;
#9895 = CARTESIAN_POINT ( 'NONE',  ( 20.91846109042669610, 4.580160148488255700, 2.658159626579862156 ) ) ;
#9896 = CARTESIAN_POINT ( 'NONE',  ( -2.697268050091675118E-17, 3.729367930467589076, 6.000000000000000000 ) ) ;
#9897 = CARTESIAN_POINT ( 'NONE',  ( 66.43385761674679202, 57.75742247880091185, -4.000000000000006217 ) ) ;
#9898 = EDGE_CURVE ( 'NONE', #28243, #33383, #37935, .T. ) ;
#9899 = ORIENTED_EDGE ( 'NONE', *, *, #22254, .T. ) ;
#9900 = ADVANCED_FACE ( 'NONE', ( #19217 ), #35683, .T. ) ;
#9901 = CIRCLE ( 'NONE', #20408, 0.1000000000000028644 ) ;
#9902 = PLANE ( 'NONE',  #39710 ) ;
#9903 = DIRECTION ( 'NONE',  ( -1.000000000000000000, 0.000000000000000000, 0.000000000000000000 ) ) ;
#9904 = EDGE_LOOP ( 'NONE', ( #23926, #11041, #29009, #8401 ) ) ;
#9905 = FACE_BOUND ( 'NONE', #8013, .T. ) ;
#9906 = CARTESIAN_POINT ( 'NONE',  ( 3.808759754361716876, -32.36363944866005227, 6.998987538705436329 ) ) ;
#9907 = ORIENTED_EDGE ( 'NONE', *, *, #16907, .T. ) ;
#9908 = CARTESIAN_POINT ( 'NONE',  ( 21.86792300497991803, 5.743675277279487901, 3.228481761958482021 ) ) ;
#9909 = ADVANCED_FACE ( 'NONE', ( #23515 ), #26601, .F. ) ;
#9910 = CARTESIAN_POINT ( 'NONE',  ( 82.50386574309229104, 63.87755912629609867, -1.586031901070164674 ) ) ;
#9911 = CARTESIAN_POINT ( 'NONE',  ( 81.10500554505499338, 61.42844135377578141, 1.938154327158146062 ) ) ;
#9912 = CARTESIAN_POINT ( 'NONE',  ( 2.910418097296712414, -26.39252032545340398, 7.785868773668302545 ) ) ;
#9913 = ORIENTED_EDGE ( 'NONE', *, *, #26041, .F. ) ;
#9914 = CARTESIAN_POINT ( 'NONE',  ( 75.20156067606269801, 62.14723293136128746, -3.810661578667819516 ) ) ;
#9916 = DIRECTION ( 'NONE',  ( 0.000000000000000000, 0.000000000000000000, 1.000000000000000000 ) ) ;
#9915 = CARTESIAN_POINT ( 'NONE',  ( 28.61591789821288145, 47.14532032487838364, 4.000000000000000000 ) ) ;
#9917 = CARTESIAN_POINT ( 'NONE',  ( 17.01838609035475613, 9.182891198947618960, -2.862528759259550970 ) ) ;
#9918 = CARTESIAN_POINT ( 'NONE',  ( 78.95529765307294667, 66.08830754916624528, -1.741375869723587710 ) ) ;
#9919 = CARTESIAN_POINT ( 'NONE',  ( 76.23342353645796265, 61.41352271612323932, 3.867068906741275569 ) ) ;
#9920 = VERTEX_POINT ( 'NONE', #14430 ) ;
#9921 = AXIS2_PLACEMENT_3D ( 'NONE', #24520, #14625, #21233 ) ;
#9922 = FACE_OUTER_BOUND ( 'NONE', #38031, .T. ) ;
#9923 = CARTESIAN_POINT ( 'NONE',  ( -58.55427315445740533, 30.31497649546018991, 5.142179345755665487 ) ) ;
#9924 = CARTESIAN_POINT ( 'NONE',  ( 82.02451737050283498, 62.15044802891524967, 1.700667878122440468 ) ) ;
#9926 = CARTESIAN_POINT ( 'NONE',  ( 15.78341758396470418, 8.012724437683271361, 3.484800230006450228 ) ) ;
#9925 = CARTESIAN_POINT ( 'NONE',  ( -0.09718281214228366438, -32.57305050230510091, 6.875671892026060661 ) ) ;
#9927 = CARTESIAN_POINT ( 'NONE',  ( 29.24730582455742578, -0.4004845594861357605, -5.905559009470326970 ) ) ;
#9928 = CARTESIAN_POINT ( 'NONE',  ( -1.699420810764287859, -29.60578847477102116, 7.691066658568944447 ) ) ;
#9929 = CARTESIAN_POINT ( 'NONE',  ( 3.573870332252533810, -26.73266402712449619, 6.920489980334476599 ) ) ;
#9930 = CARTESIAN_POINT ( 'NONE',  ( 4.682439246746215922, -31.37861164225721211, 7.782861076432729064 ) ) ;
#9931 = ORIENTED_EDGE ( 'NONE', *, *, #10183, .F. ) ;
#9932 = DIRECTION ( 'NONE',  ( 0.000000000000000000, 0.000000000000000000, 1.000000000000000000 ) ) ;
#9933 = CARTESIAN_POINT ( 'NONE',  ( 67.59777080239751967, 57.90654639195260245, 3.983714026670993835 ) ) ;
#9934 = CARTESIAN_POINT ( 'NONE',  ( 35.34375719191214671, -3.571401254346052045, -5.666764866774185450 ) ) ;
#9935 = CARTESIAN_POINT ( 'NONE',  ( 5.128444259610362543, -30.27593629695848421, 6.864216812847430127 ) ) ;
#9936 = CARTESIAN_POINT ( 'NONE',  ( 1.734605777361225565, -33.06976452674143019, 7.674970859709602244 ) ) ;
#9937 = CARTESIAN_POINT ( 'NONE',  ( 1.736314072191997848, -32.96974039457447248, 7.692469944509197077 ) ) ;
#9938 = CARTESIAN_POINT ( 'NONE',  ( 21.88224095673515635, -13.29272450212527446, -2.499999999999999556 ) ) ;
#9939 = CARTESIAN_POINT ( 'NONE',  ( 22.00316676826400908, -11.76202948577872753, 2.500000000000000000 ) ) ;
#9940 = LINE ( 'NONE', #3405, #5186 ) ;
#9941 = ORIENTED_EDGE ( 'NONE', *, *, #16965, .T. ) ;
#9942 = B_SPLINE_CURVE_WITH_KNOTS ( 'NONE', 3,
 ( #10870, #38470, #14167, #32524, #22655, #23054, #32726, #36011, #4711, #32136 ),
 .UNSPECIFIED., .F., .F.,
 ( 4, 3, 3, 4 ),
 ( 0.0005050348086185310918, 0.0005143352185143295566, 0.0005445898203825194584, 0.0005634294782181710655 ),
 .UNSPECIFIED. ) ;
#9943 = ORIENTED_EDGE ( 'NONE', *, *, #35263, .T. ) ;
#9944 = CARTESIAN_POINT ( 'NONE',  ( -11.81496944966682960, -21.25669541281728669, -4.000000000000000000 ) ) ;
#9945 = CARTESIAN_POINT ( 'NONE',  ( 68.43818535210665743, 59.05932329210152432, -3.950303728398549374 ) ) ;
#9946 = AXIS2_PLACEMENT_3D ( 'NONE', #13375, #1448, #23068 ) ;
#9947 = ORIENTED_EDGE ( 'NONE', *, *, #14815, .F. ) ;
#9948 = DIRECTION ( 'NONE',  ( 0.000000000000000000, 1.000000000000000000, 0.000000000000000000 ) ) ;
#9949 = CARTESIAN_POINT ( 'NONE',  ( 30.67349724481533002, -3.593355625737403525, 4.777428303402127874 ) ) ;
#9950 = CARTESIAN_POINT ( 'NONE',  ( 24.00583079004835341, 2.820796528902969502, 3.912411818918270168 ) ) ;
#9951 = CARTESIAN_POINT ( 'NONE',  ( 8.290806648384990041, -35.94265729135299381, 6.000000000000000000 ) ) ;
#9953 = EDGE_CURVE ( 'NONE', #15453, #7222, #26989, .T. ) ;
#9952 = CARTESIAN_POINT ( 'NONE',  ( -56.59682361629209879, 30.63869417066593925, 3.015094993620162978 ) ) ;
#9954 = VERTEX_POINT ( 'NONE', #1106 ) ;
#9955 = CARTESIAN_POINT ( 'NONE',  ( 21.83036068403676921, 5.963027752284762784, 3.135844384568250653 ) ) ;
#9956 = ADVANCED_FACE ( 'NONE', ( #29884 ), #29291, .F. ) ;
#9957 = DIRECTION ( 'NONE',  ( 0.000000000000000000, 8.881784197001253901E-15, 1.000000000000000000 ) ) ;
#9958 = CARTESIAN_POINT ( 'NONE',  ( 81.23333979799274118, 62.00977392264719157, 2.676159939830916379 ) ) ;
#9959 = AXIS2_PLACEMENT_3D ( 'NONE', #4163, #29065, #872 ) ;
#9960 = ADVANCED_FACE ( 'NONE', ( #13638 ), #32988, .F. ) ;
#9961 = CARTESIAN_POINT ( 'NONE',  ( 0.6790956408842164782, -32.92475242180294259, 7.139344958878409919 ) ) ;
#9962 = ORIENTED_EDGE ( 'NONE', *, *, #20675, .F. ) ;
#9963 = CARTESIAN_POINT ( 'NONE',  ( 78.90238306073098329, 63.15141027621823611, -3.791687334209852267 ) ) ;
#9965 = CARTESIAN_POINT ( 'NONE',  ( -0.4487487021806388365, -26.64985754041175525, 6.700000000000000178 ) ) ;
#9964 = CARTESIAN_POINT ( 'NONE',  ( 22.04975653352279963, 0.2919591322827700397, 7.506304445313716656 ) ) ;
#9966 = CARTESIAN_POINT ( 'NONE',  ( 80.19843342643493145, 65.64991096650632585, -2.811330881955115490 ) ) ;
#9967 = CARTESIAN_POINT ( 'NONE',  ( 80.57587054825803818, 61.08954103313657669, 1.748505333477117896 ) ) ;
#9968 = CARTESIAN_POINT ( 'NONE',  ( 33.45716606812183613, -3.829385970599605393, -5.093809925484540813 ) ) ;
#9969 = FACE_OUTER_BOUND ( 'NONE', #8588, .T. ) ;
#9970 =( BOUNDED_CURVE ( )  B_SPLINE_CURVE ( 3, ( #17377, #1772, #17582, #30164 ),
 .UNSPECIFIED., .F., .T. ) 
 B_SPLINE_CURVE_WITH_KNOTS ( ( 4, 4 ),
 ( 4.748221474220559735, 4.941946782021394036 ),
 .UNSPECIFIED. ) 
 CURVE ( )  GEOMETRIC_REPRESENTATION_ITEM ( )  RATIONAL_B_SPLINE_CURVE ( ( 1.000000000000000000, 0.9968749865767494445, 0.9968749865767494445, 1.000000000000000000 ) ) 
 REPRESENTATION_ITEM ( '' )  );
#9971 = CARTESIAN_POINT ( 'NONE',  ( -63.37463611956035692, 42.57616119279575173, 3.693273243659103588 ) ) ;
#9972 = CARTESIAN_POINT ( 'NONE',  ( 24.13449073166137637, 1.731319574254092997, -6.231442870084249464 ) ) ;
#9973 = DIRECTION ( 'NONE',  ( 0.000000000000000000, 0.000000000000000000, 1.000000000000000000 ) ) ;
#9974 = VERTEX_POINT ( 'NONE', #32793 ) ;
#9975 = CARTESIAN_POINT ( 'NONE',  ( -75.33383759686411452, -3.421339376598665716, 9.017346126309083942 ) ) ;
#9976 = CARTESIAN_POINT ( 'NONE',  ( 3.551251297819357777, -25.49307895267003587, 6.700000000000000178 ) ) ;
#9977 = ORIENTED_EDGE ( 'NONE', *, *, #2580, .T. ) ;
#9978 = CARTESIAN_POINT ( 'NONE',  ( -0.1489007850597646454, -32.54049873642831159, 7.761113333117550361 ) ) ;
#9979 = LINE ( 'NONE', #35922, #6559 ) ;
#9980 = CARTESIAN_POINT ( 'NONE',  ( 32.02031732332363845, -3.752465789452563261, -4.808771302114207558 ) ) ;
#9981 = CARTESIAN_POINT ( 'NONE',  ( 36.71895965078132917, -3.458220008152968372, -5.860798406330455457 ) ) ;
#9982 = CARTESIAN_POINT ( 'NONE',  ( 3.846394003886068891, -32.20710163246565116, 6.892063359921928090 ) ) ;
#9983 = CARTESIAN_POINT ( 'NONE',  ( 17.44269447096448644, 8.925452895480308513, 2.905853932266882378 ) ) ;
#9984 = CARTESIAN_POINT ( 'NONE',  ( 5.196109512279864617, -29.74298762467820367, 7.009310105710483185 ) ) ;
#9985 = CARTESIAN_POINT ( 'NONE',  ( -0.8989622146313063222, -27.22613634409080419, 7.751599049952198506 ) ) ;
#9986 = DIRECTION ( 'NONE',  ( 0.000000000000000000, 0.000000000000000000, 1.000000000000000000 ) ) ;
#9987 = DIRECTION ( 'NONE',  ( -0.000000000000000000, -0.000000000000000000, 1.000000000000000000 ) ) ;
#9988 = CARTESIAN_POINT ( 'NONE',  ( 25.21793605145752792, 1.560386695300661319, -4.376291279302483517 ) ) ;
#9989 = CIRCLE ( 'NONE', #33006, 0.1000000000000028644 ) ;
#9990 = CARTESIAN_POINT ( 'NONE',  ( 29.65754893815654825, 1.153748204478383999, -4.260714825772614844 ) ) ;
#9991 = CARTESIAN_POINT ( 'NONE',  ( 15.70794464876099816, 12.77956130087500952, -2.500000000000005329 ) ) ;
#9992 = ORIENTED_EDGE ( 'NONE', *, *, #29445, .T. ) ;
#9993 = CARTESIAN_POINT ( 'NONE',  ( 66.54830849220104483, 57.89461212714910943, 3.999444518117950764 ) ) ;
#9994 = DIRECTION ( 'NONE',  ( -0.8660254037844232755, 0.5000000000000265343, 0.000000000000000000 ) ) ;
#9995 = CARTESIAN_POINT ( 'NONE',  ( 84.91553621511910421, 2.364970790127210787, 4.120477167815592701 ) ) ;
#9996 = ORIENTED_EDGE ( 'NONE', *, *, #15587, .F. ) ;
#9997 = CARTESIAN_POINT ( 'NONE',  ( 26.60586539650099169, 1.632482450356405268, 4.331819419614522104 ) ) ;
#9998 = PLANE ( 'NONE',  #13980 ) ;
#9999 = CARTESIAN_POINT ( 'NONE',  ( 1.201481589801058014, -26.10828805710466582, 7.766640943994345569 ) ) ;
#10000 = ORIENTED_EDGE ( 'NONE', *, *, #35456, .T. ) ;
#10001 = LINE ( 'NONE', #31440, #13654 ) ;
#10002 = EDGE_CURVE ( 'NONE', #9233, #19674, #4771, .T. ) ;
#10003 = ORIENTED_EDGE ( 'NONE', *, *, #21855, .F. ) ;
#10004 = CARTESIAN_POINT ( 'NONE',  ( 79.82585920881969344, 63.98597419336228853, -3.710743084827439198 ) ) ;
#10005 = CARTESIAN_POINT ( 'NONE',  ( -0.08065709997538077214, -26.55697965350343281, 7.695279973900954751 ) ) ;
#10006 = CARTESIAN_POINT ( 'NONE',  ( 80.98019550867157079, 61.28820853408525693, 1.743126864185295055 ) ) ;
#10008 = VERTEX_POINT ( 'NONE', #4583 ) ;
#10007 = CARTESIAN_POINT ( 'NONE',  ( -9.741734729663692249, 54.65020406074287251, -1.000000000000000000 ) ) ;
#10009 = DIRECTION ( 'NONE',  ( -0.000000000000000000, -0.000000000000000000, 1.000000000000000000 ) ) ;
#10010 = CARTESIAN_POINT ( 'NONE',  ( 28.37767182338955507, -4.101067068145935579, 4.014301156824140016 ) ) ;
#10011 = DIRECTION ( 'NONE',  ( 0.000000000000000000, 0.000000000000000000, -1.000000000000000000 ) ) ;
#10012 = CARTESIAN_POINT ( 'NONE',  ( 21.85643539959777826, -13.51165962708896728, -8.254727072381385256 ) ) ;
#10013 = CARTESIAN_POINT ( 'NONE',  ( 23.73324195583390761, 3.546141233244914925, -3.227706410081386146 ) ) ;
#10014 = ORIENTED_EDGE ( 'NONE', *, *, #38061, .F. ) ;
#10015 = CARTESIAN_POINT ( 'NONE',  ( -64.95171866297674512, 36.28765213650433452, -6.629387290673639299 ) ) ;
#10016 = AXIS2_PLACEMENT_3D ( 'NONE', #8247, #20607, #27203 ) ;
#10017 = VERTEX_POINT ( 'NONE', #38537 ) ;
#10018 = CARTESIAN_POINT ( 'NONE',  ( -1.033762044237207522, -31.59092488823622702, 6.939395833800444002 ) ) ;
#10019 = CARTESIAN_POINT ( 'NONE',  ( -1.489921458977837565, -30.74547780039133116, 7.635761828346577573 ) ) ;
#10020 = CARTESIAN_POINT ( 'NONE',  ( -73.51024996325405425, -0.7972945005789436879, -9.719117299233273499 ) ) ;
#10021 = CARTESIAN_POINT ( 'NONE',  ( 1.700390093233090871, -29.56993018339339940, 7.750000000000000888 ) ) ;
#10022 = DIRECTION ( 'NONE',  ( 1.000000000000000000, 0.000000000000000000, 0.000000000000000000 ) ) ;
#10023 = CARTESIAN_POINT ( 'NONE',  ( 80.31657930512768928, 64.64970693426512582, 3.487490852634252292 ) ) ;
#10024 = CARTESIAN_POINT ( 'NONE',  ( 86.09116122586011954, 0.08319669091220074919, -6.006182420748226392 ) ) ;
#10025 = CARTESIAN_POINT ( 'NONE',  ( -0.5767534791761352864, -26.91199542853306070, 7.698786668945016842 ) ) ;
#10026 = CARTESIAN_POINT ( 'NONE',  ( -1.336825994161656928, -27.83057829189845478, 7.756742906098587298 ) ) ;
#10027 = CARTESIAN_POINT ( 'NONE',  ( 86.43572624768425783, -0.5192074800720990480, -5.777013305174518720 ) ) ;
#10028 = CARTESIAN_POINT ( 'NONE',  ( 33.62470413278058601, -1.226591137072588600, 5.454346315099659392 ) ) ;
#10029 = EDGE_CURVE ( 'NONE', #23121, #37478, #23312, .T. ) ;
#10030 = DIRECTION ( 'NONE',  ( 1.047444401652940007E-14, -1.000000000000000000, -0.000000000000000000 ) ) ;
#10031 = CARTESIAN_POINT ( 'NONE',  ( -0.3385372945680173995, -26.84912605459717838, 7.013842709614101167 ) ) ;
#10032 = CARTESIAN_POINT ( 'NONE',  ( 4.659898462552006571, -27.89621867541739775, 7.782167645815905921 ) ) ;
#10033 = CARTESIAN_POINT ( 'NONE',  ( -0.9969019986233668140, -27.33953798572080274, 7.651421919295150254 ) ) ;
#10034 = B_SPLINE_CURVE_WITH_KNOTS ( 'NONE', 3,
 ( #19891, #10422, #27229, #8077, #36701, #29168, #23189, #11564, #29366, #32464, #21066, #14658, #36305, #23931, #13721, #24140, #38821, #5620, #5415, #20640, #8484, #35563, #976, #24346, #26287 ),
 .UNSPECIFIED., .F., .F.,
 ( 4, 3, 3, 3, 3, 3, 3, 3, 4 ),
 ( 6.468151674592953384E-05, 9.076621574722270420E-05, 0.0001210204262067992404, 0.0001512763324577443512, 0.0001815301820994240324, 0.0002117781465860730096, 0.0002420274594459778639, 0.0002722905548971166559, 0.0002816827545175487591 ),
 .UNSPECIFIED. ) ;
#10035 = ORIENTED_EDGE ( 'NONE', *, *, #28665, .T. ) ;
#10036 = CARTESIAN_POINT ( 'NONE',  ( 68.69556364554829031, 58.38064408996493171, 3.985059344218205180 ) ) ;
#10037 = CARTESIAN_POINT ( 'NONE',  ( 36.42090402691821538, -3.114971261605032904, 5.890760934929827997 ) ) ;
#10038 = VECTOR ( 'NONE', #39625, 1000.000000000000000 ) ;
#10039 = EDGE_CURVE ( 'NONE', #28543, #2729, #27664, .T. ) ;
#10040 = CARTESIAN_POINT ( 'NONE',  ( 71.66251436080506210, 60.98061884659114895, -3.745173303738185577 ) ) ;
#10041 = FACE_OUTER_BOUND ( 'NONE', #11554, .T. ) ;
#10042 = CARTESIAN_POINT ( 'NONE',  ( 86.68816865751659861, 0.9854590918928021193, 5.166709667929270999 ) ) ;
#10043 = VERTEX_POINT ( 'NONE', #17307 ) ;
#10045 = CARTESIAN_POINT ( 'NONE',  ( -0.4079795678955136506, -26.77622091812672878, 6.998987538705430111 ) ) ;
#10044 = CARTESIAN_POINT ( 'NONE',  ( 81.24801795318222730, 61.46771992710468169, -1.817988788077152584 ) ) ;
#10046 = CARTESIAN_POINT ( 'NONE',  ( 2.782197798051136317, -32.89830469346890141, 7.754798119455333705 ) ) ;
#10047 = VECTOR ( 'NONE', #32448, 1000.000000000000000 ) ;
#10048 = EDGE_LOOP ( 'NONE', ( #13065, #24431, #6724, #6013 ) ) ;
#10049 = FACE_OUTER_BOUND ( 'NONE', #34835, .T. ) ;
#10050 = ORIENTED_EDGE ( 'NONE', *, *, #35862, .T. ) ;
#10051 = CARTESIAN_POINT ( 'NONE',  ( -73.09553771626850960, -2.532785756717299108, 9.765145150773129501 ) ) ;
#10052 = ORIENTED_EDGE ( 'NONE', *, *, #16552, .F. ) ;
#10053 = EDGE_CURVE ( 'NONE', #28074, #11880, #5519, .T. ) ;
#10054 = CARTESIAN_POINT ( 'NONE',  ( 78.70126604931442671, 66.02149264047228883, -1.577285172236841726 ) ) ;
#10055 = CARTESIAN_POINT ( 'NONE',  ( -1.503235331079484149, -28.43115960637267747, 7.652160403243382980 ) ) ;
#10056 = CARTESIAN_POINT ( 'NONE',  ( 23.90473187725620363, 2.109340586275191942, 4.420426059884545289 ) ) ;
#10057 = ORIENTED_EDGE ( 'NONE', *, *, #16606, .F. ) ;
#10058 = LINE ( 'NONE', #6588, #6194 ) ;
#10060 = CARTESIAN_POINT ( 'NONE',  ( 3.977572546501454642, -32.22783162523180067, 7.695279973900954751 ) ) ;
#10059 = CARTESIAN_POINT ( 'NONE',  ( -58.88504699088242234, 28.60929463400939099, -6.101381014920331580 ) ) ;
#10061 = DIRECTION ( 'NONE',  ( 0.9594800004753906153, 0.2817767355331954326, 0.000000000000000000 ) ) ;
#10062 = CARTESIAN_POINT ( 'NONE',  ( 69.77571843317402056, 59.04509999696490041, 3.985452289341159915 ) ) ;
#10063 = ORIENTED_EDGE ( 'NONE', *, *, #40113, .T. ) ;
#10064 = CARTESIAN_POINT ( 'NONE',  ( 23.44360806831497257, 3.234883382834601750, -3.775111565067499342 ) ) ;
#10065 = ORIENTED_EDGE ( 'NONE', *, *, #23203, .F. ) ;
#10066 = ORIENTED_EDGE ( 'NONE', *, *, #2825, .F. ) ;
#10067 = EDGE_CURVE ( 'NONE', #30519, #32349, #34647, .T. ) ;
#10068 = CARTESIAN_POINT ( 'NONE',  ( 21.85643539959777826, -4.710037025930063237, 11.93878138912534226 ) ) ;
#10069 = CARTESIAN_POINT ( 'NONE',  ( 21.85970433026863802, 3.598116536247010444, 3.919871293596266515 ) ) ;
#10070 = ORIENTED_EDGE ( 'NONE', *, *, #17372, .F. ) ;
#10071 = DIRECTION ( 'NONE',  ( 0.000000000000000000, 0.000000000000000000, 1.000000000000000000 ) ) ;
#10072 = CARTESIAN_POINT ( 'NONE',  ( 79.50049935621065345, 66.06919348781509882, 2.170472567306921174 ) ) ;
#10073 = CARTESIAN_POINT ( 'NONE',  ( 87.79537149936930973, -0.4305974645707495441, -5.064761461465907999 ) ) ;
#10074 = ORIENTED_EDGE ( 'NONE', *, *, #3010, .F. ) ;
#10075 = AXIS2_PLACEMENT_3D ( 'NONE', #1833, #10859, #36195 ) ;
#10076 = CARTESIAN_POINT ( 'NONE',  ( 0.5650878065122802996, -32.77478541679437285, 7.730758795053806587 ) ) ;
#10077 = CARTESIAN_POINT ( 'NONE',  ( 28.89675923326203488, -2.947373090957444042, 4.716436167749639807 ) ) ;
#10078 = CARTESIAN_POINT ( 'NONE',  ( 35.95071194461377928, -2.121207001979848794, 5.817376088847740156 ) ) ;
#10079 = CARTESIAN_POINT ( 'NONE',  ( 5.076938436256279275, -29.17122450598600381, 7.006423389747788555 ) ) ;
#10080 = CARTESIAN_POINT ( 'NONE',  ( 35.33511053670775937, -3.171501256377859512, -5.721296600767692198 ) ) ;
#10081 = CARTESIAN_POINT ( 'NONE',  ( 0.5713440154618105726, -32.77699347534518637, 7.692469944509197965 ) ) ;
#10082 = CARTESIAN_POINT ( 'NONE',  ( 84.23367565633908782, 2.854638525470858834, 2.083157151739415180 ) ) ;
#10083 = EDGE_CURVE ( 'NONE', #25477, #22296, #4187, .T. ) ;
#10084 = EDGE_CURVE ( 'NONE', #13148, #273, #17110, .T. ) ;
#10085 = CARTESIAN_POINT ( 'NONE',  ( -72.84815947045233031, 2.429809908889422498, 10.96147798754374669 ) ) ;
#10086 = CARTESIAN_POINT ( 'NONE',  ( 1.230319205269136518, -26.20258206353872765, 7.754798119455333705 ) ) ;
#10087 = ADVANCED_FACE ( 'NONE', ( #10731 ), #11133, .T. ) ;
#10088 = DIRECTION ( 'NONE',  ( 0.7508067542896625923, 7.864283315039216110E-15, -0.6605219282605402364 ) ) ;
#10089 = AXIS2_PLACEMENT_3D ( 'NONE', #26451, #24159, #4822 ) ;
#10090 = AXIS2_PLACEMENT_3D ( 'NONE', #3219, #37954, #4015 ) ;
#10091 = CARTESIAN_POINT ( 'NONE',  ( 32.00410610819579915, -3.635846591686252793, 4.956023177179895711 ) ) ;
#10092 = ORIENTED_EDGE ( 'NONE', *, *, #6199, .T. ) ;
#10093 = EDGE_LOOP ( 'NONE', ( #7810, #26024, #8245, #38543, #25403 ) ) ;
#10094 = CARTESIAN_POINT ( 'NONE',  ( 27.81484381033608599, 1.842735594674395516, 3.911111060978480936 ) ) ;
#10095 = DIRECTION ( 'NONE',  ( 0.000000000000000000, 0.000000000000000000, 1.000000000000000000 ) ) ;
#10096 = CARTESIAN_POINT ( 'NONE',  ( 66.54439450091902586, 57.90558988169555477, -3.999229419688612008 ) ) ;
#10097 = ORIENTED_EDGE ( 'NONE', *, *, #30189, .F. ) ;
#10098 = EDGE_CURVE ( 'NONE', #34388, #14142, #30100, .T. ) ;
#10099 = VERTEX_POINT ( 'NONE', #27606 ) ;
#10100 = FACE_BOUND ( 'NONE', #39696, .T. ) ;
#10101 = ORIENTED_EDGE ( 'NONE', *, *, #40018, .F. ) ;
#10102 = CARTESIAN_POINT ( 'NONE',  ( 82.01097102582248510, 65.15803335478928204, -1.775718711110015224 ) ) ;
#10103 = CARTESIAN_POINT ( 'NONE',  ( 2.929197463401206125, -26.39973560994384982, 7.784476445165072533 ) ) ;
#10104 = ORIENTED_EDGE ( 'NONE', *, *, #31441, .F. ) ;
#10105 = ORIENTED_EDGE ( 'NONE', *, *, #31485, .T. ) ;
#10106 = CARTESIAN_POINT ( 'NONE',  ( 74.93610893867889899, 61.23939191379614755, -3.912919437578919357 ) ) ;
#10108 = DIRECTION ( 'NONE',  ( 0.000000000000000000, 0.000000000000000000, -1.000000000000000000 ) ) ;
#10107 = CARTESIAN_POINT ( 'NONE',  ( -74.03402466285142225, 19.33157623370700762, 9.800414904976365804 ) ) ;
#10109 = CARTESIAN_POINT ( 'NONE',  ( 16.29644454726526348, 9.829709983188696043, -2.749852321238235753 ) ) ;
#10110 = CARTESIAN_POINT ( 'NONE',  ( 76.54260510937180584, 60.74419326975372968, 3.642592851547784782 ) ) ;
#10111 = CARTESIAN_POINT ( 'NONE',  ( 4.383437233793472387, -27.48154155094239570, 6.863904403958575706 ) ) ;
#10112 = EDGE_CURVE ( 'NONE', #218, #28242, #6627, .T. ) ;
#10113 = LINE ( 'NONE', #3975, #448 ) ;
#10114 = VECTOR ( 'NONE', #36242, 1000.000000000000000 ) ;
#10115 = CARTESIAN_POINT ( 'NONE',  ( 79.78161832376108009, 66.22496747522392013, 1.859759604986721548 ) ) ;
#10116 = CARTESIAN_POINT ( 'NONE',  ( -0.9682691519857027362, -31.83449588853605405, 7.643192810543820492 ) ) ;
#10117 = CARTESIAN_POINT ( 'NONE',  ( 29.97903609306309747, -3.796949753938318128, 3.982659670407546759 ) ) ;
#10118 = CARTESIAN_POINT ( 'NONE',  ( 2.406143767593636795, -26.24398412221321308, 7.759451378593096749 ) ) ;
#10119 = CARTESIAN_POINT ( 'NONE',  ( 3.547885809248545019, -26.71567729002453362, 6.882085323592685100 ) ) ;
#10120 = EDGE_CURVE ( 'NONE', #32660, #19192, #31716, .T. ) ;
#10121 = AXIS2_PLACEMENT_3D ( 'NONE', #100, #15520, #40630 ) ;
#10122 = DIRECTION ( 'NONE',  ( 1.000000000000000000, -0.000000000000000000, 0.000000000000000000 ) ) ;
#10123 = CARTESIAN_POINT ( 'NONE',  ( 0.7304454269062439220, -26.31121765476125773, 6.988553391373222290 ) ) ;
#10124 = LINE ( 'NONE', #7047, #7189 ) ;
#10125 = EDGE_CURVE ( 'NONE', #2282, #8440, #37505, .T. ) ;
#10126 = CARTESIAN_POINT ( 'NONE',  ( 36.34374669389929835, -1.915861758104068224, -5.836669621121017393 ) ) ;
#10127 = VECTOR ( 'NONE', #29860, 1000.000000000000000 ) ;
#10128 = CARTESIAN_POINT ( 'NONE',  ( 5.727845070442864284, -26.50757187106134083, 6.894806418505347700 ) ) ;
#10129 = CARTESIAN_POINT ( 'NONE',  ( 4.370302737341240196, -27.30684236520528785, 7.750000000000000000 ) ) ;
#10130 = CARTESIAN_POINT ( 'NONE',  ( -2.673316637388258865, -27.10729750018004935, 7.695279973900954751 ) ) ;
#10131 = CARTESIAN_POINT ( 'NONE',  ( -76.12810195176366790, 8.940663570071636812, 9.995849007841474787 ) ) ;
#10132 = EDGE_CURVE ( 'NONE', #25920, #17641, #34020, .T. ) ;
#10133 = PLANE ( 'NONE',  #10330 ) ;
#10134 = CARTESIAN_POINT ( 'NONE',  ( -1.469804480216468701, -28.34112281322530791, 7.784476445165073422 ) ) ;
#10135 = ORIENTED_EDGE ( 'NONE', *, *, #12129, .F. ) ;
#10136 = CARTESIAN_POINT ( 'NONE',  ( -30.44874870218064089, -26.64985754041175525, 6.700000000000000178 ) ) ;
#10137 = CARTESIAN_POINT ( 'NONE',  ( 67.74957807481123950, 58.23899230517488235, -3.997461085607396214 ) ) ;
#10138 = CARTESIAN_POINT ( 'NONE',  ( 3.055515830036299008, -26.34291387766242920, 6.895394898881666457 ) ) ;
#10139 = VERTEX_POINT ( 'NONE', #39963 ) ;
#10140 = DIRECTION ( 'NONE',  ( -0.000000000000000000, -0.000000000000000000, 1.000000000000000000 ) ) ;
#10141 = DIRECTION ( 'NONE',  ( 0.06925283225918045515, 0.9903616414705930238, 0.1199494240409451351 ) ) ;
#10142 = CARTESIAN_POINT ( 'NONE',  ( 22.40981647624643713, 3.721157939412742532, 4.045705223971617137 ) ) ;
#10143 = CARTESIAN_POINT ( 'NONE',  ( 5.049964969917366986, -28.55486946145695271, 6.941203072598474577 ) ) ;
#10144 = CARTESIAN_POINT ( 'NONE',  ( 1.085683504084817175, -26.22595486797094466, 7.740055089680402567 ) ) ;
#10145 = CARTESIAN_POINT ( 'NONE',  ( 1.130000382093760747, -26.11671394750277742, 6.887161170156906209 ) ) ;
#10146 = ORIENTED_EDGE ( 'NONE', *, *, #12433, .T. ) ;
#10147 = CARTESIAN_POINT ( 'NONE',  ( 23.75168596251202402, 3.571076225440265262, 3.154308973096512148 ) ) ;
#10148 = CARTESIAN_POINT ( 'NONE',  ( 3.852146645688039328, -32.33035474113215457, 7.750000000000000888 ) ) ;
#10149 = VECTOR ( 'NONE', #30288, 1000.000000000000000 ) ;
#10150 = CARTESIAN_POINT ( 'NONE',  ( 20.51517429375766355, -3.043394856432828366, 3.333276972429214613 ) ) ;
#10151 = CARTESIAN_POINT ( 'NONE',  ( 80.45813098276143194, 63.95641783144333203, 3.614389211669657875 ) ) ;
#10152 = DIRECTION ( 'NONE',  ( 0.000000000000000000, 0.000000000000000000, -1.000000000000000000 ) ) ;
#10153 = ORIENTED_EDGE ( 'NONE', *, *, #20133, .F. ) ;
#10154 = CARTESIAN_POINT ( 'NONE',  ( 78.47217392918747692, 65.00024052541876074, -3.055712048904924316 ) ) ;
#10156 = CARTESIAN_POINT ( 'NONE',  ( -1.708840123953186962, -28.77800258176304737, 6.927178575251052628 ) ) ;
#10155 = CARTESIAN_POINT ( 'NONE',  ( 22.63505186344747244, 0.3020627423357405417, 6.468267501412062082 ) ) ;
#10157 = CARTESIAN_POINT ( 'NONE',  ( 81.75671479976286093, 62.52433184976155189, -2.563845612518023565 ) ) ;
#10158 = CARTESIAN_POINT ( 'NONE',  ( 78.58588809754505178, 64.79968573292298117, 3.228498513792966484 ) ) ;
#10159 = EDGE_CURVE ( 'NONE', #21319, #31581, #7935, .T. ) ;
#10160 = CARTESIAN_POINT ( 'NONE',  ( 8.290806648384990041, 0.000000000000000000, -6.000000000000000000 ) ) ;
#10161 = CARTESIAN_POINT ( 'NONE',  ( 82.43037228308448050, 64.59322875725442259, 1.165579324820864571 ) ) ;
#10162 = DIRECTION ( 'NONE',  ( -1.000000000000000000, 0.000000000000000000, 0.000000000000000000 ) ) ;
#10163 = CARTESIAN_POINT ( 'NONE',  ( 25.11223377877777807, -2.893972711065841086, 5.714375009671201155 ) ) ;
#10164 = CARTESIAN_POINT ( 'NONE',  ( 4.043747737267941567, -27.09675613275700101, 7.386948897581450346 ) ) ;
#10165 = ORIENTED_EDGE ( 'NONE', *, *, #12062, .T. ) ;
#10166 = CARTESIAN_POINT ( 'NONE',  ( -79.93950600478302704, -5.593546482839650835, 6.495256196073648347 ) ) ;
#10167 = CARTESIAN_POINT ( 'NONE',  ( 22.60277623034728478, 0.2789645760982217282, -6.515020334618169429 ) ) ;
#10168 = CARTESIAN_POINT ( 'NONE',  ( -0.05447690023199193432, -32.59178206026290781, 7.773839561854630098 ) ) ;
#10169 = VECTOR ( 'NONE', #15091, 1000.000000000000114 ) ;
#10170 = CIRCLE ( 'NONE', #15434, 0.1000000000000028644 ) ;
#10171 = CARTESIAN_POINT ( 'NONE',  ( -0.9974109439700435953, -31.77706419566279905, 7.785096263473211486 ) ) ;
#10172 = EDGE_CURVE ( 'NONE', #35733, #17688, #15011, .T. ) ;
#10173 = CARTESIAN_POINT ( 'NONE',  ( -58.92473026143643722, -52.43948302755219260, -2.500000000000000000 ) ) ;
#10174 = CARTESIAN_POINT ( 'NONE',  ( 33.68478720806815829, -3.838055986494960159, -5.140077084911478522 ) ) ;
#10175 = FACE_OUTER_BOUND ( 'NONE', #38403, .T. ) ;
#10176 = VECTOR ( 'NONE', #33033, 1000.000000000000000 ) ;
#10177 = CARTESIAN_POINT ( 'NONE',  ( 3.805292929746987074, -32.24004161184372919, 6.864651958020303368 ) ) ;
#10178 = CARTESIAN_POINT ( 'NONE',  ( 17.18926217949810109, 9.340092606904171646, 2.827706503231969037 ) ) ;
#10179 = CARTESIAN_POINT ( 'NONE',  ( 5.195942103142157542, -29.74646048981854207, 6.903112506833881667 ) ) ;
#10180 = CARTESIAN_POINT ( 'NONE',  ( -0.5720344077344724498, -26.90795824500195721, 7.660770905198787339 ) ) ;
#10181 = CARTESIAN_POINT ( 'NONE',  ( -8.878675913592189772, -24.55319635012989110, 6.800000000000000711 ) ) ;
#10182 = ADVANCED_FACE ( 'NONE', ( #2933 ), #27199, .F. ) ;
#10183 = EDGE_CURVE ( 'NONE', #21412, #5208, #8244, .T. ) ;
#10184 = AXIS2_PLACEMENT_3D ( 'NONE', #8203, #31641, #3461 ) ;
#10185 = DIRECTION ( 'NONE',  ( 0.000000000000000000, 0.000000000000000000, 1.000000000000000000 ) ) ;
#10186 = CARTESIAN_POINT ( 'NONE',  ( 22.50793842622461582, 0.7792813105832565590, -6.394562644212967939 ) ) ;
#10187 = CARTESIAN_POINT ( 'NONE',  ( 35.22275699169255603, -1.056573163075043453, -5.416485502172596611 ) ) ;
#10188 = EDGE_CURVE ( 'NONE', #9079, #744, #16468, .T. ) ;
#10189 = DIRECTION ( 'NONE',  ( -0.000000000000000000, -1.000000000000000000, -0.000000000000000000 ) ) ;
#10190 = ORIENTED_EDGE ( 'NONE', *, *, #29665, .F. ) ;
#10191 = VERTEX_POINT ( 'NONE', #37280 ) ;
#10192 = CARTESIAN_POINT ( 'NONE',  ( 66.56787846382142959, 57.83972306852010803, 3.999917672784798039 ) ) ;
#10193 = FACE_OUTER_BOUND ( 'NONE', #33775, .T. ) ;
#10194 = CARTESIAN_POINT ( 'NONE',  ( 88.33724419093491065, -2.316998127210522007, 1.237639510709749091 ) ) ;
#10195 = ORIENTED_EDGE ( 'NONE', *, *, #18727, .T. ) ;
#10196 = CARTESIAN_POINT ( 'NONE',  ( 2.864308709047130197, -26.26912818964179053, 7.710604733652628440 ) ) ;
#10197 = APPLICATION_PROTOCOL_DEFINITION ( 'draft international standard', 'automotive_design', 1998, #35030 ) ;
#10198 = FACE_OUTER_BOUND ( 'NONE', #5672, .T. ) ;
#10199 = FACE_OUTER_BOUND ( 'NONE', #18199, .T. ) ;
#10200 = ORIENTED_EDGE ( 'NONE', *, *, #36845, .F. ) ;
#10201 =( NAMED_UNIT ( * ) PLANE_ANGLE_UNIT ( ) SI_UNIT ( $, .RADIAN. ) );
#10202 = CIRCLE ( 'NONE', #10835, 7.744449365083023729 ) ;
#10203 = VECTOR ( 'NONE', #29206, 1000.000000000000000 ) ;
#10204 = ORIENTED_EDGE ( 'NONE', *, *, #16173, .T. ) ;
#10205 = CARTESIAN_POINT ( 'NONE',  ( 79.40660192983035870, 64.44177602733365973, -3.564905221331804874 ) ) ;
#10206 =( BOUNDED_CURVE ( )  B_SPLINE_CURVE ( 3, ( #38960, #4019, #1520, #16729 ),
 .UNSPECIFIED., .F., .T. ) 
 B_SPLINE_CURVE_WITH_KNOTS ( ( 4, 4 ),
 ( 1.381924640371167134, 1.574767692156074705 ),
 .UNSPECIFIED. ) 
 CURVE ( )  GEOMETRIC_REPRESENTATION_ITEM ( )  RATIONAL_B_SPLINE_CURVE ( ( 1.000000000000000000, 0.9969033633783033199, 0.9969033633783033199, 1.000000000000000000 ) ) 
 REPRESENTATION_ITEM ( '' )  );
#10207 = CARTESIAN_POINT ( 'NONE',  ( 80.91969899470544192, 61.54505855127009539, 2.326060681237265726 ) ) ;
#10208 = CARTESIAN_POINT ( 'NONE',  ( -1.304540412773448566, -31.16068525338094730, 6.863904403958575706 ) ) ;
#10209 = AXIS2_PLACEMENT_3D ( 'NONE', #13746, #23215, #35779 ) ;
#10210 = CARTESIAN_POINT ( 'NONE',  ( 25.83360062294675075, 1.871733103193846448, 4.238356183839651514 ) ) ;
#10211 = B_SPLINE_CURVE_WITH_KNOTS ( 'NONE', 3,
 ( #37231, #2480, #27153, #30457, #11286, #9026, #18083, #27563, #21399, #21605 ),
 .UNSPECIFIED., .F., .F.,
 ( 4, 3, 3, 4 ),
 ( 0.0002170292169044785754, 0.0002420761345915984773, 0.0002723302478207019375, 0.0002816811360866781563 ),
 .UNSPECIFIED. ) ;
#10212 = CARTESIAN_POINT ( 'NONE',  ( -0.5323850565855563488, -32.26524778338716004, 7.743886751744255115 ) ) ;
#10213 = CARTESIAN_POINT ( 'NONE',  ( -1.795296463333102999, -29.46015129865232751, 7.766640943994648438 ) ) ;
#10214 = CARTESIAN_POINT ( 'NONE',  ( 21.85643539959776049, -15.24219007203948983, -1.854490019360333086 ) ) ;
#10215 = PRODUCT_RELATED_PRODUCT_CATEGORY ( 'part', '', ( #20310 ) ) ;
#10216 = CARTESIAN_POINT ( 'NONE',  ( 22.39823815405979701, 4.874039138771919077, -3.101746399076472205 ) ) ;
#10217 = VERTEX_POINT ( 'NONE', #23896 ) ;
#10218 = CARTESIAN_POINT ( 'NONE',  ( 5.200356001372292702, -29.55434199642423465, 7.638132480492515697 ) ) ;
#10219 = VERTEX_POINT ( 'NONE', #20814 ) ;
#10220 = CARTESIAN_POINT ( 'NONE',  ( 3.896194328649233984, -32.16578144256224903, 7.635761828346577573 ) ) ;
#10221 = DIRECTION ( 'NONE',  ( 0.000000000000000000, 0.000000000000000000, 1.000000000000000000 ) ) ;
#10222 = CARTESIAN_POINT ( 'NONE',  ( -73.23924125533064000, -0.08275262721004308930, -9.788968532873301598 ) ) ;
#10223 = CARTESIAN_POINT ( 'NONE',  ( 4.370302737341240196, -27.30684236520528785, 7.750000000000000000 ) ) ;
#10224 = DIRECTION ( 'NONE',  ( -0.000000000000000000, 1.000000000000000000, -0.000000000000000000 ) ) ;
#10225 = CARTESIAN_POINT ( 'NONE',  ( 81.32870865761989876, 61.49729006283357080, 1.754135932968025724 ) ) ;
#10226 = CARTESIAN_POINT ( 'NONE',  ( 85.17103880321602105, 1.638380925414154587, -5.247232096711407223 ) ) ;
#10227 = CYLINDRICAL_SURFACE ( 'NONE', #1003, 0.9999999999999977796 ) ;
#10228 = FACE_OUTER_BOUND ( 'NONE', #19075, .T. ) ;
#10229 = CARTESIAN_POINT ( 'NONE',  ( -1.644402349235647653, -30.18018250254910839, 7.643333865083955736 ) ) ;
#10230 = EDGE_CURVE ( 'NONE', #30840, #33369, #33597, .T. ) ;
#10231 = VECTOR ( 'NONE', #20920, 1000.000000000000000 ) ;
#10232 = AXIS2_PLACEMENT_3D ( 'NONE', #5193, #36890, #27815 ) ;
#10233 = CARTESIAN_POINT ( 'NONE',  ( -64.94969296618708654, 34.86786693855311370, 6.612442482648480002 ) ) ;
#10234 = DIRECTION ( 'NONE',  ( -0.000000000000000000, -1.000000000000000000, -0.000000000000000000 ) ) ;
#10235 = EDGE_CURVE ( 'NONE', #6673, #39610, #12374, .T. ) ;
#10236 = DIRECTION ( 'NONE',  ( -1.000000000000000000, 0.000000000000000000, 0.000000000000000000 ) ) ;
#10237 = CARTESIAN_POINT ( 'NONE',  ( -0.9920141182173938255, -27.33364690670997277, 7.640616322432102869 ) ) ;
#10238 = B_SPLINE_CURVE_WITH_KNOTS ( 'NONE', 3,
 ( #39447, #32896, #29398, #23418, #11237, #13751, #20720, #33306, #17618, #13941, #2016, #39041, #26314, #38849, #35982, #20312, #4683, #17217, #29789 ),
 .UNSPECIFIED., .F., .F.,
 ( 4, 3, 3, 3, 3, 3, 4 ),
 ( 0.000000000000000000, 2.546128104244741393E-05, 5.711050680483831731E-05, 8.113074941675599164E-05, 0.0001053129305727048962, 0.0001360598016347087881, 0.0001612931755702011341 ),
 .UNSPECIFIED. ) ;
#10239 = CARTESIAN_POINT ( 'NONE',  ( 69.13527637438681950, 58.97494527044376866, 3.984982412582155575 ) ) ;
#10240 = CARTESIAN_POINT ( 'NONE',  ( 33.62807682128043751, -1.230511385543872294, 5.454872704708900066 ) ) ;
#10241 = VECTOR ( 'NONE', #21878, 1000.000000000000114 ) ;
#10242 = DIRECTION ( 'NONE',  ( -0.000000000000000000, -0.000000000000000000, 1.000000000000000000 ) ) ;
#10243 = CARTESIAN_POINT ( 'NONE',  ( 86.36291470068610465, 1.350799773688788674, 4.987004148466622766 ) ) ;
#10244 = ORIENTED_EDGE ( 'NONE', *, *, #10002, .T. ) ;
#10246 = CARTESIAN_POINT ( 'NONE',  ( 4.817466283527966020, -30.92780942099031449, 6.959317978105159952 ) ) ;
#10245 = CARTESIAN_POINT ( 'NONE',  ( 80.65352406091058413, 63.67746643299658160, -3.602832836245130288 ) ) ;
#10247 = CARTESIAN_POINT ( 'NONE',  ( -1.238581594385354201, -27.66927444853685714, 6.903112506833889661 ) ) ;
#10248 = ORIENTED_EDGE ( 'NONE', *, *, #17117, .F. ) ;
#10249 = LINE ( 'NONE', #20315, #12204 ) ;
#10250 = VERTEX_POINT ( 'NONE', #24104 ) ;
#10251 = CARTESIAN_POINT ( 'NONE',  ( 4.879927719065142000, -33.52973165241049713, 7.013842709614101167 ) ) ;
#10252 = VERTEX_POINT ( 'NONE', #3743 ) ;
#10253 = CARTESIAN_POINT ( 'NONE',  ( 79.53095237740755863, 64.90064992126218613, -3.392181771880278696 ) ) ;
#10254 = DIRECTION ( 'NONE',  ( -1.000000000000000000, 0.000000000000000000, 0.000000000000000000 ) ) ;
#10255 = CARTESIAN_POINT ( 'NONE',  ( 21.83945981511907064, 2.416022838233994552, 5.659870449405054238 ) ) ;
#10257 = ORIENTED_EDGE ( 'NONE', *, *, #27330, .T. ) ;
#10256 = ORIENTED_EDGE ( 'NONE', *, *, #25717, .F. ) ;
#10258 = CARTESIAN_POINT ( 'NONE',  ( 79.16788024942138691, 66.21349342525118686, -1.524764441711168095 ) ) ;
#10259 = ADVANCED_FACE ( 'NONE', ( #25547 ), #12370, .F. ) ;
#10260 = CARTESIAN_POINT ( 'NONE',  ( 5.026976287143079425, -30.27265651311746453, 6.864276522220859711 ) ) ;
#10262 = CARTESIAN_POINT ( 'NONE',  ( 85.76750662938394498, 2.019590379147275794, 3.841493691465702298 ) ) ;
#10261 = CARTESIAN_POINT ( 'NONE',  ( -58.90847777598104784, 28.53357273443418762, -6.181373327462416967 ) ) ;
#10263 = CARTESIAN_POINT ( 'NONE',  ( -1.261279527196320194, -27.90004417849888085, 7.712764235869103757 ) ) ;
#10264 = CARTESIAN_POINT ( 'NONE',  ( 69.65195751129601831, 59.35873293165669651, 3.965028736237012907 ) ) ;
#10265 = CARTESIAN_POINT ( 'NONE',  ( 23.41724364834474414, 3.428523892220677993, -3.609970445808396544 ) ) ;
#10266 = ORIENTED_EDGE ( 'NONE', *, *, #40329, .T. ) ;
#10267 = CARTESIAN_POINT ( 'NONE',  ( 2.329922961629665945, -33.01285193709216514, 7.743886751744252450 ) ) ;
#10268 = AXIS2_PLACEMENT_3D ( 'NONE', #16403, #32873, #10430 ) ;
#10269 = B_SPLINE_CURVE_WITH_KNOTS ( 'NONE', 3,
 ( #13178, #10079, #32534, #13577, #22665, #22858, #35230, #38683, #7001, #15504, #4333, #19567, #10479, #3941, #16461, #29034, #35430, #838, #13370, #7199, #4132, #30235, #10878, #23834, #2250, #14176, #24252, #14773, #5121, #27344, #17654 ),
 .UNSPECIFIED., .F., .F.,
 ( 4, 3, 3, 3, 3, 3, 3, 3, 3, 3, 4 ),
 ( 1.734723475976807094E-18, 2.999644130997709601E-05, 6.002588995694745322E-05, 8.960886084588071728E-05, 0.0001190604700446499739, 0.0001489538463052708260, 0.0001796139255493996438, 0.0002109707048517061299, 0.0002426195318110375249, 0.0002740640997890022267, 0.0002849778069099830643 ),
 .UNSPECIFIED. ) ;
#10270 = EDGE_LOOP ( 'NONE', ( #32656, #3801, #442, #2743 ) ) ;
#10271 = CARTESIAN_POINT ( 'NONE',  ( 21.85643539959779957, 3.623429283794106670, 13.13803316603621241 ) ) ;
#10272 = CARTESIAN_POINT ( 'NONE',  ( 20.24823138111575105, 11.68787526792862153, 3.842642712662352800 ) ) ;
#10273 = VERTEX_POINT ( 'NONE', #31726 ) ;
#10274 = CARTESIAN_POINT ( 'NONE',  ( 0.4685308032799795352, -32.73893911755277486, 6.874555630061442102 ) ) ;
#10275 = CARTESIAN_POINT ( 'NONE',  ( 81.16506502659913735, 61.30232764367859488, 1.065084354002949762 ) ) ;
#10276 = CARTESIAN_POINT ( 'NONE',  ( 84.82990711808488982, 3.023024660489734394, 1.086629044751433293 ) ) ;
#10277 = ORIENTED_EDGE ( 'NONE', *, *, #14671, .F. ) ;
#10278 = B_SPLINE_CURVE_WITH_KNOTS ( 'NONE', 3,
 ( #15185, #15392, #39899, #28153, #12087, #5729, #40707, #36811, #18267, #14767, #30652, #24875, #40491, #37213, #25083, #30859 ),
 .UNSPECIFIED., .F., .F.,
 ( 4, 2, 2, 2, 2, 2, 2, 4 ),
 ( 0.000000000000000000, 0.0006740595217997351124, 0.001348119043599470225, 0.002696238087198940449, 0.004044357130798413059, 0.005392476174397886970, 0.008088714261596836527, 0.01078495234879578782 ),
 .UNSPECIFIED. ) ;
#10279 = CARTESIAN_POINT ( 'NONE',  ( 2.735183283186696013, -32.91346230508531789, 7.011627023500183853 ) ) ;
#10280 = CARTESIAN_POINT ( 'NONE',  ( 14.65850939258177554, -5.614383887714384791, 2.494212926738383906 ) ) ;
#10281 = CARTESIAN_POINT ( 'NONE',  ( 37.01706860164229340, -2.756673952631257141, 5.983806835110248024 ) ) ;
#10282 = CARTESIAN_POINT ( 'NONE',  ( -17.69482985384421880, -29.56993018339339940, 2.500000000000000000 ) ) ;
#10283 = ADVANCED_FACE ( 'NONE', ( #16068 ), #28839, .T. ) ;
#10284 = CARTESIAN_POINT ( 'NONE',  ( 22.92126275026679494, 2.653310250737696663, -3.783815423649973031 ) ) ;
#10285 = DIRECTION ( 'NONE',  ( -0.000000000000000000, 1.000000000000000000, -0.000000000000000000 ) ) ;
#10286 =( REPRESENTATION_RELATIONSHIP ('NONE','NONE', #24012, #39290 ) REPRESENTATION_RELATIONSHIP_WITH_TRANSFORMATION ( #17781 )SHAPE_REPRESENTATION_RELATIONSHIP( ) );
#10287 = CARTESIAN_POINT ( 'NONE',  ( 85.48109816848365483, 1.178641903994587903, 5.687362864452985889 ) ) ;
#10288 = CARTESIAN_POINT ( 'NONE',  ( 3.858226607809892794, -26.94243297489357403, 7.692469944509195301 ) ) ;
#10289 = CARTESIAN_POINT ( 'NONE',  ( -20.44874870218064444, -26.64985754041175525, 6.700000000000000178 ) ) ;
#10290 = CARTESIAN_POINT ( 'NONE',  ( 29.62473861780153683, -3.849278697187920706, 4.318228108797867115 ) ) ;
#10291 = VERTEX_POINT ( 'NONE', #3147 ) ;
#10292 = ORIENTED_EDGE ( 'NONE', *, *, #19440, .F. ) ;
#10293 = CARTESIAN_POINT ( 'NONE',  ( 23.38512868750360596, 3.559325214671839266, 3.095447384079575315 ) ) ;
#10294 = CARTESIAN_POINT ( 'NONE',  ( 1.597520268100450780, -33.06375448864240241, 7.771081512783701406 ) ) ;
#10295 = AXIS2_PLACEMENT_3D ( 'NONE', #17128, #26227, #7472 ) ;
#10296 = CARTESIAN_POINT ( 'NONE',  ( -62.99901854238117238, 37.98537211837078331, -4.070195263748868975 ) ) ;
#10297 = CARTESIAN_POINT ( 'NONE',  ( 87.60931828755812489, -2.129004962406701562, 3.117860766101097525 ) ) ;
#10298 = AXIS2_PLACEMENT_3D ( 'NONE', #33792, #24507, #2296 ) ;
#10299 = ORIENTED_EDGE ( 'NONE', *, *, #27668, .F. ) ;
#10300 = CARTESIAN_POINT ( 'NONE',  ( 3.013805019779557171, -26.32571329602632559, 7.751599049952173637 ) ) ;
#10301 = CARTESIAN_POINT ( 'NONE',  ( 2.293051275415638912, -26.12047319804549517, 7.637894019485641728 ) ) ;
#10302 = ORIENTED_EDGE ( 'NONE', *, *, #36302, .F. ) ;
#10303 = CARTESIAN_POINT ( 'NONE',  ( -65.15514661499977933, 34.97220226750606997, 6.888442104241535802 ) ) ;
#10304 = EDGE_CURVE ( 'NONE', #39924, #39141, #5301, .T. ) ;
#10305 = CARTESIAN_POINT ( 'NONE',  ( 5.015318072754217482, -33.54151383920058294, 7.635761828346577573 ) ) ;
#10306 = VERTEX_POINT ( 'NONE', #9470 ) ;
#10307 = CARTESIAN_POINT ( 'NONE',  ( 80.61888529134419912, 66.16066543623874452, -1.646077502936216685 ) ) ;
#10308 = CARTESIAN_POINT ( 'NONE',  ( -1.231209508105928441, -31.29206202033822137, 7.652160403243386533 ) ) ;
#10309 = VERTEX_POINT ( 'NONE', #21848 ) ;
#10310 = CARTESIAN_POINT ( 'NONE',  ( 76.06955384389377173, 61.76325957217478191, -3.887901781368106491 ) ) ;
#10312 = CARTESIAN_POINT ( 'NONE',  ( 4.454149367520055414, -27.41100356581296182, 7.761113333116790081 ) ) ;
#10311 = DIRECTION ( 'NONE',  ( -0.000000000000000000, -0.000000000000000000, 1.000000000000000000 ) ) ;
#10313 = DIRECTION ( 'NONE',  ( 0.000000000000000000, 0.000000000000000000, -1.000000000000000000 ) ) ;
#10314 = ADVANCED_FACE ( 'NONE', ( #22467 ), #15660, .T. ) ;
#10315 = CARTESIAN_POINT ( 'NONE',  ( 77.14378789031550809, 60.95143994403615295, 3.590981437852719171 ) ) ;
#10316 = CARTESIAN_POINT ( 'NONE',  ( 4.417542878868808032, -27.52612349775301581, 6.887945620086116882 ) ) ;
#10317 = ADVANCED_FACE ( 'NONE', ( #19368 ), #38088, .T. ) ;
#10318 = VECTOR ( 'NONE', #13090, 999.9999999999998863 ) ;
#10319 = DIRECTION ( 'NONE',  ( 0.000000000000000000, 0.000000000000000000, 1.000000000000000000 ) ) ;
#10320 = CARTESIAN_POINT ( 'NONE',  ( 22.01541346579904967, 4.834729283906541220, -3.642368534677343117 ) ) ;
#10321 = CARTESIAN_POINT ( 'NONE',  ( 1.664433243520564654, -26.07011488755866679, 7.695279973900954751 ) ) ;
#10322 = CARTESIAN_POINT ( 'NONE',  ( 78.92300404249586165, 66.17133619070195039, 1.270639542487624896 ) ) ;
#10323 =( BOUNDED_CURVE ( )  B_SPLINE_CURVE ( 3, ( #17566, #8513, #1969, #14488 ),
 .UNSPECIFIED., .F., .F. ) 
 B_SPLINE_CURVE_WITH_KNOTS ( ( 4, 4 ),
 ( 4.748221474220559735, 4.941946782021394924 ),
 .UNSPECIFIED. ) 
 CURVE ( )  GEOMETRIC_REPRESENTATION_ITEM ( )  RATIONAL_B_SPLINE_CURVE ( ( 1.000000000000000000, 0.9968749865767494445, 0.9968749865767494445, 1.000000000000000000 ) ) 
 REPRESENTATION_ITEM ( '' )  );
#10324 = CARTESIAN_POINT ( 'NONE',  ( -0.1220456601027410937, -32.55802789346970627, 6.865554069792297653 ) ) ;
#10325 = CARTESIAN_POINT ( 'NONE',  ( 26.92542807167190944, 1.449366069832211279, 5.022290288739529984 ) ) ;
#10326 = AXIS2_PLACEMENT_3D ( 'NONE', #11642, #36377, #8355 ) ;
#10327 = CARTESIAN_POINT ( 'NONE',  ( -69.92837670882107659, -0.7829914368874777431, 5.916079783099621459 ) ) ;
#10328 = AXIS2_PLACEMENT_3D ( 'NONE', #24607, #37163, #16744 ) ;
#10329 = CARTESIAN_POINT ( 'NONE',  ( 32.03973861597579287, -5.079083921188654926, 0.4704245571143086391 ) ) ;
#10330 = AXIS2_PLACEMENT_3D ( 'NONE', #32194, #3994, #3595 ) ;
#10331 = CARTESIAN_POINT ( 'NONE',  ( 4.722241970102593278, -31.32479717685847476, 7.773839561854635427 ) ) ;
#10332 = EDGE_LOOP ( 'NONE', ( #28949, #19110, #36047, #27360, #37184 ) ) ;
#10333 = CARTESIAN_POINT ( 'NONE',  ( -0.5636438011847132445, -32.10651479984770873, 6.864651958020304257 ) ) ;
#10334 = CARTESIAN_POINT ( 'NONE',  ( 3.930782290905703746, -26.87263809153695249, 7.651421919295148477 ) ) ;
#10335 = EDGE_CURVE ( 'NONE', #1123, #31321, #15943, .T. ) ;
#10336 = CARTESIAN_POINT ( 'NONE',  ( 36.73503357909203260, -2.304591497473642558, -5.935222444422922905 ) ) ;
#10337 = CARTESIAN_POINT ( 'NONE',  ( 1.107165259060771456, -32.91777789440434532, 7.769368695748486431 ) ) ;
#10338 = DIRECTION ( 'NONE',  ( -0.000000000000000000, 1.000000000000000000, -0.000000000000000000 ) ) ;
#10339 = CARTESIAN_POINT ( 'NONE',  ( 3.425693392627762179, -32.49966342626535010, 7.730758795053806587 ) ) ;
#10340 = CARTESIAN_POINT ( 'NONE',  ( 2.218073121325518482, -32.93030207017181965, 6.874555630061442102 ) ) ;
#10341 = CARTESIAN_POINT ( 'NONE',  ( 5.796245933686637208, -28.19952006637477027, 6.894806418505347700 ) ) ;
#10342 = CARTESIAN_POINT ( 'NONE',  ( -63.05049812975219226, 38.43447230638341949, -4.010972415401406366 ) ) ;
#10343 = B_SPLINE_CURVE_WITH_KNOTS ( 'NONE', 3,
 ( #10953, #10558, #13861, #1719, #35502, #29513, #33007, #35701, #23134, #26822, #20428, #1322, #1515, #20033 ),
 .UNSPECIFIED., .F., .F.,
 ( 4, 2, 2, 2, 2, 2, 4 ),
 ( 2.818925648462311528E-18, 0.0006285028710944130402, 0.001257005742188823261, 0.001885508613283233591, 0.002514011484377643921, 0.003771017226566485830, 0.005028022968755326873 ),
 .UNSPECIFIED. ) ;
#10344 = DIRECTION ( 'NONE',  ( -0.000000000000000000, -0.000000000000000000, 1.000000000000000000 ) ) ;
#10345 = ORIENTED_EDGE ( 'NONE', *, *, #19659, .F. ) ;
#10346 = CARTESIAN_POINT ( 'NONE',  ( 37.02980894656261057, -2.495571335640368371, 5.974001483408611257 ) ) ;
#10347 = DIRECTION ( 'NONE',  ( 0.000000000000000000, 1.000000000000000000, 0.000000000000000000 ) ) ;
#10348 = CARTESIAN_POINT ( 'NONE',  ( 67.72966869545554403, 58.29280778740498192, -3.997461085607385556 ) ) ;
#10349 = ADVANCED_FACE ( 'NONE', ( #439 ), #6612, .F. ) ;
#10350 = CARTESIAN_POINT ( 'NONE',  ( 4.713340623123058570, -27.78888299018493058, 7.695279973900954751 ) ) ;
#10351 = VERTEX_POINT ( 'NONE', #35237 ) ;
#10352 = CYLINDRICAL_SURFACE ( 'NONE', #27865, 0.1000000000000028644 ) ;
#10353 = CARTESIAN_POINT ( 'NONE',  ( -1.600411900518525110, -28.40601156757937673, 7.710604733652632881 ) ) ;
#10354 = CARTESIAN_POINT ( 'NONE',  ( 23.23474455812838713, 3.274026224173547828, 3.847451402220932959 ) ) ;
#10355 = CARTESIAN_POINT ( 'NONE',  ( 5.046722968108102947, -28.54421561425872866, 6.998987538705433664 ) ) ;
#10356 = CARTESIAN_POINT ( 'NONE',  ( 3.477237270422150139, -26.55450084266673727, 6.894806418505347700 ) ) ;
#10357 = VECTOR ( 'NONE', #11983, 1000.000000000000000 ) ;
#10358 = VECTOR ( 'NONE', #35201, 1000.000000000000114 ) ;
#10359 = CARTESIAN_POINT ( 'NONE',  ( -55.16612787639756732, 31.23053227951973199, 1.484562114140385747 ) ) ;
#10360 = EDGE_LOOP ( 'NONE', ( #12598, #340, #15055, #32572 ) ) ;
#10361 = CARTESIAN_POINT ( 'NONE',  ( 22.61528281558029008, 4.620618817536152889, 3.048381724597784892 ) ) ;
#10362 = CARTESIAN_POINT ( 'NONE',  ( 4.945445480008764605, -30.88065529806472043, 7.754798119455333705 ) ) ;
#10363 = CARTESIAN_POINT ( 'NONE',  ( 81.20826633916702519, 61.35171532218112134, 1.496866203714591892 ) ) ;
#10364 = DIRECTION ( 'NONE',  ( -0.000000000000000000, -0.000000000000000000, -1.000000000000000000 ) ) ;
#10365 = VERTEX_POINT ( 'NONE', #19575 ) ;
#10366 = CARTESIAN_POINT ( 'NONE',  ( 77.82439497328331868, 65.16220298991649429, -2.551779361026667026 ) ) ;
#10368 = CARTESIAN_POINT ( 'NONE',  ( -1.740083682737729731, -28.92717035510830925, 6.890142680165448397 ) ) ;
#10367 = CARTESIAN_POINT ( 'NONE',  ( 21.79691714197424091, 0.2351871378864240913, 8.326263741760431714 ) ) ;
#10369 = EDGE_CURVE ( 'NONE', #37105, #19656, #26359, .T. ) ;
#10370 = CARTESIAN_POINT ( 'NONE',  ( 80.78189192732895663, 64.90162691772428616, -3.235508711551936756 ) ) ;
#10371 = CARTESIAN_POINT ( 'NONE',  ( 77.95070745440513349, 65.53481705947537250, 1.908681007153592235 ) ) ;
#10372 = EDGE_CURVE ( 'NONE', #12131, #15868, #23461, .T. ) ;
#10373 = CARTESIAN_POINT ( 'NONE',  ( -1.078675913592196167, -26.64985754041175525, 6.700000000000000178 ) ) ;
#10374 = CARTESIAN_POINT ( 'NONE',  ( 82.18073233876091876, 62.22941084722771166, 1.168532795813725045 ) ) ;
#10375 = CARTESIAN_POINT ( 'NONE',  ( 25.11437021580303863, 164.7550792202006562, 1.000000000000000000 ) ) ;
#10376 = AXIS2_PLACEMENT_3D ( 'NONE', #20737, #24025, #18050 ) ;
#10377 = CARTESIAN_POINT ( 'NONE',  ( 25.36335546794393281, -3.584835346285432767, 4.690180580146940059 ) ) ;
#10378 = ORIENTED_EDGE ( 'NONE', *, *, #22349, .T. ) ;
#10379 = CARTESIAN_POINT ( 'NONE',  ( -78.59183336369314077, -5.357290617477898031, 6.436894183391851598 ) ) ;
#10380 = DIRECTION ( 'NONE',  ( -0.000000000000000000, -0.000000000000000000, -1.000000000000000000 ) ) ;
#10381 = DIRECTION ( 'NONE',  ( 0.000000000000000000, 0.000000000000000000, 1.000000000000000000 ) ) ;
#10382 = CARTESIAN_POINT ( 'NONE',  ( 22.43263433131228268, 5.122865301372990565, 2.446692766515739859 ) ) ;
#10383 = ORIENTED_EDGE ( 'NONE', *, *, #35521, .T. ) ;
#10384 = CARTESIAN_POINT ( 'NONE',  ( 35.36788826667455510, -3.790803511439575946, -5.512024906129279422 ) ) ;
#10385 = DIRECTION ( 'NONE',  ( -0.9396926207859005453, -0.3420201433256903067, 0.000000000000000000 ) ) ;
#10386 = CARTESIAN_POINT ( 'NONE',  ( 3.300060709366284595, -32.68297658758336155, 7.011627023500182965 ) ) ;
#10387 = CARTESIAN_POINT ( 'NONE',  ( -1.071744829033150603, -31.70657895489327416, 6.875780273367532835 ) ) ;
#10388 = DIRECTION ( 'NONE',  ( 0.000000000000000000, 0.000000000000000000, 1.000000000000000000 ) ) ;
#10389 = CARTESIAN_POINT ( 'NONE',  ( -0.5758935922563414023, -26.91125798201889197, 7.678495282201408756 ) ) ;
#10390 = CARTESIAN_POINT ( 'NONE',  ( -33.07867591359219972, -26.64985754041175525, 6.700000000000000178 ) ) ;
#10391 = AXIS2_PLACEMENT_3D ( 'NONE', #36215, #35630, #7404 ) ;
#10392 = FACE_OUTER_BOUND ( 'NONE', #16969, .T. ) ;
#10393 = CARTESIAN_POINT ( 'NONE',  ( 26.10580188794843792, 1.913936627547451641, -4.230755467540477710 ) ) ;
#10394 = CARTESIAN_POINT ( 'NONE',  ( 30.05259702970372260, 1.006150772074058564, -4.336635385246468744 ) ) ;
#10395 = CARTESIAN_POINT ( 'NONE',  ( 16.64247417353310254, 12.36459659714428483, -2.500000000000000888 ) ) ;
#10396 = CARTESIAN_POINT ( 'NONE',  ( 2.253737889363386593, -33.02591140679692927, 6.875671892026062437 ) ) ;
#10397 = ORIENTED_EDGE ( 'NONE', *, *, #17999, .T. ) ;
#10398 = ORIENTED_EDGE ( 'NONE', *, *, #28772, .F. ) ;
#10399 = CARTESIAN_POINT ( 'NONE',  ( 66.54635149611212341, 57.90010100995254305, 3.999344142520906864 ) ) ;
#10400 = CARTESIAN_POINT ( 'NONE',  ( 86.09116122586011954, 0.08319669091220074919, -6.006182420748226392 ) ) ;
#10401 = EDGE_LOOP ( 'NONE', ( #13058, #2978, #13710, #25320 ) ) ;
#10402 = CARTESIAN_POINT ( 'NONE',  ( 27.43879754216082389, 0.9604377377020558715, 4.488885984917203587 ) ) ;
#10403 =( LENGTH_UNIT ( ) NAMED_UNIT ( * ) SI_UNIT ( .MILLI., .METRE. ) );
#10404 = EDGE_CURVE ( 'NONE', #21932, #21394, #36219, .T. ) ;
#10405 = CARTESIAN_POINT ( 'NONE',  ( 2.309267857255833167, -32.91496648640696776, 7.748216051605118615 ) ) ;
#10406 = DIRECTION ( 'NONE',  ( 0.000000000000000000, 0.000000000000000000, 1.000000000000000000 ) ) ;
#10407 = VERTEX_POINT ( 'NONE', #35833 ) ;
#10408 = DIRECTION ( 'NONE',  ( 0.000000000000000000, 0.000000000000000000, 1.000000000000000000 ) ) ;
#10409 = ORIENTED_EDGE ( 'NONE', *, *, #24798, .T. ) ;
#10410 = EDGE_CURVE ( 'NONE', #13769, #28407, #17260, .T. ) ;
#10411 = ORIENTED_EDGE ( 'NONE', *, *, #15379, .T. ) ;
#10412 = CARTESIAN_POINT ( 'NONE',  ( 80.32689410753103232, 62.53373119284189130, -3.467090974304448459 ) ) ;
#10413 = CARTESIAN_POINT ( 'NONE',  ( 33.78306522148626101, -4.833110834643807863, 3.502350965566474628 ) ) ;
#10414 = CARTESIAN_POINT ( 'NONE',  ( 78.94919473400565835, 65.41189549592698427, 2.864416008774272271 ) ) ;
#10415 = EDGE_CURVE ( 'NONE', #19773, #17567, #35155, .T. ) ;
#10416 = CIRCLE ( 'NONE', #570, 0.1000000000000028644 ) ;
#10418 = EDGE_CURVE ( 'NONE', #28407, #3677, #14511, .T. ) ;
#10417 = DIRECTION ( 'NONE',  ( -7.826543628040252284E-17, 1.000000000000000000, 0.000000000000000000 ) ) ;
#10419 = DIRECTION ( 'NONE',  ( 1.000000000000000000, 0.000000000000000000, 0.000000000000000000 ) ) ;
#10420 = LINE ( 'NONE', #16393, #9740 ) ;
#10421 = CARTESIAN_POINT ( 'NONE',  ( 33.81163260347297239, -4.968337719301128885, -3.151236393681405623 ) ) ;
#10422 = CARTESIAN_POINT ( 'NONE',  ( 3.369155479471896530, -26.60763004909045293, 7.703977250142851396 ) ) ;
#10423 = ORIENTED_EDGE ( 'NONE', *, *, #21751, .F. ) ;
#10424 = CARTESIAN_POINT ( 'NONE',  ( 66.27376694608931018, 57.73522568913554665, -4.000000000000000000 ) ) ;
#10425 = FACE_OUTER_BOUND ( 'NONE', #11359, .T. ) ;
#10426 = CARTESIAN_POINT ( 'NONE',  ( -0.5986408314062141578, -32.19260107032493323, 7.782861076432727288 ) ) ;
#10427 = CARTESIAN_POINT ( 'NONE',  ( -72.95788378915689520, 3.814940674406429810, -10.95087388501848125 ) ) ;
#10428 = AXIS2_PLACEMENT_3D ( 'NONE', #1478, #39123, #16346 ) ;
#10429 = CARTESIAN_POINT ( 'NONE',  ( -72.84815947045233031, 2.429809908903243443, 12.50000000000000000 ) ) ;
#10430 = DIRECTION ( 'NONE',  ( -0.8660254037844261621, -0.5000000000000215383, 0.000000000000000000 ) ) ;
#10431 = CARTESIAN_POINT ( 'NONE',  ( 81.39824655423383604, 62.07766870923516933, 2.596981798947347819 ) ) ;
#10432 = CARTESIAN_POINT ( 'NONE',  ( 86.14505873727070195, -0.01797735283943463491, 5.995667628870159582 ) ) ;
#10433 = DIRECTION ( 'NONE',  ( 0.000000000000000000, 1.000000000000000000, 0.000000000000000000 ) ) ;
#10434 = DIRECTION ( 'NONE',  ( -0.6427876096865235978, 0.7660444431189911141, 0.000000000000000000 ) ) ;
#10435 = B_SPLINE_CURVE_WITH_KNOTS ( 'NONE', 3,
 ( #24056, #36624, #30456, #28169, #31684, #6968, #38048, #23527, #13144, #21098, #32491, #5446 ),
 .UNSPECIFIED., .F., .F.,
 ( 4, 2, 2, 2, 2, 4 ),
 ( 0.004696307191636101344, 0.005283442520392493159, 0.005870577849148884975, 0.006164145513527088255, 0.006457713177905292402, 0.007044848506661660799 ),
 .UNSPECIFIED. ) ;
#10436 = CARTESIAN_POINT ( 'NONE',  ( -0.4128411470553862705, -26.90640809309241632, 6.866852738645443210 ) ) ;
#10437 = CARTESIAN_POINT ( 'NONE',  ( 4.956151073483226810, -30.57389002924307775, 7.139196562012274150 ) ) ;
#10438 = CARTESIAN_POINT ( 'NONE',  ( -1.001523146005661946, -27.34514595843441498, 7.670465701733755637 ) ) ;
#10439 = CARTESIAN_POINT ( 'NONE',  ( 36.14162845619620157, -3.143484948803114243, 5.847173227813405205 ) ) ;
#10440 = CARTESIAN_POINT ( 'NONE',  ( -64.08758708074091714, 24.84364830758654108, 3.800414904976363140 ) ) ;
#10441 = CARTESIAN_POINT ( 'NONE',  ( 87.56526962053540331, 0.0002576605070852033049, 4.866394609412610706 ) ) ;
#10443 = CARTESIAN_POINT ( 'NONE',  ( 4.823856784610486059, -30.91304441079773468, 6.903372536218454592 ) ) ;
#10442 = CARTESIAN_POINT ( 'NONE',  ( 81.18025391627377019, 61.34316975053406651, -1.531260274641951913 ) ) ;
#10444 = DIRECTION ( 'NONE',  ( 0.000000000000000000, -0.1369933068947546406, 0.9905719730872863948 ) ) ;
#10445 = CARTESIAN_POINT ( 'NONE',  ( 88.16566304253608166, -0.6741327274749846499, -2.283436234569833800 ) ) ;
#10446 = ORIENTED_EDGE ( 'NONE', *, *, #10418, .F. ) ;
#10447 = CARTESIAN_POINT ( 'NONE',  ( 2.921324086407800280, -26.64985754041175525, 6.800000000000000711 ) ) ;
#10448 = ORIENTED_EDGE ( 'NONE', *, *, #3834, .T. ) ;
#10449 = DIRECTION ( 'NONE',  ( -0.5000000000000039968, 0.8660254037844363761, -0.000000000000000000 ) ) ;
#10451 = ORIENTED_EDGE ( 'NONE', *, *, #4600, .F. ) ;
#10450 = ORIENTED_EDGE ( 'NONE', *, *, #32226, .T. ) ;
#10452 = CARTESIAN_POINT ( 'NONE',  ( 78.75977295323076532, 65.93644120262121078, -1.938154327158300827 ) ) ;
#10453 = DIRECTION ( 'NONE',  ( 0.000000000000000000, -0.9994119649315837961, -0.03428883712799970368 ) ) ;
#10454 = CARTESIAN_POINT ( 'NONE',  ( 24.68943462063005967, 2.063637610377018206, 4.241669502777529743 ) ) ;
#10456 = ORIENTED_EDGE ( 'NONE', *, *, #3427, .F. ) ;
#10455 = ORIENTED_EDGE ( 'NONE', *, *, #18923, .T. ) ;
#10457 = EDGE_CURVE ( 'NONE', #13597, #33969, #32746, .T. ) ;
#10458 = EDGE_CURVE ( 'NONE', #39035, #25329, #846, .T. ) ;
#10460 = EDGE_CURVE ( 'NONE', #30200, #34241, #34960, .T. ) ;
#10459 = CARTESIAN_POINT ( 'NONE',  ( -63.08758708074093136, 43.61223004741322740, 4.000000000000000000 ) ) ;
#10461 = B_SPLINE_CURVE_WITH_KNOTS ( 'NONE', 3,
 ( #38976, #10582, #7100, #7297, #19663, #38787, #4432, #16750, #29332, #1151, #13685, #35721, #23944, #14882, #17761, #30553, #33237, #30967, #37120, #21492, #8290, #14474 ),
 .UNSPECIFIED., .F., .F.,
 ( 4, 2, 2, 2, 2, 2, 2, 2, 2, 2, 4 ),
 ( 0.000000000000000000, 0.2499999999999973910, 0.3749999999999961142, 0.4999999999999947820, 0.5624999999999912292, 0.5937499999999934497, 0.6249999999999956701, 0.6874999999999942268, 0.7187499999999961142, 0.7499999999999980016, 1.000000000000000000 ),
 .UNSPECIFIED. ) ;
#10463 = DIRECTION ( 'NONE',  ( 1.000000000000000000, 0.000000000000000000, 0.000000000000000000 ) ) ;
#10462 = CARTESIAN_POINT ( 'NONE',  ( 4.546924931960046656, -31.42929550842064756, 7.013842709614101167 ) ) ;
#10464 = CARTESIAN_POINT ( 'NONE',  ( -1.242570340174825594, -27.67546881208082965, 7.013842709614101167 ) ) ;
#10465 = CARTESIAN_POINT ( 'NONE',  ( 71.03485184658521234, 59.25305893485334963, 3.963404584535439312 ) ) ;
#10466 = CARTESIAN_POINT ( 'NONE',  ( 24.53703648633796774, 2.972983101647284521, -3.608924253653490233 ) ) ;
#10467 = VERTEX_POINT ( 'NONE', #17059 ) ;
#10468 = CARTESIAN_POINT ( 'NONE',  ( -71.43161014973536282, 0.09092285538556041380, 5.980075040747969695 ) ) ;
#10469 = ORIENTED_EDGE ( 'NONE', *, *, #32509, .F. ) ;
#10470 = AXIS2_PLACEMENT_3D ( 'NONE', #32233, #7897, #23941 ) ;
#10471 = CARTESIAN_POINT ( 'NONE',  ( 21.85643539959776760, -1.193669045901033066, -12.68912657263372346 ) ) ;
#10472 = CARTESIAN_POINT ( 'NONE',  ( 21.46948114135319230, 9.243557392228170855, -3.873122283670241917 ) ) ;
#10473 = CARTESIAN_POINT ( 'NONE',  ( 0.3425108556361675105, -32.68700637368826989, 6.959317978105162616 ) ) ;
#10474 = CARTESIAN_POINT ( 'NONE',  ( 81.44087877708247447, 61.54565157041406565, 1.662073781717998022 ) ) ;
#10475 = CARTESIAN_POINT ( 'NONE',  ( 87.14484084030976874, 0.3304612005822565313, -5.669005978848654870 ) ) ;
#10476 = CARTESIAN_POINT ( 'NONE',  ( 16.74878488105810348, 0.9046941363780687251, 4.803740791053210835 ) ) ;
#10477 = ORIENTED_EDGE ( 'NONE', *, *, #17912, .F. ) ;
#10478 = CARTESIAN_POINT ( 'NONE',  ( 4.221612433196463066, -25.23005020686840183, 7.635761828346577573 ) ) ;
#10479 = CARTESIAN_POINT ( 'NONE',  ( 5.076948709542616456, -29.17136787882120785, 6.903372536218456368 ) ) ;
#10480 = VECTOR ( 'NONE', #21013, 1000.000000000000000 ) ;
#10481 = CARTESIAN_POINT ( 'NONE',  ( 14.59423631969371193, -5.048651580101616965, -2.484181559264142081 ) ) ;
#10482 = CARTESIAN_POINT ( 'NONE',  ( 37.04352256721959691, -2.892790444795046323, -5.987935616230180891 ) ) ;
#10483 = CARTESIAN_POINT ( 'NONE',  ( 1.700390093233090871, -29.56993018339339940, 6.800000000000000711 ) ) ;
#10484 = CARTESIAN_POINT ( 'NONE',  ( 84.12549522848908623, 2.987061070915658867, -0.8566216743701494662 ) ) ;
#10485 = CARTESIAN_POINT ( 'NONE',  ( -70.92837670882107659, 28.72470171467712063, 0.000000000000000000 ) ) ;
#10486 = CARTESIAN_POINT ( 'NONE',  ( 1.667813721708216956, -26.16298220691985676, 7.257242401810563237 ) ) ;
#10487 = DIRECTION ( 'NONE',  ( 1.000000000000000000, 0.000000000000000000, 0.000000000000000000 ) ) ;
#10488 = CARTESIAN_POINT ( 'NONE',  ( 28.70277213621809409, -3.561666039817526386, 4.654175941992544807 ) ) ;
#10489 = EDGE_LOOP ( 'NONE', ( #25045, #22038, #32154, #8053, #35989 ) ) ;
#10490 = EDGE_LOOP ( 'NONE', ( #25919, #10949, #14956, #21678 ) ) ;
#10491 = CARTESIAN_POINT ( 'NONE',  ( 37.17617793620765809, -2.565058875548333894, 5.981048444294359001 ) ) ;
#10492 = CARTESIAN_POINT ( 'NONE',  ( -4.224659823956008253, -51.67615071827237472, -2.500000000000000000 ) ) ;
#10493 = CARTESIAN_POINT ( 'NONE',  ( 66.27376694609004915, 57.73522568913436004, -4.000000000000000000 ) ) ;
#10494 = CARTESIAN_POINT ( 'NONE',  ( 86.93061992748306466, -1.256218166249259749, 5.071404822462298512 ) ) ;
#10495 = TOROIDAL_SURFACE ( 'NONE', #23011, 6.999999999999986677, 1.000000000000000000 ) ;
#10496 = ORIENTED_EDGE ( 'NONE', *, *, #7945, .T. ) ;
#10497 = CARTESIAN_POINT ( 'NONE',  ( 5.140927780591328933, -28.92751227575017481, 7.710604733652626663 ) ) ;
#10498 = CARTESIAN_POINT ( 'NONE',  ( -77.95330471031414277, 33.71485196875532608, 8.800414904976364028 ) ) ;
#10499 =( NAMED_UNIT ( * ) SI_UNIT ( $, .STERADIAN. ) SOLID_ANGLE_UNIT ( ) );
#10500 = ORIENTED_EDGE ( 'NONE', *, *, #17745, .T. ) ;
#10501 = FACE_OUTER_BOUND ( 'NONE', #6397, .T. ) ;
#10502 = SURFACE_SIDE_STYLE ('',( #22283 ) ) ;
#10503 = ORIENTED_EDGE ( 'NONE', *, *, #17306, .T. ) ;
#10504 = CARTESIAN_POINT ( 'NONE',  ( 23.64899080490409489, 3.263760929269430289, 3.660893560480292575 ) ) ;
#10505 = CARTESIAN_POINT ( 'NONE',  ( 78.69012442119819184, 66.05840891509440382, -1.017094602978585449 ) ) ;
#10506 = AXIS2_PLACEMENT_3D ( 'NONE', #6908, #25241, #38379 ) ;
#10508 = EDGE_CURVE ( 'NONE', #23344, #6217, #21771, .T. ) ;
#10507 = PLANE ( 'NONE',  #11417 ) ;
#10509 = EDGE_LOOP ( 'NONE', ( #12970, #28515, #2346, #36434, #33038 ) ) ;
#10510 = CARTESIAN_POINT ( 'NONE',  ( 75.72894860151858154, 61.00966332974834927, -3.846775394605490561 ) ) ;
#10512 = CARTESIAN_POINT ( 'NONE',  ( 4.427633003249534127, -27.39263707270477965, 7.780491323090173772 ) ) ;
#10511 = DIRECTION ( 'NONE',  ( 0.8888117386314211554, 0.4582725098355677762, 0.000000000000000000 ) ) ;
#10513 = FACE_OUTER_BOUND ( 'NONE', #20478, .T. ) ;
#10514 = CARTESIAN_POINT ( 'NONE',  ( 76.72366484839766088, 61.84716987400887689, 3.872369636032537699 ) ) ;
#10515 = ORIENTED_EDGE ( 'NONE', *, *, #8161, .T. ) ;
#10516 = DIRECTION ( 'NONE',  ( 1.000000000000000000, 0.000000000000000000, 0.000000000000000000 ) ) ;
#10517 = CARTESIAN_POINT ( 'NONE',  ( 1.709223551401949148, -26.07549619481818581, 7.773839561854632763 ) ) ;
#10518 = CARTESIAN_POINT ( 'NONE',  ( 23.94313517838655869, 2.810339304371657132, -3.943303330136482820 ) ) ;
#10519 = CARTESIAN_POINT ( 'NONE',  ( 0.1825688514500733994, -0.6000000000000004219, 3.931742364882332197 ) ) ;
#10520 = CARTESIAN_POINT ( 'NONE',  ( 82.15586074033954844, 62.44414535927739962, 1.848245342697198756 ) ) ;
#10521 = B_SPLINE_CURVE_WITH_KNOTS ( 'NONE', 3,
 ( #12291, #370, #24653, #31050, #5925, #9200, #28144, #21780, #18666, #3074, #32668, #3675, #19499, #34965, #32463, #31857, #29365, #32072, #10421, #1382, #575, #20091, #4469, #10612, #22997, #22595, #38415, #6740, #23188, #28967, #35562, #4261, #35757 ),
 .UNSPECIFIED., .F., .F.,
 ( 4, 2, 2, 2, 2, 2, 2, 2, 2, 2, 2, 1, 2, 2, 1, 1, 2, 4 ),
 ( 0.4585963849156251548, 0.4882313195419025753, 0.5030487868550412855, 0.5178662541681799958, 0.5771361234207347257, 0.6067710580470121462, 0.6215885253601507454, 0.6364059926732894557, 0.6956758619258440746, 0.7253107965521212730, 0.7401282638652599832, 0.7475369975218293384, 0.7493891809359716216, 0.7503152726430426522, 0.7512413643501137939, 0.7549457311783988045, 0.8142156004309570871, 0.9327553389360742075 ),
 .UNSPECIFIED. ) ;
#10522 = CARTESIAN_POINT ( 'NONE',  ( -0.08946644513347716543, -32.57766927571074689, 6.880608371227948439 ) ) ;
#10523 = CARTESIAN_POINT ( 'NONE',  ( 30.73735125564872916, -2.095387222228427770, 5.934458408524426076 ) ) ;
#10524 = CARTESIAN_POINT ( 'NONE',  ( 2.266461764120263123, -26.21737921967696039, 7.740055089680400791 ) ) ;
#10525 = CARTESIAN_POINT ( 'NONE',  ( 3.560683935411703693, -26.72399628134570904, 6.895222827070020877 ) ) ;
#10526 = CARTESIAN_POINT ( 'NONE',  ( 11.65737507970504439, -27.06993018339339940, 6.000000000000000000 ) ) ;
#10527 = CARTESIAN_POINT ( 'NONE',  ( -0.5557083577496700899, -32.11357244989347492, 6.866852738645443210 ) ) ;
#10528 = CARTESIAN_POINT ( 'NONE',  ( -1.600658481268679267, -28.40671124064021669, 7.695279973900954751 ) ) ;
#10529 = CARTESIAN_POINT ( 'NONE',  ( 34.76593155650069633, -3.465238236085922185, -5.619570445338033515 ) ) ;
#10530 = CARTESIAN_POINT ( 'NONE',  ( 1.145429890469515932, -32.92433313672930240, 7.703977250142847844 ) ) ;
#10531 = DIRECTION ( 'NONE',  ( 0.000000000000000000, 0.000000000000000000, 1.000000000000000000 ) ) ;
#10532 = CARTESIAN_POINT ( 'NONE',  ( -2.340808619595282636, -26.33796619817592699, 7.754798119455333705 ) ) ;
#10533 = CARTESIAN_POINT ( 'NONE',  ( -1.574103479719520360, -28.35884934600536056, 7.778495531946295394 ) ) ;
#10534 = EDGE_CURVE ( 'NONE', #29043, #28218, #17801, .T. ) ;
#10535 = CARTESIAN_POINT ( 'NONE',  ( 21.88744680497111261, -13.17188653508849150, -2.500000000000000888 ) ) ;
#10536 = CIRCLE ( 'NONE', #33579, 0.1000000000000028644 ) ;
#10537 = CARTESIAN_POINT ( 'NONE',  ( 30.19003827612802482, -2.952522945788203845, 4.918283640461378781 ) ) ;
#10538 = VERTEX_POINT ( 'NONE', #29637 ) ;
#10539 = CARTESIAN_POINT ( 'NONE',  ( 36.92447304359136240, -2.367222292930631689, 5.951667485741300112 ) ) ;
#10540 = DIRECTION ( 'NONE',  ( 0.3754033771448285206, 0.6502177225477927536, 0.6605219282605379050 ) ) ;
#10541 = CARTESIAN_POINT ( 'NONE',  ( 67.22540103859083160, 57.85622601175691671, -3.990981480864019826 ) ) ;
#10542 = CARTESIAN_POINT ( 'NONE',  ( 3.075261667515430286, -26.35127567747291977, 6.971170733404098208 ) ) ;
#10543 = ADVANCED_FACE ( 'NONE', ( #26754 ), #20358, .T. ) ;
#10544 = ORIENTED_EDGE ( 'NONE', *, *, #6630, .T. ) ;
#10545 = PLANE ( 'NONE',  #17325 ) ;
#10546 = CARTESIAN_POINT ( 'NONE',  ( 30.76799283776897198, -3.322052511316047951, 4.963599853823706276 ) ) ;
#10547 = CARTESIAN_POINT ( 'NONE',  ( 85.09607640761747405, 1.741501683616388130, -5.098621195172435172 ) ) ;
#10548 = LINE ( 'NONE', #13442, #5098 ) ;
#10549 = CARTESIAN_POINT ( 'NONE',  ( -1.461482890078116936, -28.31986800979595031, 6.866852738645442322 ) ) ;
#10550 = CARTESIAN_POINT ( 'NONE',  ( 3.612054795167425336, -26.63811301223460859, 6.931070083220558509 ) ) ;
#10551 = DIRECTION ( 'NONE',  ( 0.000000000000000000, 0.000000000000000000, -1.000000000000000000 ) ) ;
#10552 = ORIENTED_EDGE ( 'NONE', *, *, #39830, .T. ) ;
#10553 = CARTESIAN_POINT ( 'NONE',  ( 22.61513645261399219, 4.622024906660042731, 3.046565464745161655 ) ) ;
#10554 = AXIS2_PLACEMENT_3D ( 'NONE', #22058, #34633, #9691 ) ;
#10555 = CARTESIAN_POINT ( 'NONE',  ( -1.740011302788441627, -30.21307731605675073, 7.697032948437509070 ) ) ;
#10556 = CARTESIAN_POINT ( 'NONE',  ( 81.28814307398172900, 61.80674180605062418, 2.393593008231199804 ) ) ;
#10557 = EDGE_CURVE ( 'NONE', #24741, #27839, #7807, .T. ) ;
#10559 = EDGE_CURVE ( 'NONE', #13946, #8281, #17161, .T. ) ;
#10558 = CARTESIAN_POINT ( 'NONE',  ( -63.70768058868311812, 44.39675795731061214, 1.212206658320163166 ) ) ;
#10560 = ORIENTED_EDGE ( 'NONE', *, *, #11698, .F. ) ;
#10561 = CARTESIAN_POINT ( 'NONE',  ( 79.99044059672593221, 61.67469478680249040, -3.091829831932956019 ) ) ;
#10562 =( BOUNDED_SURFACE ( )  B_SPLINE_SURFACE ( 3, 2, ( 
 ( #19094, #3283, #11313 ),
 ( #36655, #40145, #21218 ),
 ( #20798, #37813, #23879 ),
 ( #5164, #8434, #2093 ),
 ( #37056, #9617, #21015 ),
 ( #33789, #36453, #24297 ) ),
 .UNSPECIFIED., .F., .F., .T. ) 
 B_SPLINE_SURFACE_WITH_KNOTS ( ( 4, 2, 4 ),
 ( 3, 3 ),
 ( 4.712388980384689674, 5.164939930480247909, 5.617490880575807033 ),
 ( 0.000000000000000000, 1.000000000000000000 ),
 .UNSPECIFIED. ) 
 GEOMETRIC_REPRESENTATION_ITEM ( )  RATIONAL_B_SPLINE_SURFACE ( (
 ( 1.000000000000000000, 0.7071067811865475727, 1.000000000000000000),
 ( 1.000000000000000000, 0.6870851634080177295, 1.000000000000000000),
 ( 1.000000000000000000, 0.6661308060340611625, 1.000000000000000000),
 ( 1.000000000000000000, 0.6267038978092043244, 1.000000000000000000),
 ( 1.000000000000000000, 0.6082500109239441510, 1.000000000000000000),
 ( 1.000000000000000000, 0.5935057080259639184, 1.000000000000000000) ) ) 
 REPRESENTATION_ITEM ( '' )  SURFACE ( )  );
#10564 = CARTESIAN_POINT ( 'NONE',  ( -1.707873693682673055, -28.77385357979384040, 6.956915634232264445 ) ) ;
#10563 = CARTESIAN_POINT ( 'NONE',  ( 21.73476950717714118, 0.2476036213341410441, 9.023233531077035963 ) ) ;
#10565 = CARTESIAN_POINT ( 'NONE',  ( 79.04416262434902762, 66.14279969385735569, -1.662073781712726017 ) ) ;
#10566 = CARTESIAN_POINT ( 'NONE',  ( 79.22522514097650514, 63.97890519848278501, 3.707164540951486398 ) ) ;
#10567 = DIRECTION ( 'NONE',  ( -0.9980241895169804645, 0.000000000000000000, 0.06283086135788849835 ) ) ;
#10568 = VECTOR ( 'NONE', #27239, 1000.000000000000000 ) ;
#10569 = CARTESIAN_POINT ( 'NONE',  ( 79.33847868486732580, 66.30689617902915245, 1.090531591958330937 ) ) ;
#10571 = ORIENTED_EDGE ( 'NONE', *, *, #24100, .T. ) ;
#10570 = LINE ( 'NONE', #16944, #26860 ) ;
#10572 = CARTESIAN_POINT ( 'NONE',  ( 25.32326662574907772, -3.445015843796760624, -4.932833089913290614 ) ) ;
#10573 = FACE_OUTER_BOUND ( 'NONE', #11911, .T. ) ;
#10574 = ORIENTED_EDGE ( 'NONE', *, *, #32833, .F. ) ;
#10575 = CARTESIAN_POINT ( 'NONE',  ( -76.43910119853934759, -5.761394667964060190, 8.352738067394287924 ) ) ;
#10576 = CARTESIAN_POINT ( 'NONE',  ( 0.6636879034114320230, -26.22699007480350986, 7.013842709614101167 ) ) ;
#10577 = EDGE_CURVE ( 'NONE', #9234, #25156, #7303, .T. ) ;
#10578 = CARTESIAN_POINT ( 'NONE',  ( -0.06814292006501697363, -32.57731014431580263, 7.781480525794714609 ) ) ;
#10579 = VERTEX_POINT ( 'NONE', #23653 ) ;
#10580 = CARTESIAN_POINT ( 'NONE',  ( -1.002278781269885899, -31.77069333300380194, 7.785344483711591934 ) ) ;
#10581 = CARTESIAN_POINT ( 'NONE',  ( 25.73398621336427539, 2.637371603049242896, -3.518938631727759336 ) ) ;
#10582 = CARTESIAN_POINT ( 'NONE',  ( 30.24787234978726858, -2.991825711127265919, -4.927310046378262420 ) ) ;
#10583 = DIRECTION ( 'NONE',  ( 1.000000000000000000, -0.000000000000000000, 0.000000000000000000 ) ) ;
#10584 = CARTESIAN_POINT ( 'NONE',  ( -1.021571885336638674, -31.77015830299410837, 6.870737987065011154 ) ) ;
#10585 = CARTESIAN_POINT ( 'NONE',  ( 5.199955032719538295, -29.62511382514724545, 6.875671892026065990 ) ) ;
#10586 = AXIS2_PLACEMENT_3D ( 'NONE', #5008, #30538, #17539 ) ;
#10587 = FACE_OUTER_BOUND ( 'NONE', #26046, .T. ) ;
#10588 = CARTESIAN_POINT ( 'NONE',  ( 4.318185990598753854, -31.87765716460728882, 7.780491323090173772 ) ) ;
#10589 = ORIENTED_EDGE ( 'NONE', *, *, #16233, .T. ) ;
#10590 = EDGE_CURVE ( 'NONE', #1177, #34207, #26243, .T. ) ;
#10592 = ADVANCED_FACE ( 'NONE', ( #11844 ), #33914, .T. ) ;
#10591 = CARTESIAN_POINT ( 'NONE',  ( 66.69694663263604184, 57.94160696200565042, 3.999246569073970026 ) ) ;
#10593 = EDGE_CURVE ( 'NONE', #2020, #4342, #3409, .T. ) ;
#10594 = CARTESIAN_POINT ( 'NONE',  ( 87.24982552262115121, -1.326261458569501839, 4.881571762780114732 ) ) ;
#10595 = CIRCLE ( 'NONE', #1422, 7.744449365083023729 ) ;
#10596 = DIRECTION ( 'NONE',  ( -0.000000000000000000, -0.000000000000000000, 1.000000000000000000 ) ) ;
#10597 = VERTEX_POINT ( 'NONE', #25048 ) ;
#10598 = CARTESIAN_POINT ( 'NONE',  ( -80.67082329696982868, 10.50842065708840067, -5.186806082895198955 ) ) ;
#10599 = CYLINDRICAL_SURFACE ( 'NONE', #16589, 0.09010775117052739758 ) ;
#10600 = CARTESIAN_POINT ( 'NONE',  ( 1.080526075423322796, -26.12525383235529119, 7.756742906098588186 ) ) ;
#10601 = VERTEX_POINT ( 'NONE', #40455 ) ;
#10602 = DIRECTION ( 'NONE',  ( 0.000000000000000000, 0.000000000000000000, 1.000000000000000000 ) ) ;
#10603 = ORIENTED_EDGE ( 'NONE', *, *, #26458, .F. ) ;
#10604 = CARTESIAN_POINT ( 'NONE',  ( 78.87241222613832292, 65.34207468649371719, -2.902290250791178305 ) ) ;
#10605 = EDGE_CURVE ( 'NONE', #31392, #486, #30617, .T. ) ;
#10606 = CARTESIAN_POINT ( 'NONE',  ( 33.89725028478159174, -5.465908938576614418, 0.4877600842561391481 ) ) ;
#10607 = CARTESIAN_POINT ( 'NONE',  ( 80.51397140397814667, 62.59311809350369060, 3.432573985763616164 ) ) ;
#10608 = DIRECTION ( 'NONE',  ( -0.000000000000000000, -0.000000000000000000, 1.000000000000000000 ) ) ;
#10609 = CARTESIAN_POINT ( 'NONE',  ( 24.38340127123625578, 2.573202976557773525, 4.012017501801370400 ) ) ;
#10610 = CARTESIAN_POINT ( 'NONE',  ( 20.34585743190884344, 6.625446340279268043, -3.270942662530205602 ) ) ;
#10611 = DIRECTION ( 'NONE',  ( -0.3754033771448376799, 0.6502177225477876465, 0.6605219282605379050 ) ) ;
#10612 = CARTESIAN_POINT ( 'NONE',  ( 33.78877019722047947, -4.859422714393206277, -3.437826128937246484 ) ) ;
#10613 = CARTESIAN_POINT ( 'NONE',  ( -70.92837670882201451, -21.78299143689573469, 6.000000000001379341 ) ) ;
#10614 = CARTESIAN_POINT ( 'NONE',  ( 78.42694857803141417, 65.87163300571076263, -1.555883980134156186 ) ) ;
#10615 = ADVANCED_FACE ( 'NONE', ( #31226 ), #40063, .F. ) ;
#10616 = CARTESIAN_POINT ( 'NONE',  ( -1.774306543252402557, -29.99004581285702997, 6.931070083220559397 ) ) ;
#10617 = FACE_OUTER_BOUND ( 'NONE', #11928, .T. ) ;
#10618 = CIRCLE ( 'NONE', #40222, 6.329987104167475565 ) ;
#10619 = CARTESIAN_POINT ( 'NONE',  ( -75.92415766659136978, -3.925048772356933835, -10.09882139952678948 ) ) ;
#10620 = LINE ( 'NONE', #10429, #8988 ) ;
#10621 = CARTESIAN_POINT ( 'NONE',  ( 2.242723711017451382, -32.92639770848892766, 6.894806418505347700 ) ) ;
#10622 = CARTESIAN_POINT ( 'NONE',  ( 81.23980251882781545, 61.36242252098747940, 1.459100623883065717 ) ) ;
#10623 = CARTESIAN_POINT ( 'NONE',  ( -1.482541337455568931, -30.76531870494248366, 7.712764235869104645 ) ) ;
#10624 = CARTESIAN_POINT ( 'NONE',  ( 3.953870441647290956, -27.02398707340232420, 7.778050822775634643 ) ) ;
#10625 = CARTESIAN_POINT ( 'NONE',  ( -1.314054584179517704, -27.80863854348385189, 7.778495531946295394 ) ) ;
#10626 = CARTESIAN_POINT ( 'NONE',  ( -1.642039206111510108, -30.19297164693361424, 7.670860738520328681 ) ) ;
#10627 = EDGE_CURVE ( 'NONE', #3011, #5958, #18640, .T. ) ;
#10628 = ORIENTED_EDGE ( 'NONE', *, *, #30089, .F. ) ;
#10629 = CARTESIAN_POINT ( 'NONE',  ( 4.500391056462942352, -27.46992940240218672, 6.971170733404105313 ) ) ;
#10630 = EDGE_CURVE ( 'NONE', #40685, #34893, #24783, .T. ) ;
#10631 = CARTESIAN_POINT ( 'NONE',  ( 22.01541346579904967, 4.834729283906541220, -3.642368534677343117 ) ) ;
#10632 = CARTESIAN_POINT ( 'NONE',  ( 4.883321523921757112, -28.37454166184433646, 7.712764235869103757 ) ) ;
#10633 = CARTESIAN_POINT ( 'NONE',  ( -0.9907592352440830474, -27.33213670732227030, 7.638132480492513920 ) ) ;
#10634 = DIRECTION ( 'NONE',  ( 0.000000000000000000, 0.000000000000000000, 1.000000000000000000 ) ) ;
#10635 = CARTESIAN_POINT ( 'NONE',  ( 68.61500287773905882, 58.59333675578601230, 3.993768376023893563 ) ) ;
#10636 = CARTESIAN_POINT ( 'NONE',  ( 35.33522264782425282, -3.171501239445705167, 5.721314098418827321 ) ) ;
#10637 = EDGE_CURVE ( 'NONE', #38489, #36027, #8275, .T. ) ;
#10638 = CARTESIAN_POINT ( 'NONE',  ( -64.08758708074093136, 42.98405160571059014, -2.320550953111519377 ) ) ;
#10639 = CARTESIAN_POINT ( 'NONE',  ( 84.84279093542515682, 3.008464274580536113, -1.251974654204536908 ) ) ;
#10641 = CARTESIAN_POINT ( 'NONE',  ( -0.3985195385088214359, -26.76911271758127597, 6.961115707816233567 ) ) ;
#10640 = CARTESIAN_POINT ( 'NONE',  ( 79.89688848262225918, 64.77169266163328132, -3.452358620554651036 ) ) ;
#10642 = CARTESIAN_POINT ( 'NONE',  ( -1.230621875064890069, -27.65703250815151648, 6.971170733404100872 ) ) ;
#10643 = CARTESIAN_POINT ( 'NONE',  ( -57.73493806181992483, 28.75062263012322106, 2.538950603207606349 ) ) ;
#10644 = EDGE_LOOP ( 'NONE', ( #19346, #19786, #12951, #19849, #13544 ) ) ;
#10645 = CARTESIAN_POINT ( 'NONE',  ( -80.30224715670834712, 11.50583414542592742, -3.508222272703448663 ) ) ;
#10646 = CARTESIAN_POINT ( 'NONE',  ( -17.07867591359219617, -26.64985754041175525, 6.800000000000000711 ) ) ;
#10647 = ORIENTED_EDGE ( 'NONE', *, *, #34625, .F. ) ;
#10648 = CARTESIAN_POINT ( 'NONE',  ( 3.594851464545667952, -26.62696974998548782, 7.013842709614101167 ) ) ;
#10649 = ORIENTED_EDGE ( 'NONE', *, *, #22930, .F. ) ;
#10650 = CARTESIAN_POINT ( 'NONE',  ( 80.39951605126471179, 63.19197404919984962, -3.632888195267880427 ) ) ;
#10651 = DIRECTION ( 'NONE',  ( -0.000000000000000000, -1.000000000000000000, -0.000000000000000000 ) ) ;
#10652 = CARTESIAN_POINT ( 'NONE',  ( 80.65725571609037559, 62.96675706018874052, 3.489836119548948901 ) ) ;
#10653 = CARTESIAN_POINT ( 'NONE',  ( 24.35217137059073522, 1.294611633738677270, 4.709786998218760345 ) ) ;
#10655 = ORIENTED_EDGE ( 'NONE', *, *, #16606, .T. ) ;
#10654 = AXIS2_PLACEMENT_3D ( 'NONE', #2525, #15050, #12375 ) ;
#10656 = DIRECTION ( 'NONE',  ( 1.000000000000000000, 1.776143608908745286E-15, 0.000000000000000000 ) ) ;
#10658 = CARTESIAN_POINT ( 'NONE',  ( -34.97867591359219830, -24.55319635012989110, 6.700000000000000178 ) ) ;
#10657 = CARTESIAN_POINT ( 'NONE',  ( -58.83360130232286878, 28.75651630857863950, -5.941118172103339035 ) ) ;
#10659 = CARTESIAN_POINT ( 'NONE',  ( 4.178779287455901326, -33.93453988814196975, 7.695279973900954751 ) ) ;
#10660 = CARTESIAN_POINT ( 'NONE',  ( -64.08758708074093136, 42.86724024435063285, -2.417504070309356212 ) ) ;
#10661 = CARTESIAN_POINT ( 'NONE',  ( 4.390205000165592786, -31.80932647847912875, 7.635761828346570468 ) ) ;
#10662 = CARTESIAN_POINT ( 'NONE',  ( 21.81164502259897731, 5.201711882885422078, -3.655446855725318134 ) ) ;
#10663 = ORIENTED_EDGE ( 'NONE', *, *, #18494, .F. ) ;
#10664 = CARTESIAN_POINT ( 'NONE',  ( 5.140201863657823722, -30.18543153557743608, 7.773839561854630986 ) ) ;
#10665 = EDGE_CURVE ( 'NONE', #39112, #12351, #39492, .T. ) ;
#10666 = CARTESIAN_POINT ( 'NONE',  ( 22.36058758039612471, 3.933412737179332375, -7.046732538784932665 ) ) ;
#10667 = CARTESIAN_POINT ( 'NONE',  ( 21.88165365390326400, 4.350072964282386323, 2.563907282946755012E-12 ) ) ;
#10668 = CARTESIAN_POINT ( 'NONE',  ( 16.08591480223022074, 7.879342699536265648, 3.484773800359155960 ) ) ;
#10669 = CARTESIAN_POINT ( 'NONE',  ( 0.3625495304258689044, -32.69566459030958328, 6.895222827070020877 ) ) ;
#10670 = CARTESIAN_POINT ( 'NONE',  ( 81.69067057340667759, 62.21317191937867364, 2.410848004515911303 ) ) ;
#10671 = CARTESIAN_POINT ( 'NONE',  ( 86.69901843299427924, 0.4902165918510832388, 5.965927736749048194 ) ) ;
#10672 = B_SPLINE_CURVE_WITH_KNOTS ( 'NONE', 3,
 ( #37693, #31549, #34448, #18357, #6430, #18988, #22084, #15888, #25368, #9712, #22291, #15274, #40184, #11966, #24541, #8885, #12182, #21467, #6022 ),
 .UNSPECIFIED., .F., .F.,
 ( 4, 3, 3, 3, 3, 3, 4 ),
 ( 0.000000000000000000, 2.546128104244794248E-05, 5.711050680484199682E-05, 8.113074941676081634E-05, 0.0001053129305727044219, 0.0001360598016347131791, 0.0001612931755713729670 ),
 .UNSPECIFIED. ) ;
#10673 = CARTESIAN_POINT ( 'NONE',  ( -1.553683706606911130, -30.55532538593644176, 7.013842709614101167 ) ) ;
#10674 = EDGE_LOOP ( 'NONE', ( #5107, #10895, #7681, #37030 ) ) ;
#10675 = CARTESIAN_POINT ( 'NONE',  ( -81.60021392995659539, -5.622709797487786432, 2.348518091125527008 ) ) ;
#10676 = DIRECTION ( 'NONE',  ( -0.1303762246624283472, 0.7394003126383926761, 0.6605219282605379050 ) ) ;
#10677 = CARTESIAN_POINT ( 'NONE',  ( -70.92837670882107659, 13.87661300689599742, 10.00000000000000533 ) ) ;
#10678 = CARTESIAN_POINT ( 'NONE',  ( 18.20696997742687984, -2.825060525577835602, -3.048036020847092242 ) ) ;
#10679 = CARTESIAN_POINT ( 'NONE',  ( 27.40537536757053161, 0.9587627913666219026, -4.483669646254042185 ) ) ;
#10680 = PLANE ( 'NONE',  #34579 ) ;
#10681 = CARTESIAN_POINT ( 'NONE',  ( 84.47786603692917140, 2.553026049322892455, -3.367302602819985058 ) ) ;
#10682 = CARTESIAN_POINT ( 'NONE',  ( 28.66920249112477848, -4.024975064351027143, -4.110187144531254333 ) ) ;
#10683 = CIRCLE ( 'NONE', #845, 4.075022672948151126 ) ;
#10684 = EDGE_CURVE ( 'NONE', #21155, #9806, #10034, .T. ) ;
#10685 = ADVANCED_FACE ( 'NONE', ( #11364 ), #36909, .T. ) ;
#10686 = DIRECTION ( 'NONE',  ( 0.9637806624122927657, -0.2666961468790326473, 0.000000000000000000 ) ) ;
#10687 = ADVANCED_FACE ( 'NONE', ( #21269 ), #26083, .F. ) ;
#10688 = CARTESIAN_POINT ( 'NONE',  ( -1.139432846729372173, -27.70032573496690986, 6.997764925645182821 ) ) ;
#10689 = ORIENTED_EDGE ( 'NONE', *, *, #6051, .F. ) ;
#10690 = ORIENTED_EDGE ( 'NONE', *, *, #38245, .T. ) ;
#10691 = CARTESIAN_POINT ( 'NONE',  ( 33.11281012697673276, -0.1525902709989853945, 4.944059908066099851 ) ) ;
#10692 = CARTESIAN_POINT ( 'NONE',  ( 16.45184370577523225, -3.221501287979960715, 2.774106118266566945 ) ) ;
#10693 = CARTESIAN_POINT ( 'NONE',  ( -69.42837670882107659, -47.11702805680359063, 38.00000000000000711 ) ) ;
#10694 = CARTESIAN_POINT ( 'NONE',  ( 86.19214148621283300, -0.1009238796382747189, 5.955419684790980384 ) ) ;
#10695 = ORIENTED_EDGE ( 'NONE', *, *, #13113, .T. ) ;
#10696 = CARTESIAN_POINT ( 'NONE',  ( 3.423404917024849059, -32.61643964784510530, 6.894806418505347700 ) ) ;
#10697 = ORIENTED_EDGE ( 'NONE', *, *, #40626, .T. ) ;
#10698 = CARTESIAN_POINT ( 'NONE',  ( -58.56870219631065311, 27.89510117891458663, -3.538387446898162647 ) ) ;
#10699 = AXIS2_PLACEMENT_3D ( 'NONE', #33682, #8116, #20899 ) ;
#10700 = VERTEX_POINT ( 'NONE', #22998 ) ;
#10701 = CARTESIAN_POINT ( 'NONE',  ( 23.17633557675668143, 3.725374598916875168, 3.475392858078595104 ) ) ;
#10702 = CARTESIAN_POINT ( 'NONE',  ( 79.92383974732979368, 66.30194418458911798, -1.599335268229509888 ) ) ;
#10703 = CARTESIAN_POINT ( 'NONE',  ( 3.854318901935272379, -32.32856308795815892, 7.753200566781599079 ) ) ;
#10704 = ORIENTED_EDGE ( 'NONE', *, *, #2237, .T. ) ;
#10706 = CARTESIAN_POINT ( 'NONE',  ( 0.9267304714826871681, -32.98335233567298275, 7.013842709614101167 ) ) ;
#10705 = CARTESIAN_POINT ( 'NONE',  ( 2.496367219260529957, -26.16164236867905046, 6.965379264086542399 ) ) ;
#10707 = DIRECTION ( 'NONE',  ( -0.000000000000000000, 1.000000000000000000, -0.000000000000000000 ) ) ;
#10708 = CARTESIAN_POINT ( 'NONE',  ( 75.46848212330048966, 60.05767933327602037, 3.584990529380366997 ) ) ;
#10709 = AXIS2_PLACEMENT_3D ( 'NONE', #27463, #15722, #2785 ) ;
#10710 = CARTESIAN_POINT ( 'NONE',  ( 22.50620321255335554, 2.285223840635106640, -5.090854016693098671 ) ) ;
#10711 = CARTESIAN_POINT ( 'NONE',  ( -12.87867591359218977, -26.64985754041175525, 6.700000000000000178 ) ) ;
#10712 = CARTESIAN_POINT ( 'NONE',  ( 1.743740428028915268, -26.08457629419881485, 7.785096263473212375 ) ) ;
#10713 = CARTESIAN_POINT ( 'NONE',  ( 25.62569289649984583, 1.971242808189318296, -4.205907154860246244 ) ) ;
#10714 = CARTESIAN_POINT ( 'NONE',  ( 3.848298546108438245, -32.20554951821143419, 6.894806418505343260 ) ) ;
#10715 = DIRECTION ( 'NONE',  ( 0.000000000000000000, -0.000000000000000000, -1.000000000000000000 ) ) ;
#10716 = CARTESIAN_POINT ( 'NONE',  ( 80.64500926360319966, 65.89167229754917798, 2.340562087103263966 ) ) ;
#10717 = CARTESIAN_POINT ( 'NONE',  ( -0.2100398175957213787, -32.50254975568888938, 6.980586498568972509 ) ) ;
#10718 = CARTESIAN_POINT ( 'NONE',  ( 29.97449823033972649, -1.245471885678776980, 6.039028575696650414 ) ) ;
#10719 = DIRECTION ( 'NONE',  ( -0.000000000000000000, -0.000000000000000000, 1.000000000000000000 ) ) ;
#10720 = CARTESIAN_POINT ( 'NONE',  ( 25.51679268433478853, -4.687544639108172539, 0.4528783670679029094 ) ) ;
#10721 = DIRECTION ( 'NONE',  ( -0.000000000000000000, -0.000000000000000000, 1.000000000000000000 ) ) ;
#10722 = CARTESIAN_POINT ( 'NONE',  ( -0.5410438812439372080, -32.12650380312074816, 6.874555630061441214 ) ) ;
#10723 = VECTOR ( 'NONE', #18222, 1000.000000000000000 ) ;
#10724 = CARTESIAN_POINT ( 'NONE',  ( 0.1185081075117514898, -26.44780621764473949, 6.971170733404104425 ) ) ;
#10725 = CARTESIAN_POINT ( 'NONE',  ( 36.92999076337549269, -2.615982695873473762, -5.970216232463218198 ) ) ;
#10726 = DIRECTION ( 'NONE',  ( -0.1736481776669206722, -0.9848077530122096857, -0.000000000000000000 ) ) ;
#10727 = DIRECTION ( 'NONE',  ( 0.000000000000000000, 0.000000000000000000, 1.000000000000000000 ) ) ;
#10728 = CARTESIAN_POINT ( 'NONE',  ( -1.799566460562916470, -29.58736926422850999, 7.749999999999998224 ) ) ;
#10729 = DIRECTION ( 'NONE',  ( 1.000000000000000000, 0.000000000000000000, 0.000000000000000000 ) ) ;
#10730 = ADVANCED_FACE ( 'NONE', ( #17953 ), #20849, .F. ) ;
#10731 = FACE_OUTER_BOUND ( 'NONE', #28723, .T. ) ;
#10732 = EDGE_CURVE ( 'NONE', #30327, #38236, #30313, .T. ) ;
#10733 = ORIENTED_EDGE ( 'NONE', *, *, #15724, .F. ) ;
#10734 = CARTESIAN_POINT ( 'NONE',  ( 20.76538735788932399, 4.421521651906416217, 3.217090461606771701 ) ) ;
#10735 = B_SPLINE_CURVE_WITH_KNOTS ( 'NONE', 3,
 ( #27052, #39186, #32838, #39597, #39814, #11381, #20868, #5229, #23946, #4630, #11582, #33032, #17764, #13885 ),
 .UNSPECIFIED., .F., .F.,
 ( 4, 2, 2, 2, 2, 2, 4 ),
 ( 1.390486644391990834E-17, 0.0002943548652378657647, 0.0005887097304757176516, 0.0008830645957135694300, 0.001177419460951421425, 0.001766129191427110454, 0.002354838921902799483 ),
 .UNSPECIFIED. ) ;
#10736 = CARTESIAN_POINT ( 'NONE',  ( 1.212983646527633130, -26.10426722441512837, 7.754798119455333705 ) ) ;
#10737 = CARTESIAN_POINT ( 'NONE',  ( 67.54222599743037847, 57.89884484782556484, -3.985038673850038737 ) ) ;
#10738 = CARTESIAN_POINT ( 'NONE',  ( -1.348517286369408597, -27.85116208076715694, 7.686927408461905920 ) ) ;
#10739 = VERTEX_POINT ( 'NONE', #10613 ) ;
#10740 = LINE ( 'NONE', #22924, #23949 ) ;
#10741 = CARTESIAN_POINT ( 'NONE',  ( -4.248748702180636272, -26.64985754041175525, 6.800000000000000711 ) ) ;
#10742 = DIRECTION ( 'NONE',  ( 0.000000000000000000, 1.000000000000000000, 0.000000000000000000 ) ) ;
#10743 = DIRECTION ( 'NONE',  ( -0.000000000000000000, -0.000000000000000000, 1.000000000000000000 ) ) ;
#10744 = CARTESIAN_POINT ( 'NONE',  ( 0.07492370758569941169, -33.99638339305766266, 7.635761828346577573 ) ) ;
#10745 = CARTESIAN_POINT ( 'NONE',  ( 1.700390093233090871, -29.56993018339339940, 7.750000000000000888 ) ) ;
#10746 = ORIENTED_EDGE ( 'NONE', *, *, #19521, .F. ) ;
#10747 = CARTESIAN_POINT ( 'NONE',  ( 21.71285251252540505, 6.321249563836915719, 3.195723793048483863 ) ) ;
#10748 = FACE_OUTER_BOUND ( 'NONE', #5870, .T. ) ;
#10750 = CIRCLE ( 'NONE', #8124, 0.1000000000000028644 ) ;
#10749 = CARTESIAN_POINT ( 'NONE',  ( 81.19396390929411211, 61.77420168221061658, 2.442092683901115446 ) ) ;
#10751 = AXIS2_PLACEMENT_3D ( 'NONE', #22341, #35104, #13450 ) ;
#10752 = LINE ( 'NONE', #14451, #27834 ) ;
#10753 = ORIENTED_EDGE ( 'NONE', *, *, #3588, .F. ) ;
#10754 = CARTESIAN_POINT ( 'NONE',  ( 78.36941018910007983, 65.17477963226572513, -2.845586111146954700 ) ) ;
#10755 = CARTESIAN_POINT ( 'NONE',  ( 21.97782326148428211, 0.2280598603087039544, 7.713529440660342296 ) ) ;
#10756 = CARTESIAN_POINT ( 'NONE',  ( 80.57438652552279734, 65.15318659310567284, -3.125353918834855360 ) ) ;
#10757 = EDGE_CURVE ( 'NONE', #22478, #3797, #27018, .T. ) ;
#10758 = CARTESIAN_POINT ( 'NONE',  ( 78.24936850314311698, 65.65315377296109034, 2.033355767895868915 ) ) ;
#10759 = AXIS2_PLACEMENT_3D ( 'NONE', #19376, #14137, #26713 ) ;
#10760 = DIRECTION ( 'NONE',  ( -0.06282940500769126912, -0.006808616672654400036, -0.9980010564149641716 ) ) ;
#10761 = B_SPLINE_CURVE_WITH_KNOTS ( 'NONE', 3,
 ( #40330, #14597, #18303, #39518 ),
 .UNSPECIFIED., .F., .F.,
 ( 4, 4 ),
 ( 0.000000000000000000, 0.0008960438496711642777 ),
 .UNSPECIFIED. ) ;
#10762 = AXIS2_PLACEMENT_3D ( 'NONE', #10107, #25568, #10511 ) ;
#10763 = CARTESIAN_POINT ( 'NONE',  ( 82.34614708994683951, 62.54074552962158862, 1.204231967107850076 ) ) ;
#10765 = ORIENTED_EDGE ( 'NONE', *, *, #22386, .F. ) ;
#10764 = CARTESIAN_POINT ( 'NONE',  ( 5.121324086407808451, -24.55319635012989110, 6.700000000000000178 ) ) ;
#10766 = CARTESIAN_POINT ( 'NONE',  ( 30.07020345058763766, -4.232275913155626235, -2.900971327107725983 ) ) ;
#10767 = CARTESIAN_POINT ( 'NONE',  ( -64.38387608637881954, 34.70929407487278695, -5.501206404649174431 ) ) ;
#10768 = EDGE_LOOP ( 'NONE', ( #18484, #25661, #25565, #8171 ) ) ;
#10769 = CARTESIAN_POINT ( 'NONE',  ( -73.70040385515898151, -1.203501491044927763, 10.84085080396863532 ) ) ;
#10770 = CARTESIAN_POINT ( 'NONE',  ( 22.29883823987281843, 0.2632337822729923227, -7.099254618854787147 ) ) ;
#10771 = CARTESIAN_POINT ( 'NONE',  ( 6.073619586072577903, -32.40619529368077423, 6.894806418505347700 ) ) ;
#10772 = FACE_OUTER_BOUND ( 'NONE', #2757, .T. ) ;
#10773 = ORIENTED_EDGE ( 'NONE', *, *, #2122, .F. ) ;
#10774 = CARTESIAN_POINT ( 'NONE',  ( 23.38445862666371511, 3.558655165361555905, -3.098096260192995111 ) ) ;
#10775 = DIRECTION ( 'NONE',  ( -0.4999999999999999445, -0.8660254037844387076, 0.000000000000000000 ) ) ;
#10776 = DIRECTION ( 'NONE',  ( 0.6427876096865481337, -0.7660444431189706860, -0.000000000000000000 ) ) ;
#10777 = CARTESIAN_POINT ( 'NONE',  ( 5.125310579500037100, -30.29098473247341161, 6.865482280155368322 ) ) ;
#10778 = DIRECTION ( 'NONE',  ( 1.000000000000000000, 0.000000000000000000, 0.000000000000000000 ) ) ;
#10779 = CARTESIAN_POINT ( 'NONE',  ( 2.685785295776140114, -32.82400398323339630, 7.013842709614101167 ) ) ;
#10780 = DIRECTION ( 'NONE',  ( -1.000000000000000000, 0.000000000000000000, 0.000000000000000000 ) ) ;
#10781 = CYLINDRICAL_SURFACE ( 'NONE', #32937, 0.1000000000000028644 ) ;
#10782 = VECTOR ( 'NONE', #32766, 1000.000000000000227 ) ;
#10783 = AXIS2_PLACEMENT_3D ( 'NONE', #27233, #2353, #34059 ) ;
#10784 = EDGE_CURVE ( 'NONE', #6584, #22181, #5589, .T. ) ;
#10785 = ORIENTED_EDGE ( 'NONE', *, *, #36921, .T. ) ;
#10786 = CARTESIAN_POINT ( 'NONE',  ( 66.41209187282773030, 57.81891248311896447, 4.000000000000023093 ) ) ;
#10787 = CARTESIAN_POINT ( 'NONE',  ( 71.74426859761079811, 60.78783288850195987, -3.823636340558493885 ) ) ;
#10788 = AXIS2_PLACEMENT_3D ( 'NONE', #18796, #3194, #28682 ) ;
#10789 = CARTESIAN_POINT ( 'NONE',  ( 86.54029261786013194, -0.3196574014320466284, 5.877194713501632251 ) ) ;
#10790 =( BOUNDED_CURVE ( )  B_SPLINE_CURVE ( 3, ( #319, #12858, #16545, #23343 ),
 .UNSPECIFIED., .F., .T. ) 
 B_SPLINE_CURVE_WITH_KNOTS ( ( 4, 4 ),
 ( 1.381924640371168467, 1.574767692156076260 ),
 .UNSPECIFIED. ) 
 CURVE ( )  GEOMETRIC_REPRESENTATION_ITEM ( )  RATIONAL_B_SPLINE_CURVE ( ( 1.000000000000000000, 0.9969033633783033199, 0.9969033633783033199, 1.000000000000000000 ) ) 
 REPRESENTATION_ITEM ( '' )  );
#10791 = ORIENTED_EDGE ( 'NONE', *, *, #11089, .F. ) ;
#10792 = CARTESIAN_POINT ( 'NONE',  ( -73.56175482597444670, 5.777891328422431805, -10.86681767987946934 ) ) ;
#10793 = CARTESIAN_POINT ( 'NONE',  ( -1.699260392630454364, -29.52118006577551412, 6.894806418505346812 ) ) ;
#10794 = CARTESIAN_POINT ( 'NONE',  ( -6.348748702180634140, -25.49307895267003587, 6.700000000000000178 ) ) ;
#10795 = CARTESIAN_POINT ( 'NONE',  ( 5.095244238841699413, -29.75692037041947913, 7.013842709614101167 ) ) ;
#10796 = CARTESIAN_POINT ( 'NONE',  ( 25.27016851667936237, -3.231043682594727073, 4.010790585719321122 ) ) ;
#10797 = EDGE_LOOP ( 'NONE', ( #9190, #849, #32815, #27219 ) ) ;
#10798 = VERTEX_POINT ( 'NONE', #25377 ) ;
#10799 = CARTESIAN_POINT ( 'NONE',  ( 80.37564778476929916, 62.54931541869399325, -3.458772244351171476 ) ) ;
#10800 = CARTESIAN_POINT ( 'NONE',  ( -56.59682361629209879, 30.63869417066593925, 3.015094993620162978 ) ) ;
#10801 = CARTESIAN_POINT ( 'NONE',  ( 80.89520131247735435, 61.53942361443156983, 2.340042473998425354 ) ) ;
#10803 = ORIENTED_EDGE ( 'NONE', *, *, #23432, .T. ) ;
#10802 = CARTESIAN_POINT ( 'NONE',  ( 0.5050015716840180469, -26.38699875270473427, 7.712764235869104645 ) ) ;
#10804 = PRESENTATION_LAYER_ASSIGNMENT (  '', '', ( #30561 ) ) ;
#10805 = AXIS2_PLACEMENT_3D ( 'NONE', #34778, #38426, #32086 ) ;
#10806 = CARTESIAN_POINT ( 'NONE',  ( 1.700390093233090871, -29.56993018339339940, 7.800000000000000711 ) ) ;
#10807 = B_SPLINE_CURVE_WITH_KNOTS ( 'NONE', 3,
 ( #36762, #23787, #32877, #21128 ),
 .UNSPECIFIED., .F., .F.,
 ( 4, 4 ),
 ( 8.940560153363745023E-19, 6.391136169898180939E-06 ),
 .UNSPECIFIED. ) ;
#10808 = DIRECTION ( 'NONE',  ( 0.4690749385695657803, 0.8831583674551003460, 0.000000000000000000 ) ) ;
#10809 = DIRECTION ( 'NONE',  ( -0.8831583674551141128, 0.4690749385695399676, 0.000000000000000000 ) ) ;
#10810 = ADVANCED_FACE ( 'NONE', ( #9723 ), #18160, .F. ) ;
#10811 = CARTESIAN_POINT ( 'NONE',  ( 21.85643539959774273, -6.795129563591141064, 12.90182208710982259 ) ) ;
#10812 = DIRECTION ( 'NONE',  ( 0.3757233601570978965, 0.9267318687906764829, 0.000000000000000000 ) ) ;
#10813 = ORIENTED_EDGE ( 'NONE', *, *, #14119, .T. ) ;
#10814 = CARTESIAN_POINT ( 'NONE',  ( 5.200270010222271644, -29.54093765580782005, 7.730015791551948290 ) ) ;
#10815 = EDGE_CURVE ( 'NONE', #40423, #4923, #9260, .T. ) ;
#10816 = CIRCLE ( 'NONE', #33210, 6.000000000000002665 ) ;
#10817 = CARTESIAN_POINT ( 'NONE',  ( 14.62198803971679872, -4.616044494662263631, 2.500000000000223377 ) ) ;
#10818 = CARTESIAN_POINT ( 'NONE',  ( -72.84060385100936230, 2.621073588131995979, -10.96223601709252193 ) ) ;
#10819 = CARTESIAN_POINT ( 'NONE',  ( 4.713340623123058570, -27.78888299018493058, 7.695279973900954751 ) ) ;
#10820 = DIRECTION ( 'NONE',  ( -0.000000000000000000, -0.000000000000000000, 1.000000000000000000 ) ) ;
#10821 = CARTESIAN_POINT ( 'NONE',  ( 81.21493646480149664, 62.54560775605910550, 3.083955809406639048 ) ) ;
#10822 = CARTESIAN_POINT ( 'NONE',  ( -1.517981995599434475, -30.66637091792136260, 7.784476445165072533 ) ) ;
#10823 = DIRECTION ( 'NONE',  ( -0.000000000000000000, 1.000000000000000000, -0.000000000000000000 ) ) ;
#10824 = CARTESIAN_POINT ( 'NONE',  ( -9.078675913592196167, -26.64985754041175525, 6.800000000000000711 ) ) ;
#10825 = PLANE ( 'NONE',  #915 ) ;
#10826 = CARTESIAN_POINT ( 'NONE',  ( 4.454246376475485825, -27.40977380682100417, 6.865482280155369210 ) ) ;
#10827 = CARTESIAN_POINT ( 'NONE',  ( -0.3249999971511661756, -26.83903245017845407, 6.920489980334477487 ) ) ;
#10828 = CARTESIAN_POINT ( 'NONE',  ( 4.924932876884335009, -28.49181894775827928, 7.778050822775631090 ) ) ;
#10829 = CARTESIAN_POINT ( 'NONE',  ( 4.165454363429216933, -31.91160874139497494, 6.969307238440509700 ) ) ;
#10830 = EDGE_CURVE ( 'NONE', #13769, #25932, #2555, .T. ) ;
#10831 = LINE ( 'NONE', #23407, #5719 ) ;
#10832 = CARTESIAN_POINT ( 'NONE',  ( 69.43824574602471955, 58.18893279706789201, 3.907754234428237439 ) ) ;
#10833 = CARTESIAN_POINT ( 'NONE',  ( 36.63346434955200692, -3.080208230909283085, 5.923936114067666736 ) ) ;
#10834 = ORIENTED_EDGE ( 'NONE', *, *, #23032, .F. ) ;
#10835 = AXIS2_PLACEMENT_3D ( 'NONE', #30661, #10881, #17254 ) ;
#10836 = CARTESIAN_POINT ( 'NONE',  ( 4.234390967386161719, -31.83684322112676668, 7.768425012602597768 ) ) ;
#10837 = VECTOR ( 'NONE', #14633, 1000.000000000000000 ) ;
#10838 = CARTESIAN_POINT ( 'NONE',  ( 85.57721755140556752, 2.175474006149249018, 4.430974418963669059 ) ) ;
#10840 = CARTESIAN_POINT ( 'NONE',  ( -0.4112773674722806638, -26.77871049686494942, 6.903112506833885220 ) ) ;
#10839 = CARTESIAN_POINT ( 'NONE',  ( 80.61377670644299087, 63.65766204751285784, -3.614389211669656987 ) ) ;
#10841 = CIRCLE ( 'NONE', #36483, 6.681288188914807691 ) ;
#10842 = CARTESIAN_POINT ( 'NONE',  ( 5.190258803612193717, -29.91414858768555618, 7.501983001166816045 ) ) ;
#10843 = CARTESIAN_POINT ( 'NONE',  ( -58.83253814471410692, 27.61819298006738421, 3.984408728655188803 ) ) ;
#10844 = EDGE_LOOP ( 'NONE', ( #32749, #27822, #23135, #11352, #34022, #2626 ) ) ;
#10845 = DIRECTION ( 'NONE',  ( 0.000000000000000000, 1.000000000000000000, 0.000000000000000000 ) ) ;
#10846 = CIRCLE ( 'NONE', #33899, 0.1000000000000028644 ) ;
#10847 = VERTEX_POINT ( 'NONE', #6446 ) ;
#10848 = CARTESIAN_POINT ( 'NONE',  ( -1.722970638209900596, -28.84261588273779964, 7.754798119455333705 ) ) ;
#10849 = CARTESIAN_POINT ( 'NONE',  ( 78.66262733798787110, 65.98865143197190264, -1.634613895560575125 ) ) ;
#10850 = CARTESIAN_POINT ( 'NONE',  ( -18.24874870218063450, -26.64985754041175525, 6.700000000000000178 ) ) ;
#10851 = CARTESIAN_POINT ( 'NONE',  ( 78.75977295323087901, 65.93644120262132446, 1.938154327158139845 ) ) ;
#10852 = CARTESIAN_POINT ( 'NONE',  ( 23.99396089256777387, 1.018594166801584100, 4.989981842188739414 ) ) ;
#10853 = ORIENTED_EDGE ( 'NONE', *, *, #29445, .F. ) ;
#10854 = CARTESIAN_POINT ( 'NONE',  ( 5.029153757140225167, -30.26234874276111242, 6.864651958020304257 ) ) ;
#10856 = CARTESIAN_POINT ( 'NONE',  ( 5.401390093233090717, -29.58343279012807159, 7.635761828346577573 ) ) ;
#10855 = CARTESIAN_POINT ( 'NONE',  ( -56.59682361629209879, 30.63869417066593925, -3.015094993620159425 ) ) ;
#10857 = CARTESIAN_POINT ( 'NONE',  ( -1.260054023142102464, -27.89787437277597348, 7.721096864323902409 ) ) ;
#10858 = ADVANCED_FACE ( 'NONE', ( #18999 ), #5827, .F. ) ;
#10859 = DIRECTION ( 'NONE',  ( 0.9396926207859080948, 0.3420201433256694901, -0.000000000000000000 ) ) ;
#10860 = CARTESIAN_POINT ( 'NONE',  ( 23.99288918444596419, 3.298330898318068360, -3.389965429840589461 ) ) ;
#10861 = VERTEX_POINT ( 'NONE', #15078 ) ;
#10862 = CARTESIAN_POINT ( 'NONE',  ( 2.343537225896455745, -33.01033157941493101, 7.695279973900954751 ) ) ;
#10863 = EDGE_CURVE ( 'NONE', #7577, #38171, #27638, .T. ) ;
#10864 = ORIENTED_EDGE ( 'NONE', *, *, #25124, .T. ) ;
#10865 = AXIS2_PLACEMENT_3D ( 'NONE', #7987, #30234, #37013 ) ;
#10866 = CARTESIAN_POINT ( 'NONE',  ( 22.77977322753350720, -5.661609348961630594, -5.678499401198807917 ) ) ;
#10867 = PRODUCT_RELATED_PRODUCT_CATEGORY ( 'part', '', ( #11783 ) ) ;
#10868 = AXIS2_PLACEMENT_3D ( 'NONE', #33768, #15210, #2072 ) ;
#10869 = CARTESIAN_POINT ( 'NONE',  ( 16.91049418450527853, 9.757949552745497357, 2.499999999999927169 ) ) ;
#10870 = CARTESIAN_POINT ( 'NONE',  ( 1.109803157764845061, -33.01974279738480789, 7.750000000000000888 ) ) ;
#10871 = CARTESIAN_POINT ( 'NONE',  ( 79.82819440665414845, 65.73008711143909011, 2.710336141772892393 ) ) ;
#10872 = CARTESIAN_POINT ( 'NONE',  ( 85.55911739799610416, 1.969564878966352905, 4.951173091362058187 ) ) ;
#10873 = CARTESIAN_POINT ( 'NONE',  ( -0.5124352759832019322, -26.98857319813297551, 7.691066658568944447 ) ) ;
#10874 = ORIENTED_EDGE ( 'NONE', *, *, #11318, .T. ) ;
#10875 = ADVANCED_FACE ( 'NONE', ( #28459 ), #40195, .T. ) ;
#10876 = AXIS2_PLACEMENT_3D ( 'NONE', #5533, #29683, #26603 ) ;
#10877 = LINE ( 'NONE', #5476, #21705 ) ;
#10878 = CARTESIAN_POINT ( 'NONE',  ( 5.065225839463185942, -29.08208656869964415, 6.864651958020304257 ) ) ;
#10879 = CARTESIAN_POINT ( 'NONE',  ( -63.03213158086253287, 38.26878225442504800, 4.032857076801014351 ) ) ;
#10880 = CARTESIAN_POINT ( 'NONE',  ( 34.13636567165694657, -3.129955875004838628, -5.534203472820675707 ) ) ;
#10881 = DIRECTION ( 'NONE',  ( 0.000000000000000000, -0.000000000000000000, -1.000000000000000000 ) ) ;
#10882 = CARTESIAN_POINT ( 'NONE',  ( 84.29260032154424209, 2.783174668905456617, -2.501150759418095504 ) ) ;
#10883 = CARTESIAN_POINT ( 'NONE',  ( 30.23789859557072646, -3.686283672430305636, -4.621445095038371420 ) ) ;
#10884 = VERTEX_POINT ( 'NONE', #8893 ) ;
#10885 = DIRECTION ( 'NONE',  ( 0.000000000000000000, 0.000000000000000000, 1.000000000000000000 ) ) ;
#10886 = CARTESIAN_POINT ( 'NONE',  ( -68.98442902999595105, 21.93515443114010210, 8.800414904976364028 ) ) ;
#10887 = CARTESIAN_POINT ( 'NONE',  ( -1.185231845581470767, -27.77182395009346294, 6.864276522220859711 ) ) ;
#10888 = ORIENTED_EDGE ( 'NONE', *, *, #35911, .F. ) ;
#10889 = ORIENTED_EDGE ( 'NONE', *, *, #14799, .T. ) ;
#10890 = CARTESIAN_POINT ( 'NONE',  ( 29.48876346201022614, 1.220278706431014104, 4.220659031012087503 ) ) ;
#10891 = CARTESIAN_POINT ( 'NONE',  ( -1.601316894800309143, -30.73129909961408046, 6.887161170156907986 ) ) ;
#10892 = CARTESIAN_POINT ( 'NONE',  ( -62.96427906878926706, 37.71115934644217305, -4.137654479798320573 ) ) ;
#10893 = CARTESIAN_POINT ( 'NONE',  ( -75.45330471031414277, 33.71485196875532608, -46.17089178453873188 ) ) ;
#10894 = CIRCLE ( 'NONE', #32442, 0.1000000000000028644 ) ;
#10895 = ORIENTED_EDGE ( 'NONE', *, *, #10534, .F. ) ;
#10896 = CIRCLE ( 'NONE', #10232, 10.00000000000000888 ) ;
#10897 = CARTESIAN_POINT ( 'NONE',  ( 4.966384368437926078, -28.59977744957924628, 7.386948897581448570 ) ) ;
#10898 = VERTEX_POINT ( 'NONE', #15488 ) ;
#10899 = CARTESIAN_POINT ( 'NONE',  ( -69.92837670882107659, -0.7829914368874778541, 38.00000000000000711 ) ) ;
#10901 = CARTESIAN_POINT ( 'NONE',  ( 21.87278005295212324, 2.930088050433418800, 3.925081081565170660 ) ) ;
#10900 = CARTESIAN_POINT ( 'NONE',  ( 4.754320870746903793, -27.86007999067432195, 6.880608371227952880 ) ) ;
#10902 = ORIENTED_EDGE ( 'NONE', *, *, #38857, .T. ) ;
#10903 = EDGE_CURVE ( 'NONE', #15032, #21175, #15423, .T. ) ;
#10904 = CARTESIAN_POINT ( 'NONE',  ( 23.69208156265775145, 3.471075682706086685, 3.392352389993136264 ) ) ;
#10905 = CIRCLE ( 'NONE', #38504, 0.1000000000000028644 ) ;
#10906 = CARTESIAN_POINT ( 'NONE',  ( 82.47197227462035585, 63.49890707693131731, -1.793694987646316186 ) ) ;
#10907 = EDGE_CURVE ( 'NONE', #30228, #109, #31637, .T. ) ;
#10908 = CARTESIAN_POINT ( 'NONE',  ( 3.853256869806246154, -32.32948931917582769, 7.751599049952172749 ) ) ;
#10909 = VERTEX_POINT ( 'NONE', #6647 ) ;
#10911 = CARTESIAN_POINT ( 'NONE',  ( 14.77222818450456643, -4.461908109758233820, -2.511961494517393145 ) ) ;
#10910 = LINE ( 'NONE', #36443, #20637 ) ;
#10912 = CYLINDRICAL_SURFACE ( 'NONE', #27701, 0.1000000000000028644 ) ;
#10913 = CARTESIAN_POINT ( 'NONE',  ( 75.14412900705532650, 60.78131343986104440, 3.865308561588337799 ) ) ;
#10914 = CARTESIAN_POINT ( 'NONE',  ( 22.24968006774034990, 3.032303245382528711, -4.686988268442751071 ) ) ;
#10915 = DIRECTION ( 'NONE',  ( -0.000000000000000000, -0.000000000000000000, 1.000000000000000000 ) ) ;
#10916 = EDGE_CURVE ( 'NONE', #22571, #4144, #40178, .T. ) ;
#10917 = CARTESIAN_POINT ( 'NONE',  ( -0.5596933955661176352, -26.89747389307597203, 7.635761828346574909 ) ) ;
#10918 = EDGE_CURVE ( 'NONE', #2179, #17881, #34777, .T. ) ;
#10919 = CARTESIAN_POINT ( 'NONE',  ( 24.23747724132151760, 2.648570161240320964, -3.989242527747176137 ) ) ;
#10920 = CARTESIAN_POINT ( 'NONE',  ( -1.261630184736219684, -27.90066804241507015, 7.680992449362118002 ) ) ;
#10921 = FACE_OUTER_BOUND ( 'NONE', #430, .T. ) ;
#10922 = CARTESIAN_POINT ( 'NONE',  ( 81.60288604192470530, 64.55353989381950441, 2.864610283900509202 ) ) ;
#10923 = CARTESIAN_POINT ( 'NONE',  ( 85.70831578087668845, 2.086076349557777654, 3.711011680213312403 ) ) ;
#10924 = CARTESIAN_POINT ( 'NONE',  ( 31.80158048871438581, -1.669318041804891850, 6.009059823207920203 ) ) ;
#10925 = DIRECTION ( 'NONE',  ( 1.000000000000000000, 0.000000000000000000, -0.000000000000000000 ) ) ;
#10926 = LINE ( 'NONE', #23504, #25495 ) ;
#10927 = CARTESIAN_POINT ( 'NONE',  ( -81.77946201182784591, -5.605489059854700251, -1.058732183306707153 ) ) ;
#10928 = ORIENTED_EDGE ( 'NONE', *, *, #28275, .F. ) ;
#10929 = LINE ( 'NONE', #38527, #25051 ) ;
#10930 = CARTESIAN_POINT ( 'NONE',  ( 0.1171942947253034051, -26.44847140242086780, 6.931070083220560285 ) ) ;
#10931 = CARTESIAN_POINT ( 'NONE',  ( 36.64788811273031399, -3.154273958936592237, -5.926187291151666869 ) ) ;
#10932 = CARTESIAN_POINT ( 'NONE',  ( -55.15112219448760555, 31.23515184556838165, -9.800414904976365804 ) ) ;
#10933 = CARTESIAN_POINT ( 'NONE',  ( -1.699600969445970833, -29.57893194192095976, 7.630645772256162473 ) ) ;
#10934 = AXIS2_PLACEMENT_3D ( 'NONE', #30993, #27074, #21308 ) ;
#10935 = AXIS2_PLACEMENT_3D ( 'NONE', #15076, #30752, #37307 ) ;
#10936 = CARTESIAN_POINT ( 'NONE',  ( -0.4747269484695719743, -32.18314005917732601, 7.635761828346577573 ) ) ;
#10937 = ORIENTED_EDGE ( 'NONE', *, *, #1378, .F. ) ;
#10938 = CARTESIAN_POINT ( 'NONE',  ( 21.48247406815364613, 3.876925869359153509, 3.508130194431774207 ) ) ;
#10939 = CARTESIAN_POINT ( 'NONE',  ( -70.92837670882107659, 28.72470171467712063, 4.000000000000005329 ) ) ;
#10940 = CARTESIAN_POINT ( 'NONE',  ( 67.50273067437429120, 58.00668225682344570, -3.993945454764282310 ) ) ;
#10941 = CARTESIAN_POINT ( 'NONE',  ( 3.073907603833451851, -26.35069681102080708, 6.931070083220554068 ) ) ;
#10942 = ORIENTED_EDGE ( 'NONE', *, *, #315, .F. ) ;
#10943 = DIRECTION ( 'NONE',  ( -0.000000000000000000, -1.000000000000000000, -0.000000000000000000 ) ) ;
#10944 = CARTESIAN_POINT ( 'NONE',  ( 3.862587397715897541, -32.19384001730296063, 7.782167645815905033 ) ) ;
#10945 = LINE ( 'NONE', #23525, #9507 ) ;
#10946 = CARTESIAN_POINT ( 'NONE',  ( 2.315998556607181236, -32.91373647356815013, 7.652160403243383868 ) ) ;
#10947 = CYLINDRICAL_SURFACE ( 'NONE', #6310, 0.1000000000000028644 ) ;
#10948 = CARTESIAN_POINT ( 'NONE',  ( 1.275896657681770074, -26.09576640599786046, 6.989977667959447416 ) ) ;
#10949 = ORIENTED_EDGE ( 'NONE', *, *, #39961, .T. ) ;
#10950 = CARTESIAN_POINT ( 'NONE',  ( 21.99629294673994551, 5.575760840298564780, 3.113047709983713940 ) ) ;
#10951 = CARTESIAN_POINT ( 'NONE',  ( 81.16957891225081312, 61.30398062001320625, -1.000000000000000000 ) ) ;
#10952 = CARTESIAN_POINT ( 'NONE',  ( 80.65823571794965119, 63.30623879605499837, 3.578839808218917895 ) ) ;
#10953 = CARTESIAN_POINT ( 'NONE',  ( -63.70768058868311812, 44.39675795731059793, 1.000000000000000000 ) ) ;
#10954 = ORIENTED_EDGE ( 'NONE', *, *, #16571, .T. ) ;
#10955 = CARTESIAN_POINT ( 'NONE',  ( 78.43336062804344522, 61.18469638573554903, -3.363831406679923752 ) ) ;
#10957 = CARTESIAN_POINT ( 'NONE',  ( 4.984671627384348547, -28.36018029005467866, 7.635761828346577573 ) ) ;
#10956 = CARTESIAN_POINT ( 'NONE',  ( 25.40497407019471865, 0.6693547542586180121, 4.599869742869072908 ) ) ;
#10958 = CIRCLE ( 'NONE', #27396, 21.28220113893567245 ) ;
#10959 = CARTESIAN_POINT ( 'NONE',  ( 80.30538902758895858, 65.37113732874213667, -3.059106349689739712 ) ) ;
#10960 = CARTESIAN_POINT ( 'NONE',  ( 79.19917379928831735, 63.30335940139927686, 3.774260586041106258 ) ) ;
#10961 = VECTOR ( 'NONE', #20192, 1000.000000000000000 ) ;
#10962 = AXIS2_PLACEMENT_3D ( 'NONE', #27346, #11887, #9013 ) ;
#10963 = EDGE_CURVE ( 'NONE', #3554, #16444, #25720, .T. ) ;
#10964 = CARTESIAN_POINT ( 'NONE',  ( -0.8909124383283257842, -27.36873829022893645, 7.779495906702011077 ) ) ;
#10965 = ADVANCED_FACE ( 'NONE', ( #31973 ), #20073, .T. ) ;
#10966 = CARTESIAN_POINT ( 'NONE',  ( 81.62248346935344046, 65.70993096190733240, 1.153249692834613427 ) ) ;
#10967 = DIRECTION ( 'NONE',  ( 0.000000000000000000, -1.000000000000000000, 0.000000000000000000 ) ) ;
#10968 = CARTESIAN_POINT ( 'NONE',  ( 28.08579234408868786, -0.7886013899455160958, -6.074239229908586779 ) ) ;
#10969 = CARTESIAN_POINT ( 'NONE',  ( -1.526028259963971401, -30.94401141093381113, 7.139344958878410807 ) ) ;
#10970 = ORIENTED_EDGE ( 'NONE', *, *, #25915, .T. ) ;
#10971 = CARTESIAN_POINT ( 'NONE',  ( -66.99872204295122913, 28.48507918597134037, -12.49999999999999645 ) ) ;
#10972 = CARTESIAN_POINT ( 'NONE',  ( 24.74154467618137332, 0.6006174455902917320, -4.777991240237089876 ) ) ;
#10973 = DIRECTION ( 'NONE',  ( 0.000000000000000000, 0.000000000000000000, 1.000000000000000000 ) ) ;
#10974 = CARTESIAN_POINT ( 'NONE',  ( 2.322191688357494677, -25.34207446254166385, 7.754798119455333705 ) ) ;
#10975 = ORIENTED_EDGE ( 'NONE', *, *, #3300, .F. ) ;
#10976 = CARTESIAN_POINT ( 'NONE',  ( 37.10393103747592392, -3.125961714947245174, -5.976270759528274468 ) ) ;
#10977 = DIRECTION ( 'NONE',  ( 1.000000000000000000, 0.000000000000000000, 0.000000000000000000 ) ) ;
#10978 = CARTESIAN_POINT ( 'NONE',  ( -9.439742135462632078, 51.66544268451064426, -1.000000000000000000 ) ) ;
#10979 = CARTESIAN_POINT ( 'NONE',  ( 5.113370443964368128, -30.34553905407643626, 7.011627023500182965 ) ) ;
#10980 = DIRECTION ( 'NONE',  ( -0.4711084086744811716, -0.8820753183692411348, 0.000000000000000000 ) ) ;
#10981 = DIRECTION ( 'NONE',  ( 0.000000000000000000, 0.000000000000000000, -1.000000000000000000 ) ) ;
#10982 = DIRECTION ( 'NONE',  ( 0.000000000000000000, -0.7541618601367581221, 0.6566885781822803247 ) ) ;
#10983 = DIRECTION ( 'NONE',  ( 0.000000000000000000, 0.000000000000000000, -1.000000000000000000 ) ) ;
#10984 = CARTESIAN_POINT ( 'NONE',  ( 2.194212249870564069, -33.03491787133889801, 6.865482280155368322 ) ) ;
#10985 = ORIENTED_EDGE ( 'NONE', *, *, #7572, .T. ) ;
#10986 = CARTESIAN_POINT ( 'NONE',  ( 66.57570644833764106, 57.81776741001107922, 3.999845987728086083 ) ) ;
#10987 = CARTESIAN_POINT ( 'NONE',  ( 73.13464764220530867, 62.20839851451114555, -3.391332960900173887 ) ) ;
#10988 = AXIS2_PLACEMENT_3D ( 'NONE', #9612, #8783, #15993 ) ;
#10989 = ORIENTED_EDGE ( 'NONE', *, *, #18544, .F. ) ;
#10990 = CARTESIAN_POINT ( 'NONE',  ( 84.23599009083828548, 2.852497016463987567, -2.111805961397795084 ) ) ;
#10991 = PLANE ( 'NONE',  #35746 ) ;
#10992 = CARTESIAN_POINT ( 'NONE',  ( -0.9258490509262529145, -27.25630360209614977, 6.865554069792297653 ) ) ;
#10993 = DIRECTION ( 'NONE',  ( 0.000000000000000000, -0.000000000000000000, 1.000000000000000000 ) ) ;
#10994 = DIRECTION ( 'NONE',  ( -0.000000000000000000, -0.000000000000000000, 1.000000000000000000 ) ) ;
#10995 = DIRECTION ( 'NONE',  ( 0.000000000000000000, 0.000000000000000000, -1.000000000000000000 ) ) ;
#10996 = ORIENTED_EDGE ( 'NONE', *, *, #27148, .T. ) ;
#10997 = CARTESIAN_POINT ( 'NONE',  ( 80.83613523452670790, 61.24682340193510299, -1.855758959884428849 ) ) ;
#10998 = CARTESIAN_POINT ( 'NONE',  ( 14.38908530706053490, 8.635444686654100366, -3.482730190673553938 ) ) ;
#10999 = CARTESIAN_POINT ( 'NONE',  ( 80.20116317610164458, 62.79640268260013158, 3.571698303486883663 ) ) ;
#11000 = DIRECTION ( 'NONE',  ( -0.000000000000000000, 1.000000000000000000, -0.000000000000000000 ) ) ;
#11001 = CARTESIAN_POINT ( 'NONE',  ( 0.3869751666866692030, -32.81414707076048387, 7.751599049952199394 ) ) ;
#11002 = ADVANCED_FACE ( 'NONE', ( #9831, #34977 ), #6752, .T. ) ;
#11003 = CARTESIAN_POINT ( 'NONE',  ( 3.926835433623051763, -27.00030981652402318, 6.889465824494256374 ) ) ;
#11004 = DIRECTION ( 'NONE',  ( 0.000000000000000000, 0.000000000000000000, 1.000000000000000000 ) ) ;
#11005 =( GEOMETRIC_REPRESENTATION_CONTEXT ( 3 ) GLOBAL_UNCERTAINTY_ASSIGNED_CONTEXT ( ( #21353 ) ) GLOBAL_UNIT_ASSIGNED_CONTEXT ( ( #19275, #349, #25655 ) ) REPRESENTATION_CONTEXT ( 'NONE', 'WORKASPACE' ) );
#11006 = CARTESIAN_POINT ( 'NONE',  ( 21.85643539959775694, 5.081979399238238493, 12.23420521612613143 ) ) ;
#11007 = CIRCLE ( 'NONE', #28136, 0.1000000000000028644 ) ;
#11008 = CARTESIAN_POINT ( 'NONE',  ( -77.95330471031414277, 33.71485196875532608, -46.17089178453873188 ) ) ;
#11009 = ORIENTED_EDGE ( 'NONE', *, *, #35490, .T. ) ;
#11010 = PLANE ( 'NONE',  #8393 ) ;
#11011 = ORIENTED_EDGE ( 'NONE', *, *, #24795, .T. ) ;
#11012 = CARTESIAN_POINT ( 'NONE',  ( 14.75848712228891912, -5.150036851632115109, 2.500000000037279957 ) ) ;
#11013 = CARTESIAN_POINT ( 'NONE',  ( -79.28524469389549267, 10.39485579098267287, -5.506563355727433162 ) ) ;
#11014 = CARTESIAN_POINT ( 'NONE',  ( -0.2169689478323021947, -26.75353354193401501, 7.505001789837628223 ) ) ;
#11015 = CARTESIAN_POINT ( 'NONE',  ( 36.49377363026633248, -3.561668432020718367, -5.795624143399630945 ) ) ;
#11016 = CARTESIAN_POINT ( 'NONE',  ( 80.84084779726516956, 63.39242392479003740, 3.526329879082121810 ) ) ;
#11017 = CARTESIAN_POINT ( 'NONE',  ( -1.498372880175843580, -30.72231214854605952, 7.775108481317163367 ) ) ;
#11018 = B_SPLINE_CURVE_WITH_KNOTS ( 'NONE', 3,
 ( #35096, #35692, #3804, #13440, #16323, #28897 ),
 .UNSPECIFIED., .F., .F.,
 ( 4, 2, 4 ),
 ( 4.336808689942017736E-19, 0.001078930742623167250, 0.002157861485246334067 ),
 .UNSPECIFIED. ) ;
#11019 = DIRECTION ( 'NONE',  ( 1.000000000000000000, 0.000000000000000000, 0.000000000000000000 ) ) ;
#11020 = CARTESIAN_POINT ( 'NONE',  ( -0.07963814550968341399, -26.55637667292353754, 7.678495282201402539 ) ) ;
#11021 = LINE ( 'NONE', #11830, #1730 ) ;
#11022 = CARTESIAN_POINT ( 'NONE',  ( -64.41607093812410767, 34.69667448355765771, 5.588514499911548583 ) ) ;
#11023 = CARTESIAN_POINT ( 'NONE',  ( 87.46698719228061236, 0.1106531486882382370, 4.398961038131239398 ) ) ;
#11024 = CARTESIAN_POINT ( 'NONE',  ( 5.145088616758716427, -28.91287462443592560, 7.255881584735162981 ) ) ;
#11025 =( BOUNDED_SURFACE ( )  B_SPLINE_SURFACE ( 3, 2, ( 
 ( #4548, #23083, #4739 ),
 ( #38500, #11097, #29456 ),
 ( #1069, #35450, #33154 ),
 ( #13994, #7821, #7223 ),
 ( #17270, #13600, #26567 ),
 ( #32555, #1871, #20568 ),
 ( #4939, #23477, #7622 ),
 ( #26171, #29650, #23668 ),
 ( #29852, #38705, #19784 ),
 ( #36234, #20176, #8012 ),
 ( #35647, #38906, #7417 ),
 ( #19975, #4354, #1266 ),
 ( #10698, #30259, #21611 ),
 ( #30681, #23857, #27162 ),
 ( #33570, #39717, #2490 ),
 ( #18090, #2697, #30885 ),
 ( #12113, #34192, #8621 ),
 ( #30467, #9034, #5957 ),
 ( #18502, #15012, #2078 ),
 ( #27367, #31086, #5349 ),
 ( #2896, #15215, #21409 ),
 ( #37037, #26965, #24692 ) ),
 .UNSPECIFIED., .F., .F., .T. ) 
 B_SPLINE_SURFACE_WITH_KNOTS ( ( 4, 2, 2, 2, 2, 2, 2, 2, 2, 2, 4 ),
 ( 3, 3 ),
 ( 0.02037793668903936650, 0.02161998616042463614, 0.02224101089611726922, 0.02286203563180990578, 0.02410408510319517195, 0.02534613457458044158, 0.02658818404596571122, 0.02720920878165834431, 0.02783023351735097739, 0.02907228298873624703, 0.03031433246012151667 ),
 ( 0.1026333575651713903, 1.000000000000000000 ),
 .UNSPECIFIED. ) 
 GEOMETRIC_REPRESENTATION_ITEM ( )  RATIONAL_B_SPLINE_SURFACE ( (
 ( 0.9460492146741656949, 0.7371673956414426243, 1.000000000000000000),
 ( 0.9472507007640582621, 0.7430206879744423176, 1.000000000000000000),
 ( 0.9486044478916659806, 0.7496157519951633930, 1.000000000000000000),
 ( 0.9508882531966607043, 0.7607417901526136728, 1.000000000000000000),
 ( 0.9516917417591811423, 0.7646561537746467963, 1.000000000000000000),
 ( 0.9533874343465102985, 0.7729170770629283371, 1.000000000000000000),
 ( 0.9542843507619054311, 0.7772865941316136063, 1.000000000000000000),
 ( 0.9570723184632317082, 0.7908687655009754014, 1.000000000000000000),
 ( 0.9590598677958013241, 0.8005515303433297092, 1.000000000000000000),
 ( 0.9632568686825866422, 0.8209981033988795751, 1.000000000000000000),
 ( 0.9654881076387393790, 0.8318680535256492981, 1.000000000000000000),
 ( 0.9699646227543765598, 0.8536763389692718640, 1.000000000000000000),
 ( 0.9722104709448077253, 0.8646174610552612716, 1.000000000000000000),
 ( 0.9754590750861481530, 0.8804437197805374815, 1.000000000000000000),
 ( 0.9765212693044509340, 0.8856184224478864664, 1.000000000000000000),
 ( 0.9785718366633011644, 0.8956081928670607262, 1.000000000000000000),
 ( 0.9795574793614638676, 0.9004099586942033717, 1.000000000000000000),
 ( 0.9822852879408858762, 0.9136990522410552984, 1.000000000000000000),
 ( 0.9838235476076093722, 0.9211930079257193427, 1.000000000000000000),
 ( 0.9859690325004739631, 0.9316451890867138985, 1.000000000000000000),
 ( 0.9865248671184559948, 0.9343530544005280714, 1.000000000000000000),
 ( 0.9864639028331373405, 0.9340560540550024715, 1.000000000000000000) ) ) 
 REPRESENTATION_ITEM ( '' )  SURFACE ( )  );
#11026 = CARTESIAN_POINT ( 'NONE',  ( 67.71971274774827521, 58.31971506597766819, 3.997018227265501267 ) ) ;
#11027 = CARTESIAN_POINT ( 'NONE',  ( 21.25657249720342890, 3.328711648262387079, 3.524000248973877980 ) ) ;
#11028 = EDGE_CURVE ( 'NONE', #5443, #8785, #22287, .T. ) ;
#11029 = AXIS2_PLACEMENT_3D ( 'NONE', #6351, #3488, #3085 ) ;
#11030 = CARTESIAN_POINT ( 'NONE',  ( -70.92837670882107659, -23.80776546975053165, 0.000000000000000000 ) ) ;
#11031 = CARTESIAN_POINT ( 'NONE',  ( 86.06476644049696745, 1.615394338423677079, -5.255309406831162988 ) ) ;
#11033 = CARTESIAN_POINT ( 'NONE',  ( 28.38493088217029836, 0.6184565668324991661, -4.636552974946980932 ) ) ;
#11032 = CARTESIAN_POINT ( 'NONE',  ( 81.21317738564107458, 61.78038839029203189, -2.432199249741020086 ) ) ;
#11034 = CARTESIAN_POINT ( 'NONE',  ( -1.370619673614267287, -31.23390196357851778, 7.776484688137385248 ) ) ;
#11035 = LINE ( 'NONE', #19527, #32045 ) ;
#11036 = CARTESIAN_POINT ( 'NONE',  ( -59.00289461565213855, 28.67396232720155780, 6.820567581290490899 ) ) ;
#11037 = ORIENTED_EDGE ( 'NONE', *, *, #4786, .F. ) ;
#11038 = CARTESIAN_POINT ( 'NONE',  ( -76.03073930765792454, 10.38232506267625688, -8.602311807112798192 ) ) ;
#11039 = CARTESIAN_POINT ( 'NONE',  ( 1.314511067807684341, -26.19189860009866422, 6.929923840112063083 ) ) ;
#11040 = AXIS2_PLACEMENT_3D ( 'NONE', #1957, #2570, #5429 ) ;
#11041 = ORIENTED_EDGE ( 'NONE', *, *, #10029, .T. ) ;
#11042 = CARTESIAN_POINT ( 'NONE',  ( -71.55887904216392315, -21.56717086459383026, 3.967530720604706573 ) ) ;
#11043 = EDGE_CURVE ( 'NONE', #3556, #23841, #1583, .T. ) ;
#11044 = VERTEX_POINT ( 'NONE', #13734 ) ;
#11045 = APPLICATION_CONTEXT ( 'automotive_design' ) ;
#11046 = CARTESIAN_POINT ( 'NONE',  ( 79.39546522070064327, 65.15502244391674935, -3.213872034465286021 ) ) ;
#11047 = CARTESIAN_POINT ( 'NONE',  ( -12.34874870218063947, -26.64985754041175525, 6.800000000000000711 ) ) ;
#11048 = CARTESIAN_POINT ( 'NONE',  ( 80.39050082614866710, 63.54812927569808778, 3.668443954219270164 ) ) ;
#11049 = CARTESIAN_POINT ( 'NONE',  ( 21.92288564526636563, 0.6275057185515289238, 7.506979565206076899 ) ) ;
#11051 = ORIENTED_EDGE ( 'NONE', *, *, #1420, .F. ) ;
#11050 = FACE_OUTER_BOUND ( 'NONE', #24583, .T. ) ;
#11052 = CARTESIAN_POINT ( 'NONE',  ( 0.01666963137263145420, -32.52375573787565344, 7.748216051605119503 ) ) ;
#11053 = AXIS2_PLACEMENT_3D ( 'NONE', #25182, #26202, #4382 ) ;
#11054 = EDGE_CURVE ( 'NONE', #13186, #5702, #2576, .T. ) ;
#11056 = CARTESIAN_POINT ( 'NONE',  ( 19.45444762555048968, 11.13896630658038056, 2.499999999999995115 ) ) ;
#11055 = CARTESIAN_POINT ( 'NONE',  ( 1.700390093233090871, -29.56993018339339940, -8.199999999999999289 ) ) ;
#11057 = CARTESIAN_POINT ( 'NONE',  ( -1.213445411319114209, -27.81791344477159100, 7.785172627573962778 ) ) ;
#11058 = FACE_OUTER_BOUND ( 'NONE', #30254, .T. ) ;
#11059 = DIRECTION ( 'NONE',  ( -1.000000000000000000, 0.000000000000000000, 0.000000000000000000 ) ) ;
#11060 = CARTESIAN_POINT ( 'NONE',  ( 23.40982567674854309, 3.536491107301646064, -3.507547231203631988 ) ) ;
#11061 = VERTEX_POINT ( 'NONE', #26297 ) ;
#11062 = CARTESIAN_POINT ( 'NONE',  ( 5.124306173303248002, -30.29170089314414582, 7.761113333117553026 ) ) ;
#11063 = ORIENTED_EDGE ( 'NONE', *, *, #36631, .T. ) ;
#11064 = CARTESIAN_POINT ( 'NONE',  ( 21.85643539959776760, 7.937350203533870996, 6.559150378249414715 ) ) ;
#11065 = CARTESIAN_POINT ( 'NONE',  ( 17.82514609008682172, 11.84176510169323748, 2.499999999999998668 ) ) ;
#11066 = CARTESIAN_POINT ( 'NONE',  ( 0.9730757925788008356, -32.99329091482906762, 7.754798119455333705 ) ) ;
#11067 = CARTESIAN_POINT ( 'NONE',  ( 80.21610222778484456, 65.32174013293413850, 3.113722587674275566 ) ) ;
#11068 = CARTESIAN_POINT ( 'NONE',  ( 84.32156544206206661, 3.079100735703119707, -0.4907544566128131391 ) ) ;
#11069 = PLANE ( 'NONE',  #3634 ) ;
#11070 = EDGE_LOOP ( 'NONE', ( #13892, #3584, #26340, #37811 ) ) ;
#11071 = DIRECTION ( 'NONE',  ( -1.000000000000000000, 0.000000000000000000, 0.000000000000000000 ) ) ;
#11072 = EDGE_CURVE ( 'NONE', #4011, #39825, #34110, .T. ) ;
#11073 = DIRECTION ( 'NONE',  ( 0.2567910337120358211, -0.7055275666422125003, -0.6605219282605404585 ) ) ;
#11074 = CARTESIAN_POINT ( 'NONE',  ( 21.50914624065722691, -2.894264267616096120, -3.541302231922554000 ) ) ;
#11075 = CARTESIAN_POINT ( 'NONE',  ( 37.04510231533804898, -2.801254996599130020, -5.988182174130333379 ) ) ;
#11076 = DIRECTION ( 'NONE',  ( 1.000000000000000000, 0.000000000000000000, 0.000000000000000000 ) ) ;
#11077 = CARTESIAN_POINT ( 'NONE',  ( 22.34798716198837454, 0.2922943786608916961, -6.997897115895016285 ) ) ;
#11078 = CARTESIAN_POINT ( 'NONE',  ( -52.01549048184568846, -30.38627270959228710, 4.800000000000000711 ) ) ;
#11079 = ORIENTED_EDGE ( 'NONE', *, *, #39358, .F. ) ;
#11080 = CARTESIAN_POINT ( 'NONE',  ( 2.836375080312453445, -32.86472044869006481, 7.785593909369612931 ) ) ;
#11081 = CARTESIAN_POINT ( 'NONE',  ( 3.417826084928983654, -32.50428837397927850, 7.643333865083954848 ) ) ;
#11082 = CARTESIAN_POINT ( 'NONE',  ( 32.42603576456313164, -3.007759285847489750, -5.267265126335289871 ) ) ;
#11083 = AXIS2_PLACEMENT_3D ( 'NONE', #36393, #14754, #26727 ) ;
#11084 = VERTEX_POINT ( 'NONE', #17201 ) ;
#11085 = ORIENTED_EDGE ( 'NONE', *, *, #250, .F. ) ;
#11086 = CARTESIAN_POINT ( 'NONE',  ( 30.88361545799471486, 0.6996882436838504082, 4.491048756100919803 ) ) ;
#11087 = CARTESIAN_POINT ( 'NONE',  ( -1.604056983674224224, -30.72349439543635441, 6.880608371227951992 ) ) ;
#11088 = EDGE_CURVE ( 'NONE', #34426, #22624, #7744, .T. ) ;
#11089 = EDGE_CURVE ( 'NONE', #18492, #3377, #7941, .T. ) ;
#11090 = CARTESIAN_POINT ( 'NONE',  ( -62.85318495816863305, 36.92099889189292838, -4.451173097142522295 ) ) ;
#11091 = LINE ( 'NONE', #7815, #14546 ) ;
#11092 = EDGE_CURVE ( 'NONE', #21747, #23979, #16796, .T. ) ;
#11093 = VERTEX_POINT ( 'NONE', #14114 ) ;
#11094 = VERTEX_POINT ( 'NONE', #19902 ) ;
#11095 = CARTESIAN_POINT ( 'NONE',  ( -38.24874870218063450, -25.49307895267003587, 6.700000000000000178 ) ) ;
#11096 = ORIENTED_EDGE ( 'NONE', *, *, #1832, .T. ) ;
#11097 = CARTESIAN_POINT ( 'NONE',  ( -55.57018072619552385, 31.35870463729781576, -3.952748674019516795 ) ) ;
#11099 = FACE_OUTER_BOUND ( 'NONE', #31647, .T. ) ;
#11098 = CARTESIAN_POINT ( 'NONE',  ( 4.821180714308241910, -27.98542208956447652, 6.980586498568966292 ) ) ;
#11100 = ORIENTED_EDGE ( 'NONE', *, *, #26415, .F. ) ;
#11101 = CARTESIAN_POINT ( 'NONE',  ( 22.46827172332250200, 4.617652435747735318, 3.274651054683074491 ) ) ;
#11102 = CARTESIAN_POINT ( 'NONE',  ( 81.84349429120946695, 61.90138267109050929, -1.539394129974354763 ) ) ;
#11103 = DIRECTION ( 'NONE',  ( -0.000000000000000000, -1.000000000000000000, -0.000000000000000000 ) ) ;
#11104 = AXIS2_PLACEMENT_3D ( 'NONE', #36662, #30093, #11324 ) ;
#11105 = CARTESIAN_POINT ( 'NONE',  ( 14.61802081865033642, -4.461995682952384357, -2.500000000000000000 ) ) ;
#11106 = ORIENTED_EDGE ( 'NONE', *, *, #26104, .F. ) ;
#11108 = CARTESIAN_POINT ( 'NONE',  ( 24.89046942861130063, -2.711312442094912623, -4.091157751249474117 ) ) ;
#11107 = CARTESIAN_POINT ( 'NONE',  ( -70.92837670882107659, 15.04836564048558500, 0.000000000000000000 ) ) ;
#11109 = CARTESIAN_POINT ( 'NONE',  ( 20.71918928157063178, 6.165415561970744918, -3.398715681700897662 ) ) ;
#11110 = CARTESIAN_POINT ( 'NONE',  ( 74.21382537490346465, 62.79450482958245772, 3.300071129360917066 ) ) ;
#11111 = CARTESIAN_POINT ( 'NONE',  ( 21.84929449939717117, 2.757990278203812817, -5.323232446221868308 ) ) ;
#11112 = ORIENTED_EDGE ( 'NONE', *, *, #13158, .T. ) ;
#11113 = DIRECTION ( 'NONE',  ( 0.000000000000000000, 0.000000000000000000, -1.000000000000000000 ) ) ;
#11114 = CARTESIAN_POINT ( 'NONE',  ( -70.92837670882074974, 0.2169278855384722815, 6.000000000000007994 ) ) ;
#11115 = B_SPLINE_CURVE_WITH_KNOTS ( 'NONE', 3,
 ( #26088, #38220, #6548, #37812, #25879, #19093, #22600, #982, #10018, #22802, #35373, #38419, #31662, #16590, #6745, #16399, #15804, #16000, #7141, #28568, #28773, #35169, #25280, #28973, #29172, #775, #18891, #38023, #19702, #13518, #9616 ),
 .UNSPECIFIED., .F., .F.,
 ( 4, 3, 3, 3, 3, 3, 3, 3, 3, 3, 4 ),
 ( 0.000000000000000000, 2.999644130997519527E-05, 6.002588995694434291E-05, 8.960886084587663797E-05, 0.0001190604700446430892, 0.0001489538463052673836, 0.0001796139255493884224, 0.0002109707048516977815, 0.0002426195318110361968, 0.0002740640997890006546, 0.0002849778069099816549 ),
 .UNSPECIFIED. ) ;
#11116 = AXIS2_PLACEMENT_3D ( 'NONE', #10658, #7182, #29215 ) ;
#11117 = CARTESIAN_POINT ( 'NONE',  ( 27.43879703630890887, 0.9604363013853572939, -4.488885905966782275 ) ) ;
#11118 = CARTESIAN_POINT ( 'NONE',  ( -1.258681128443422281, -27.89544593293122787, 7.661510568013095046 ) ) ;
#11119 = FACE_OUTER_BOUND ( 'NONE', #35544, .T. ) ;
#11120 = CARTESIAN_POINT ( 'NONE',  ( 81.39510468133838117, 61.43011602722285147, 1.270639542487624007 ) ) ;
#11121 = CARTESIAN_POINT ( 'NONE',  ( 85.09836244081553502, 2.771204891246429547, 1.045684100250478643 ) ) ;
#11122 = CARTESIAN_POINT ( 'NONE',  ( 31.86155337613836380, -4.142523116122148963, 4.178567150506776962 ) ) ;
#11123 = CARTESIAN_POINT ( 'NONE',  ( 4.657149580636700037, -31.24850351647889823, 7.740055089680397238 ) ) ;
#11124 = CARTESIAN_POINT ( 'NONE',  ( -80.78031099096216394, -5.651013701725611682, -4.946895140558772219 ) ) ;
#11125 = EDGE_CURVE ( 'NONE', #26757, #29749, #32875, .T. ) ;
#11126 = CARTESIAN_POINT ( 'NONE',  ( 14.79476812666557350, -5.587083218280035624, 2.503656380302125228 ) ) ;
#11127 = DIRECTION ( 'NONE',  ( 0.000000000000000000, 0.000000000000000000, 1.000000000000000000 ) ) ;
#11128 = CARTESIAN_POINT ( 'NONE',  ( 34.76872341006280465, -3.305568305793640693, -5.632898191526192200 ) ) ;
#11129 = CARTESIAN_POINT ( 'NONE',  ( -30.87867591359218977, -26.64985754041175525, 6.800000000000000711 ) ) ;
#11130 = CARTESIAN_POINT ( 'NONE',  ( -1.547547272396095464, -28.27830587817873820, 7.771081512783704959 ) ) ;
#11131 = EDGE_CURVE ( 'NONE', #31247, #9551, #23398, .T. ) ;
#11132 = VECTOR ( 'NONE', #17442, 1000.000000000000000 ) ;
#11133 = PLANE ( 'NONE',  #9230 ) ;
#11134 = EDGE_CURVE ( 'NONE', #25426, #8794, #16999, .T. ) ;
#11135 = ORIENTED_EDGE ( 'NONE', *, *, #13323, .T. ) ;
#11136 = CARTESIAN_POINT ( 'NONE',  ( 33.67412422684426332, -3.719468122262790999, 5.264089307504189463 ) ) ;
#11137 = CARTESIAN_POINT ( 'NONE',  ( -70.21272673770054951, -0.07566977545864603250, 5.969620261456469734 ) ) ;
#11138 = CARTESIAN_POINT ( 'NONE',  ( 67.06207392303235792, 57.84849753947618467, -3.994852852620101480 ) ) ;
#11139 = EDGE_CURVE ( 'NONE', #35057, #20163, #14337, .T. ) ;
#11140 = FACE_OUTER_BOUND ( 'NONE', #21635, .T. ) ;
#11141 = ORIENTED_EDGE ( 'NONE', *, *, #22165, .F. ) ;
#11142 = CARTESIAN_POINT ( 'NONE',  ( -0.5600293521546132469, -32.10973131848952278, 7.774064877406533292 ) ) ;
#11143 = AXIS2_PLACEMENT_3D ( 'NONE', #3469, #22995, #4259 ) ;
#11144 = CARTESIAN_POINT ( 'NONE',  ( 1.700390093233090871, -29.56993018339339940, 7.750000000000000888 ) ) ;
#11145 = CARTESIAN_POINT ( 'NONE',  ( 78.31613663886943755, 65.79311636994390255, 1.652891522390884216 ) ) ;
#11146 = CARTESIAN_POINT ( 'NONE',  ( 1.027987119375220360, -32.90277795080599077, 6.870716933885664623 ) ) ;
#11147 = CARTESIAN_POINT ( 'NONE',  ( 0.3457495631895174948, -32.79715019981050972, 7.013842709614101167 ) ) ;
#11148 = LINE ( 'NONE', #8258, #30418 ) ;
#11149 = ORIENTED_EDGE ( 'NONE', *, *, #8074, .T. ) ;
#11150 = CARTESIAN_POINT ( 'NONE',  ( 21.83153479609358882, 5.955861309579818297, 3.139072512424320838 ) ) ;
#11151 = DIRECTION ( 'NONE',  ( 0.000000000000000000, 0.000000000000000000, -1.000000000000000000 ) ) ;
#11152 = CARTESIAN_POINT ( 'NONE',  ( 79.70553327529583498, 65.02082924290297683, 3.340002271463677896 ) ) ;
#11153 = CARTESIAN_POINT ( 'NONE',  ( -0.01837800939314739035, -32.61883756299590686, 7.695279973900954751 ) ) ;
#11154 = VERTEX_POINT ( 'NONE', #29377 ) ;
#11155 = CARTESIAN_POINT ( 'NONE',  ( 78.10617727715711567, 63.31486359019600485, -3.780406938340842515 ) ) ;
#11157 = CARTESIAN_POINT ( 'NONE',  ( 14.68539485748044626, -4.702058589831320745, -2.500000000000172307 ) ) ;
#11156 = CARTESIAN_POINT ( 'NONE',  ( 26.76119839104307729, 0.8702342918438391584, 4.383274761122565089 ) ) ;
#11158 = CARTESIAN_POINT ( 'NONE',  ( 79.69124582247823696, 65.94093779614992457, -2.443770662193227139 ) ) ;
#11159 = CARTESIAN_POINT ( 'NONE',  ( 79.25863321418395913, 62.43675908411266562, 3.670385203786648010 ) ) ;
#11160 = VERTEX_POINT ( 'NONE', #39636 ) ;
#11161 = AXIS2_PLACEMENT_3D ( 'NONE', #4044, #3246, #25441 ) ;
#11162 = CARTESIAN_POINT ( 'NONE',  ( -0.8715445521076354840, -27.34613762201350795, 7.785868773668302545 ) ) ;
#11163 = CARTESIAN_POINT ( 'NONE',  ( 82.33210628740353343, 64.54215504103274270, 1.775718711109096404 ) ) ;
#11164 = CARTESIAN_POINT ( 'NONE',  ( 63.05383694556373797, -7.271989087314214117, -6.000000000000000000 ) ) ;
#11165 = CARTESIAN_POINT ( 'NONE',  ( 30.06379901557190237, -4.186058752285889639, 3.090730270791094636 ) ) ;
#11166 = CARTESIAN_POINT ( 'NONE',  ( 4.465382618493274336, -31.56070191054703145, 7.505001789837627335 ) ) ;
#11167 = ORIENTED_EDGE ( 'NONE', *, *, #39224, .F. ) ;
#11168 = DIRECTION ( 'NONE',  ( -0.000000000000000000, -0.000000000000000000, -1.000000000000000000 ) ) ;
#11169 = CARTESIAN_POINT ( 'NONE',  ( 27.43552295442261268, 0.9748355693916180842, -4.488373114136018138 ) ) ;
#11170 = CARTESIAN_POINT ( 'NONE',  ( 17.97454669799173033, 51.66243977840390755, 4.000000000000000000 ) ) ;
#11171 = CARTESIAN_POINT ( 'NONE',  ( -62.86576508122317364, 38.67912974266874926, 4.000000000000000000 ) ) ;
#11172 = DIRECTION ( 'NONE',  ( 1.000000000000000000, 0.000000000000000000, 0.000000000000000000 ) ) ;
#11173 = AXIS2_PLACEMENT_3D ( 'NONE', #34659, #31550, #3373 ) ;
#11174 = CARTESIAN_POINT ( 'NONE',  ( 5.151060735156064219, -30.15551690657623851, 7.646866513072557936 ) ) ;
#11175 = CARTESIAN_POINT ( 'NONE',  ( 27.81554284938481203, 1.843609864746671212, -3.908850080722512388 ) ) ;
#11176 = CARTESIAN_POINT ( 'NONE',  ( 3.454978868039249473, -32.59677836288253161, 7.762796336881260473 ) ) ;
#11177 = CARTESIAN_POINT ( 'NONE',  ( 3.282272078954445060, -32.69205414914204511, 6.971170733404095543 ) ) ;
#11178 = CARTESIAN_POINT ( 'NONE',  ( -1.086373026989221113, -31.68746443619045650, 7.013842709614101167 ) ) ;
#11179 = DIRECTION ( 'NONE',  ( -0.000000000000000000, 0.000000000000000000, 1.000000000000000000 ) ) ;
#11180 = DIRECTION ( 'NONE',  ( 0.000000000000000000, 0.000000000000000000, 1.000000000000000000 ) ) ;
#11181 = DIRECTION ( 'NONE',  ( 0.000000000000000000, 0.000000000000000000, -1.000000000000000000 ) ) ;
#11182 = CARTESIAN_POINT ( 'NONE',  ( 1.876920399658227989, -26.07437817348433384, 6.903112506833889661 ) ) ;
#11183 = ORIENTED_EDGE ( 'NONE', *, *, #4584, .F. ) ;
#11184 = CARTESIAN_POINT ( 'NONE',  ( -28.87867591359218977, -26.64985754041175525, 6.700000000000000178 ) ) ;
#11185 = CARTESIAN_POINT ( 'NONE',  ( 73.17398396214588274, 60.59975200455691891, -3.944160774623525434 ) ) ;
#11186 = EDGE_CURVE ( 'NONE', #6683, #38144, #7552, .T. ) ;
#11187 = EDGE_CURVE ( 'NONE', #25932, #3811, #3033, .T. ) ;
#11188 = ORIENTED_EDGE ( 'NONE', *, *, #22059, .T. ) ;
#11189 = CARTESIAN_POINT ( 'NONE',  ( 86.70396871743868417, -0.5679530053852996918, -5.718564545587779158 ) ) ;
#11190 = ADVANCED_FACE ( 'NONE', ( #28105 ), #31012, .T. ) ;
#11191 = CARTESIAN_POINT ( 'NONE',  ( -2.248748702180634940, -26.64985754041175525, 6.800000000000000711 ) ) ;
#11192 = CARTESIAN_POINT ( 'NONE',  ( 3.024182384487883457, -26.43822554061266672, 6.882085323592686876 ) ) ;
#11193 = CARTESIAN_POINT ( 'NONE',  ( -1.416686097061773397, -28.21205094579645589, 6.959317978105164393 ) ) ;
#11194 = CARTESIAN_POINT ( 'NONE',  ( -21.07867591359219617, -26.64985754041175525, 6.700000000000000178 ) ) ;
#11195 = CONTEXT_DEPENDENT_SHAPE_REPRESENTATION ( #1119, #3991 ) ;
#11196 = CARTESIAN_POINT ( 'NONE',  ( -72.45330471031414277, 33.71485196875532608, 12.50000000000000000 ) ) ;
#11197 = DIRECTION ( 'NONE',  ( -0.000000000000000000, -0.000000000000000000, 1.000000000000000000 ) ) ;
#11198 = DIRECTION ( 'NONE',  ( 8.659560562354932858E-17, -0.7071067811865474617, 0.7071067811865474617 ) ) ;
#11199 = ORIENTED_EDGE ( 'NONE', *, *, #8395, .T. ) ;
#11200 = CIRCLE ( 'NONE', #17758, 10.00000000000000533 ) ;
#11201 = ORIENTED_EDGE ( 'NONE', *, *, #5549, .F. ) ;
#11202 = CARTESIAN_POINT ( 'NONE',  ( 79.01107290893718016, 64.84207397985339583, -3.331801170923394562 ) ) ;
#11203 = CARTESIAN_POINT ( 'NONE',  ( 17.60335279841272182, 11.93951228567222600, -2.500000000000012434 ) ) ;
#11204 = CARTESIAN_POINT ( 'NONE',  ( 80.24765655772201001, 65.96146312294936820, -2.334361474589122576 ) ) ;
#11205 = CARTESIAN_POINT ( 'NONE',  ( 78.75925357433533236, 65.51276736450270732, 2.660933152496150811 ) ) ;
#11206 = CARTESIAN_POINT ( 'NONE',  ( 0.6507332215994441338, -26.33601230518184977, 7.757178535559535959 ) ) ;
#11207 = FACE_OUTER_BOUND ( 'NONE', #31266, .T. ) ;
#11208 = CARTESIAN_POINT ( 'NONE',  ( 4.034721127530844775, -27.09790394036370031, 6.997764925645181933 ) ) ;
#11209 = CARTESIAN_POINT ( 'NONE',  ( -34.44874870218064444, -26.64985754041175525, 6.800000000000000711 ) ) ;
#11210 = CARTESIAN_POINT ( 'NONE',  ( 21.85643539959777826, -5.315239383820637542, 13.63683724657638052 ) ) ;
#11211 = CARTESIAN_POINT ( 'NONE',  ( -79.02304780370427295, 11.44793877116905101, 5.885444661546937795 ) ) ;
#11212 = VECTOR ( 'NONE', #25955, 1000.000000000000000 ) ;
#11213 = CARTESIAN_POINT ( 'NONE',  ( 14.72131129160176322, -5.032869250705308772, 2.500000000000122569 ) ) ;
#11214 = CARTESIAN_POINT ( 'NONE',  ( -79.95507389475284299, 10.45503264499227214, -6.471215697590134930 ) ) ;
#11215 = CARTESIAN_POINT ( 'NONE',  ( -0.5222078730473904695, -32.14287757506037480, 6.894806418505348589 ) ) ;
#11216 = CARTESIAN_POINT ( 'NONE',  ( 36.87241546289296679, -2.085184201125469539, -5.863287844626394296 ) ) ;
#11217 = CARTESIAN_POINT ( 'NONE',  ( 78.88492378528533777, 66.04028779424464801, 1.804401104814770784 ) ) ;
#11218 = DIRECTION ( 'NONE',  ( 1.000000000000000000, 0.000000000000000000, 0.000000000000000000 ) ) ;
#11219 = CARTESIAN_POINT ( 'NONE',  ( -38.87867591359218977, -26.64985754041175525, 6.700000000000000178 ) ) ;
#11220 = CARTESIAN_POINT ( 'NONE',  ( -0.7402732514194279023, -31.94722237671934906, 7.505001789837626447 ) ) ;
#11221 = VECTOR ( 'NONE', #5160, 1000.000000000000000 ) ;
#11222 = CARTESIAN_POINT ( 'NONE',  ( 0.5553240519966275990, -26.26254091673501989, 6.875671892026062437 ) ) ;
#11223 = CARTESIAN_POINT ( 'NONE',  ( 4.434909129570597131, -27.38534655260518846, 6.865554069792296765 ) ) ;
#11224 = AXIS2_PLACEMENT_3D ( 'NONE', #30762, #17963, #8494 ) ;
#11225 = CARTESIAN_POINT ( 'NONE',  ( 87.61513118388886312, -0.05574921402413471339, 4.133600037482800360 ) ) ;
#11226 = CARTESIAN_POINT ( 'NONE',  ( -27.07867591359219972, -26.64985754041175525, 6.800000000000000711 ) ) ;
#11227 = CARTESIAN_POINT ( 'NONE',  ( 0.1069670619869697303, -26.56643171602332032, 7.754798119455333705 ) ) ;
#11228 = CARTESIAN_POINT ( 'NONE',  ( 67.43143073044585378, 58.20127550988744503, 3.998123450764769604 ) ) ;
#11229 = CARTESIAN_POINT ( 'NONE',  ( 36.90765050460312580, -3.026038577865985513, 5.966729494780605769 ) ) ;
#11230 = ORIENTED_EDGE ( 'NONE', *, *, #8115, .F. ) ;
#11231 = DIRECTION ( 'NONE',  ( 1.000000000000000000, -0.000000000000000000, 0.000000000000000000 ) ) ;
#11232 = CARTESIAN_POINT ( 'NONE',  ( 87.01296019436635731, 0.4868102506410553754, -5.723292304581113044 ) ) ;
#11233 = EDGE_CURVE ( 'NONE', #3356, #33357, #13461, .T. ) ;
#11235 = CARTESIAN_POINT ( 'NONE',  ( 33.62515361724260998, -1.226752319248198164, -5.454416468020780506 ) ) ;
#11234 = CARTESIAN_POINT ( 'NONE',  ( 80.80454364895454944, 63.02910633771584514, -3.452358620554643487 ) ) ;
#11236 = CYLINDRICAL_SURFACE ( 'NONE', #24131, 0.1000000000000028644 ) ;
#11237 = CARTESIAN_POINT ( 'NONE',  ( 2.315891445417157524, -26.13011841296867033, 7.773839561854632763 ) ) ;
#11238 = CARTESIAN_POINT ( 'NONE',  ( -0.6902601390570299866, -32.12625400224952443, 6.980586498568965403 ) ) ;
#11239 = EDGE_LOOP ( 'NONE', ( #9211, #29354, #36083, #39937 ) ) ;
#11240 = CARTESIAN_POINT ( 'NONE',  ( -1.722830152274906990, -28.84121352662702975, 7.753200566781598191 ) ) ;
#11241 = ORIENTED_EDGE ( 'NONE', *, *, #5011, .F. ) ;
#11242 = ORIENTED_EDGE ( 'NONE', *, *, #2862, .T. ) ;
#11243 = CARTESIAN_POINT ( 'NONE',  ( 79.33915194569547680, 65.11111034845936274, -3.233326467035622098 ) ) ;
#11244 = CARTESIAN_POINT ( 'NONE',  ( -60.81661347076553881, 25.20155461598434954, -8.800414904976364028 ) ) ;
#11245 = CARTESIAN_POINT ( 'NONE',  ( 81.07324312733541660, 61.26878263851436657, 1.298998371267757745 ) ) ;
#11246 = CARTESIAN_POINT ( 'NONE',  ( 23.56014592707593280, 1.105608511620937984, 5.220594937748640696 ) ) ;
#11248 = ORIENTED_EDGE ( 'NONE', *, *, #13033, .F. ) ;
#11247 = CARTESIAN_POINT ( 'NONE',  ( -0.7896860208805611681, -27.25486626507048271, 6.882085323592686876 ) ) ;
#11249 = CARTESIAN_POINT ( 'NONE',  ( 75.87451422959399849, 60.69085731309660758, -3.756674307851894490 ) ) ;
#11250 = CARTESIAN_POINT ( 'NONE',  ( 3.319000845420424284, -32.55994614210599991, 6.866852738645442322 ) ) ;
#11252 = LINE ( 'NONE', #20736, #20978 ) ;
#11251 = CARTESIAN_POINT ( 'NONE',  ( 0.4695943777967593880, -26.29347754267606874, 7.695279973900954751 ) ) ;
#11253 = CARTESIAN_POINT ( 'NONE',  ( -1.238510913153971771, -27.86027243158510558, 7.775108481317160702 ) ) ;
#11254 = CARTESIAN_POINT ( 'NONE',  ( 4.662410371202409642, -31.23919232437170734, 7.680992449362115337 ) ) ;
#11255 = EDGE_CURVE ( 'NONE', #17262, #17544, #37526, .T. ) ;
#11256 = CARTESIAN_POINT ( 'NONE',  ( 23.15910336873031738, 3.906749609004425139, -3.275810519260066389 ) ) ;
#11257 = ORIENTED_EDGE ( 'NONE', *, *, #39213, .T. ) ;
#11258 = CARTESIAN_POINT ( 'NONE',  ( 4.401417849205680355, -27.34407100962124559, 6.894806418505347700 ) ) ;
#11259 = CARTESIAN_POINT ( 'NONE',  ( 21.85643539959778181, 8.766930670454163632, 4.215001190429523703 ) ) ;
#11260 = B_SPLINE_CURVE_WITH_KNOTS ( 'NONE', 3,
 ( #27983, #35208, #9448, #28606, #2903, #15422, #24911, #37446, #415, #6174 ),
 .UNSPECIFIED., .F., .F.,
 ( 4, 3, 3, 4 ),
 ( 0.0001585009270395677274, 0.0001815657551981809145, 0.0002118214035944089005, 0.0002170292169044720702 ),
 .UNSPECIFIED. ) ;
#11261 = CARTESIAN_POINT ( 'NONE',  ( 21.88097534389255472, 3.372061099796740180, -3.393279653742926172 ) ) ;
#11262 = CARTESIAN_POINT ( 'NONE',  ( 2.890832430579337142, -32.75471385602386931, 7.661510568013097711 ) ) ;
#11263 = CARTESIAN_POINT ( 'NONE',  ( 0.000000000000000000, -0.5999999999999994227, -4.250000000000000000 ) ) ;
#11264 = CARTESIAN_POINT ( 'NONE',  ( 78.99802787997056441, 66.11506539533188231, 1.704083397384887233 ) ) ;
#11265 = CARTESIAN_POINT ( 'NONE',  ( 85.43170627155664931, 2.122511629702291902, -4.702826977918449280 ) ) ;
#11266 =( BOUNDED_CURVE ( )  B_SPLINE_CURVE ( 3, ( #19884, #25465, #25869, #32456 ),
 .UNSPECIFIED., .F., .T. ) 
 B_SPLINE_CURVE_WITH_KNOTS ( ( 4, 4 ),
 ( 4.708531083176465515, 4.895802057644186966 ),
 .UNSPECIFIED. ) 
 CURVE ( )  GEOMETRIC_REPRESENTATION_ITEM ( )  RATIONAL_B_SPLINE_CURVE ( ( 1.000000000000000000, 0.9970795998553221295, 0.9970795998553221295, 1.000000000000000000 ) ) 
 REPRESENTATION_ITEM ( '' )  );
#11267 = DIRECTION ( 'NONE',  ( -1.000000000000000000, 0.000000000000000000, 0.000000000000000000 ) ) ;
#11268 = ORIENTED_EDGE ( 'NONE', *, *, #6491, .F. ) ;
#11269 = CARTESIAN_POINT ( 'NONE',  ( -0.6763298692248193023, -32.13921067023287037, 7.013842709614101167 ) ) ;
#11270 = EDGE_CURVE ( 'NONE', #24116, #30761, #5472, .T. ) ;
#11271 = DIRECTION ( 'NONE',  ( 0.000000000000000000, 0.6834397476448867970, -0.7300069255418700775 ) ) ;
#11272 = CARTESIAN_POINT ( 'NONE',  ( 19.69748393801550534, -3.013861005515011904, -3.228077426689117235 ) ) ;
#11273 = CARTESIAN_POINT ( 'NONE',  ( 36.89660107519480903, -3.000806692559368383, -5.965004964089976269 ) ) ;
#11274 = CARTESIAN_POINT ( 'NONE',  ( 14.69558838330753581, -65.19654454972992141, -2.500000000000000444 ) ) ;
#11275 = CIRCLE ( 'NONE', #21834, 21.28220113893567245 ) ;
#11276 = CARTESIAN_POINT ( 'NONE',  ( 24.64884766327626053, 0.7497537406995623543, -4.794175230417015321 ) ) ;
#11277 = CARTESIAN_POINT ( 'NONE',  ( 1.700390093233090871, -29.56993018339339940, 7.750000000000000888 ) ) ;
#11278 = ORIENTED_EDGE ( 'NONE', *, *, #27568, .F. ) ;
#11279 = CARTESIAN_POINT ( 'NONE',  ( 20.42173045687939137, 3.659900802137024733, 3.393702957850269541 ) ) ;
#11280 = CARTESIAN_POINT ( 'NONE',  ( 30.19238557334687911, -2.952639005720375742, -4.918649992961978690 ) ) ;
#11281 = EDGE_CURVE ( 'NONE', #4923, #40423, #9091, .T. ) ;
#11282 = EDGE_LOOP ( 'NONE', ( #30468, #21596, #17429, #1068, #32900, #16045, #12939 ) ) ;
#11283 = ORIENTED_EDGE ( 'NONE', *, *, #1940, .F. ) ;
#11284 = CARTESIAN_POINT ( 'NONE',  ( 27.81753993201519393, 1.846270399565714371, 3.902048507340946326 ) ) ;
#11285 = CARTESIAN_POINT ( 'NONE',  ( -0.5344885137010326748, -32.26349986176969509, 7.643192810543824045 ) ) ;
#11286 = CARTESIAN_POINT ( 'NONE',  ( 3.476044783818678763, -32.58606316010092030, 7.660770905198780234 ) ) ;
#11287 = VECTOR ( 'NONE', #10347, 1000.000000000000000 ) ;
#11288 = ORIENTED_EDGE ( 'NONE', *, *, #1148, .T. ) ;
#11289 = DIRECTION ( 'NONE',  ( -0.000000000000000000, -1.000000000000000000, 0.000000000000000000 ) ) ;
#11290 = ORIENTED_EDGE ( 'NONE', *, *, #27383, .F. ) ;
#11291 = ORIENTED_EDGE ( 'NONE', *, *, #3623, .T. ) ;
#11292 = DIRECTION ( 'NONE',  ( -0.000000000000000000, -0.000000000000000000, 1.000000000000000000 ) ) ;
#11293 = ORIENTED_EDGE ( 'NONE', *, *, #5581, .T. ) ;
#11294 = CARTESIAN_POINT ( 'NONE',  ( 14.75726152236038935, -4.580480956772500889, 2.509421305520750600 ) ) ;
#11295 = PLANE ( 'NONE',  #6122 ) ;
#11296 = ORIENTED_EDGE ( 'NONE', *, *, #32884, .F. ) ;
#11297 = CARTESIAN_POINT ( 'NONE',  ( 22.52624294278324157, 4.322728351962980220, 3.478153892842317241 ) ) ;
#11298 = CARTESIAN_POINT ( 'NONE',  ( 82.09872185058162586, 62.41535711090991612, -1.944145319385669923 ) ) ;
#11299 = ADVANCED_FACE ( 'NONE', ( #11826 ), #24409, .F. ) ;
#11300 = FACE_OUTER_BOUND ( 'NONE', #14707, .T. ) ;
#11301 = VERTEX_POINT ( 'NONE', #18424 ) ;
#11303 = CARTESIAN_POINT ( 'NONE',  ( 26.16692636534402538, -2.761581989583650198, -4.290379727454292080 ) ) ;
#11302 = PLANE ( 'NONE',  #3590 ) ;
#11304 = CARTESIAN_POINT ( 'NONE',  ( -6.348748702180634140, -26.64985754041175525, 6.800000000000000711 ) ) ;
#11305 = CARTESIAN_POINT ( 'NONE',  ( 74.04982613775094080, 61.68561850464361385, 3.815996826674513009 ) ) ;
#11306 = VERTEX_POINT ( 'NONE', #40248 ) ;
#11307 = CARTESIAN_POINT ( 'NONE',  ( 22.04746162069255533, 2.900181437439750542, -4.981729368850734474 ) ) ;
#11308 = ORIENTED_EDGE ( 'NONE', *, *, #15419, .F. ) ;
#11309 = CARTESIAN_POINT ( 'NONE',  ( -8.348748702180635917, -25.49307895267003587, 6.700000000000000178 ) ) ;
#11310 = CARTESIAN_POINT ( 'NONE',  ( -55.16612787639762416, 31.23053227951969646, -1.484562114140327793 ) ) ;
#11311 = DIRECTION ( 'NONE',  ( 0.000000000000000000, -0.000000000000000000, 1.000000000000000000 ) ) ;
#11312 = DIRECTION ( 'NONE',  ( 1.000000000000000000, 0.000000000000000000, 0.000000000000000000 ) ) ;
#11313 = CARTESIAN_POINT ( 'NONE',  ( -69.08758708074093136, 36.88538962427717394, 8.800414904976364028 ) ) ;
#11314 = CARTESIAN_POINT ( 'NONE',  ( 81.16673370561990453, 65.10603640127602887, 2.903340743335354190 ) ) ;
#11315 = CARTESIAN_POINT ( 'NONE',  ( 86.40868413783579172, 1.299389369533768379, 4.865112849554557251 ) ) ;
#11316 = B_SPLINE_CURVE_WITH_KNOTS ( 'NONE', 3,
 ( #7654, #10530, #3988, #35477, #20007, #16509, #29085, #888, #38531, #10337, #1491, #22909, #7249, #23110, #20205, #4182, #16699, #29284, #32587, #1098, #4384, #29488, #4580, #17107, #27602 ),
 .UNSPECIFIED., .F., .F.,
 ( 4, 3, 3, 3, 3, 3, 3, 3, 4 ),
 ( 6.468151674593758404E-05, 9.076621574722010212E-05, 0.0001210204262067969094, 0.0001512763324577425894, 0.0001815301820994201292, 0.0002117781465860718712, 0.0002420274594459749366, 0.0002722905548971152464, 0.0002816827545175596011 ),
 .UNSPECIFIED. ) ;
#11317 = CARTESIAN_POINT ( 'NONE',  ( 31.44014676667174157, -3.103618331322294921, 5.406754918213918515 ) ) ;
#11318 = EDGE_CURVE ( 'NONE', #33929, #37233, #27692, .T. ) ;
#11319 = EDGE_CURVE ( 'NONE', #17881, #31037, #1661, .T. ) ;
#11320 = CIRCLE ( 'NONE', #6770, 1.000000000000000666 ) ;
#11321 = EDGE_CURVE ( 'NONE', #1511, #36985, #16568, .T. ) ;
#11322 = DIRECTION ( 'NONE',  ( -0.000000000000000000, -0.000000000000000000, -1.000000000000000000 ) ) ;
#11323 = CARTESIAN_POINT ( 'NONE',  ( 0.5834512725888432172, -26.35863018636138122, 6.894806418505347700 ) ) ;
#11324 = DIRECTION ( 'NONE',  ( 1.000000000000000000, 0.000000000000000000, 0.000000000000000000 ) ) ;
#11325 = CARTESIAN_POINT ( 'NONE',  ( 36.68769143235972763, -2.387623739369580722, -5.932399561826603218 ) ) ;
#11326 = PLANE ( 'NONE',  #3658 ) ;
#11327 = PLANE ( 'NONE',  #19367 ) ;
#11328 = FACE_BOUND ( 'NONE', #27312, .T. ) ;
#11329 = CARTESIAN_POINT ( 'NONE',  ( 4.348731362533842848, -31.83831163058102476, 7.783750581861601070 ) ) ;
#11330 = DIRECTION ( 'NONE',  ( 0.3420201433256790380, -0.9396926207859046531, -0.000000000000000000 ) ) ;
#11331 = ADVANCED_FACE ( 'NONE', ( #19055 ), #22364, .T. ) ;
#11332 = ORIENTED_EDGE ( 'NONE', *, *, #40292, .F. ) ;
#11333 = CARTESIAN_POINT ( 'NONE',  ( 27.74721017235163600, 1.752453911456003599, 4.134717658254572825 ) ) ;
#11334 = CARTESIAN_POINT ( 'NONE',  ( -69.94741522153590552, -0.5593530815884721896, 3.919381273429904944 ) ) ;
#11335 = CARTESIAN_POINT ( 'NONE',  ( 67.17808119270118539, 57.98628055940345405, -3.998197261021421589 ) ) ;
#11336 = CARTESIAN_POINT ( 'NONE',  ( 4.299742401097503830, -31.91372402269596620, 7.751599049952198506 ) ) ;
#11337 = CARTESIAN_POINT ( 'NONE',  ( -62.92837670882106238, -23.80776546975053520, 6.000000000000000000 ) ) ;
#11338 = VERTEX_POINT ( 'NONE', #19460 ) ;
#11339 = PLANE ( 'NONE',  #30523 ) ;
#11340 = DIRECTION ( 'NONE',  ( 1.000000000000000000, 0.000000000000000000, 0.000000000000000000 ) ) ;
#11341 = CARTESIAN_POINT ( 'NONE',  ( 85.67826002946482333, 0.8418862626009593342, -5.872190610739490779 ) ) ;
#11342 = LINE ( 'NONE', #34595, #35371 ) ;
#11343 = CARTESIAN_POINT ( 'NONE',  ( 0.3285059592769975501, -32.78986077462409554, 6.925313231306332362 ) ) ;
#11344 = VECTOR ( 'NONE', #24239, 999.9999999999998863 ) ;
#11345 = CARTESIAN_POINT ( 'NONE',  ( -12.24874870218063627, -26.64985754041175525, 6.800000000000000711 ) ) ;
#11346 = VERTEX_POINT ( 'NONE', #31824 ) ;
#11347 = CARTESIAN_POINT ( 'NONE',  ( 21.83642765803570995, 5.927067409592997826, 3.151569157035945867 ) ) ;
#11348 = CARTESIAN_POINT ( 'NONE',  ( 80.71704827558885142, 66.21292280724347279, -1.118100487915077546 ) ) ;
#11349 = ADVANCED_FACE ( 'NONE', ( #6507 ), #539, .F. ) ;
#11350 = CARTESIAN_POINT ( 'NONE',  ( 81.12869333199854793, 61.28902183752150279, 1.194943971655654691 ) ) ;
#11351 = FACE_OUTER_BOUND ( 'NONE', #656, .T. ) ;
#11352 = ORIENTED_EDGE ( 'NONE', *, *, #38162, .T. ) ;
#11353 = CARTESIAN_POINT ( 'NONE',  ( 77.76298154960852571, 62.57953843473561051, -3.839379600940507675 ) ) ;
#11355 = CARTESIAN_POINT ( 'NONE',  ( 2.255447537765926658, -26.21554331940935967, 7.691066658568947112 ) ) ;
#11354 = CARTESIAN_POINT ( 'NONE',  ( 21.73387441235908923, 0.2123480426500482521, 9.115313740638288920 ) ) ;
#11356 = CARTESIAN_POINT ( 'NONE',  ( 81.42847900441161357, 61.86412877313428993, -2.316472630215918205 ) ) ;
#11357 = CARTESIAN_POINT ( 'NONE',  ( 78.73442292448851276, 62.77418112150555629, 3.804514705604325364 ) ) ;
#11358 = ORIENTED_EDGE ( 'NONE', *, *, #19977, .T. ) ;
#11359 = EDGE_LOOP ( 'NONE', ( #2070, #33150, #28746, #36826 ) ) ;
#11360 = ADVANCED_FACE ( 'NONE', ( #25237 ), #35332, .T. ) ;
#11361 = CARTESIAN_POINT ( 'NONE',  ( 36.31056033868917154, -3.612627279154186244, -5.748865049962640583 ) ) ;
#11362 = ADVANCED_FACE ( 'NONE', ( #37567 ), #3638, .T. ) ;
#11363 = CARTESIAN_POINT ( 'NONE',  ( 82.50803812506910617, 63.51743744066186537, 1.680016503630071600 ) ) ;
#11365 = CARTESIAN_POINT ( 'NONE',  ( 14.69558838330753936, -3.003688195628454238, 6.000000000000001776 ) ) ;
#11364 = FACE_OUTER_BOUND ( 'NONE', #27578, .T. ) ;
#11366 = CARTESIAN_POINT ( 'NONE',  ( 28.10280119166142399, -0.8120181649793116740, 6.074162340139093175 ) ) ;
#11367 = LINE ( 'NONE', #17957, #23381 ) ;
#11368 = FACE_OUTER_BOUND ( 'NONE', #36103, .T. ) ;
#11369 = ORIENTED_EDGE ( 'NONE', *, *, #10903, .F. ) ;
#11370 = CYLINDRICAL_SURFACE ( 'NONE', #36674, 0.09010775117052916006 ) ;
#11371 = CARTESIAN_POINT ( 'NONE',  ( 21.97527673563478956, 0.2261748271463902005, -7.720852451735783717 ) ) ;
#11372 = EDGE_CURVE ( 'NONE', #12118, #1128, #30807, .T. ) ;
#11373 = CARTESIAN_POINT ( 'NONE',  ( 0.5657570339504449652, -32.78255583154504649, 7.257242401810563237 ) ) ;
#11374 = ORIENTED_EDGE ( 'NONE', *, *, #19392, .T. ) ;
#11375 = CARTESIAN_POINT ( 'NONE',  ( 5.001387658970600114, -30.73329387158167947, 7.700536657684216024 ) ) ;
#11376 = DIRECTION ( 'NONE',  ( 1.000000000000000000, 0.000000000000000000, 0.000000000000000000 ) ) ;
#11377 = CARTESIAN_POINT ( 'NONE',  ( 5.149693937723391457, -30.16348207664124814, 7.636816916992231974 ) ) ;
#11378 = CARTESIAN_POINT ( 'NONE',  ( 35.21965174470370386, -1.049964233957617177, -5.413429237120623405 ) ) ;
#11379 = DIRECTION ( 'NONE',  ( -1.000000000000000000, -0.000000000000000000, -0.000000000000000000 ) ) ;
#11380 = CARTESIAN_POINT ( 'NONE',  ( 4.821338062315135176, -33.56355840650683575, 6.954324564059724878 ) ) ;
#11381 = CARTESIAN_POINT ( 'NONE',  ( -71.59512852109486403, -48.46428640673855170, 5.963535602158745341 ) ) ;
#11382 = CARTESIAN_POINT ( 'NONE',  ( 2.735039440433452818, -32.80869545011542954, 6.865312560952602894 ) ) ;
#11383 = CARTESIAN_POINT ( 'NONE',  ( 5.100040579096636328, -29.61868030101130245, 6.894806418505348589 ) ) ;
#11384 = LINE ( 'NONE', #23564, #22428 ) ;
#11385 = ORIENTED_EDGE ( 'NONE', *, *, #1083, .T. ) ;
#11386 = CARTESIAN_POINT ( 'NONE',  ( 66.41110252083142029, 57.82170748331523669, 4.000000000000023981 ) ) ;
#11387 = CARTESIAN_POINT ( 'NONE',  ( 72.42208042952545100, 59.16915255968121556, -3.823636340456165073 ) ) ;
#11388 = AXIS2_PLACEMENT_3D ( 'NONE', #9784, #10388, #35724 ) ;
#11389 = ORIENTED_EDGE ( 'NONE', *, *, #8451, .F. ) ;
#11390 = LINE ( 'NONE', #1971, #19962 ) ;
#11391 = DIRECTION ( 'NONE',  ( -0.000000000000000000, -0.000000000000000000, 1.000000000000000000 ) ) ;
#11392 = CARTESIAN_POINT ( 'NONE',  ( -1.656077431862442717, -30.11226380117775037, 6.894806418505347700 ) ) ;
#11393 = ORIENTED_EDGE ( 'NONE', *, *, #39302, .F. ) ;
#11394 = DIRECTION ( 'NONE',  ( -0.000000000000000000, -0.000000000000000000, 1.000000000000000000 ) ) ;
#11395 = ITEM_DEFINED_TRANSFORMATION ( 'NONE', 'NONE', #22224,  #30744 ) ;
#11396 = CARTESIAN_POINT ( 'NONE',  ( -0.5730865926811068434, -32.23100210249002373, 6.894806418505347700 ) ) ;
#11397 = ORIENTED_EDGE ( 'NONE', *, *, #14574, .F. ) ;
#11398 = DIRECTION ( 'NONE',  ( 1.000000000000000000, 0.000000000000000000, 0.000000000000000000 ) ) ;
#11399 = CARTESIAN_POINT ( 'NONE',  ( -25.07867591359219617, -26.64985754041175525, 6.700000000000000178 ) ) ;
#11400 = EDGE_CURVE ( 'NONE', #4251, #36906, #15958, .T. ) ;
#11401 = ORIENTED_EDGE ( 'NONE', *, *, #6381, .T. ) ;
#11402 = CARTESIAN_POINT ( 'NONE',  ( 80.76516742887832834, 61.34548671587045732, -2.174061886842025171 ) ) ;
#11403 = CARTESIAN_POINT ( 'NONE',  ( 17.73032643950705989, 9.401816356539047348, -2.499999999999722888 ) ) ;
#11404 = CARTESIAN_POINT ( 'NONE',  ( 80.83921286824487140, 61.18398161863572682, 1.552792442904345815 ) ) ;
#11405 = VERTEX_POINT ( 'NONE', #13075 ) ;
#11406 = EDGE_CURVE ( 'NONE', #22430, #6673, #37014, .T. ) ;
#11407 = LINE ( 'NONE', #8734, #10038 ) ;
#11408 = ADVANCED_FACE ( 'NONE', ( #30141 ), #32430, .F. ) ;
#11409 = CARTESIAN_POINT ( 'NONE',  ( 4.040371955156762063, -27.10325224939195721, 6.979335674598004857 ) ) ;
#11410 = CARTESIAN_POINT ( 'NONE',  ( 18.59223163685811997, 13.14295818854019871, 2.500000000000000444 ) ) ;
#11411 = CARTESIAN_POINT ( 'NONE',  ( 21.85643539959779957, 4.362886173974390935, 14.46802226367788791 ) ) ;
#11412 = VERTEX_POINT ( 'NONE', #38580 ) ;
#11413 = CARTESIAN_POINT ( 'NONE',  ( -79.95320165109795596, 10.45477653335570878, 6.473989127779994135 ) ) ;
#11414 = EDGE_CURVE ( 'NONE', #24169, #27368, #16320, .T. ) ;
#11415 = CARTESIAN_POINT ( 'NONE',  ( 14.77222419049203594, -4.492314308407749479, 2.511960871155140218 ) ) ;
#11416 = CIRCLE ( 'NONE', #12069, 0.1000000000000028644 ) ;
#11417 = AXIS2_PLACEMENT_3D ( 'NONE', #23282, #16675, #22887 ) ;
#11418 = EDGE_CURVE ( 'NONE', #34241, #6781, #4628, .T. ) ;
#11419 = CARTESIAN_POINT ( 'NONE',  ( -80.20725398478467127, 11.50953281160756347, -3.750582765600833923 ) ) ;
#11420 = CARTESIAN_POINT ( 'NONE',  ( -63.70768058868311812, 44.39675795731061214, 4.000000000000000000 ) ) ;
#11421 = CARTESIAN_POINT ( 'NONE',  ( 2.496911866804199409, -26.26454769719600080, 6.949473656533219135 ) ) ;
#11422 = DIRECTION ( 'NONE',  ( -0.000000000000000000, 1.000000000000000000, -0.000000000000000000 ) ) ;
#11423 = CARTESIAN_POINT ( 'NONE',  ( 3.866898022442308847, -26.94957171677655339, 7.740055089680397238 ) ) ;
#11424 = DIRECTION ( 'NONE',  ( -0.000000000000000000, -0.000000000000000000, 1.000000000000000000 ) ) ;
#11425 = CARTESIAN_POINT ( 'NONE',  ( -1.219418532703906877, -27.82788610016705988, 6.894806418505346812 ) ) ;
#11426 = CIRCLE ( 'NONE', #39027, 0.1000000000000028644 ) ;
#11427 = CARTESIAN_POINT ( 'NONE',  ( 0.1825688514504736348, 0.000000000000000000, 0.000000000000000000 ) ) ;
#11428 = CARTESIAN_POINT ( 'NONE',  ( -0.4435737903242095159, -26.93109965651677129, 6.889465824494255486 ) ) ;
#11429 = DIRECTION ( 'NONE',  ( -0.000000000000000000, -0.000000000000000000, 1.000000000000000000 ) ) ;
#11430 = CIRCLE ( 'NONE', #7512, 0.1000000000000028644 ) ;
#11431 = VERTEX_POINT ( 'NONE', #4226 ) ;
#11432 = CARTESIAN_POINT ( 'NONE',  ( 67.39181666045010388, 58.30934502646129403, 3.993945454764281422 ) ) ;
#11433 = CARTESIAN_POINT ( 'NONE',  ( 36.42662174935294672, -3.159887864482101794, 5.891653323799407538 ) ) ;
#11434 = DIRECTION ( 'NONE',  ( -0.000000000000000000, 1.000000000000000000, -0.000000000000000000 ) ) ;
#11435 = CARTESIAN_POINT ( 'NONE',  ( 87.69705646362149309, -0.3167607505441215610, 5.204154330927820205 ) ) ;
#11437 = LINE ( 'NONE', #27105, #15839 ) ;
#11436 = CARTESIAN_POINT ( 'NONE',  ( 32.92332271219583362, -2.910100397871670186, 5.759571882993297365 ) ) ;
#11438 = CARTESIAN_POINT ( 'NONE',  ( -1.605260786948502494, -28.77451848735744377, 6.939395833800443114 ) ) ;
#11439 = CARTESIAN_POINT ( 'NONE',  ( -58.91453996558632156, 28.99622802882459638, 6.206785453512805972 ) ) ;
#11440 = LINE ( 'NONE', #2640, #21991 ) ;
#11441 = ORIENTED_EDGE ( 'NONE', *, *, #4528, .T. ) ;
#11442 = CARTESIAN_POINT ( 'NONE',  ( -71.36981149190343388, -21.68728802194536698, 5.996540489601002832 ) ) ;
#11443 = VECTOR ( 'NONE', #29689, 1000.000000000000000 ) ;
#11444 = ORIENTED_EDGE ( 'NONE', *, *, #3588, .T. ) ;
#11445 = CARTESIAN_POINT ( 'NONE',  ( 81.01114204962451026, 61.40637449960411942, -2.012706562768916907 ) ) ;
#11446 = CARTESIAN_POINT ( 'NONE',  ( 3.293813124479239018, -32.57342865076346783, 7.754798119455333705 ) ) ;
#11447 = PRODUCT_DEFINITION ( 'UNKNOWN', '', #29440, #18451 ) ;
#11448 = CARTESIAN_POINT ( 'NONE',  ( 81.02780191652733777, 61.56951766280584337, 2.259810845156954517 ) ) ;
#11449 = CARTESIAN_POINT ( 'NONE',  ( 22.73568268706182849, 0.4048558432997723111, 6.305629274227928960 ) ) ;
#11451 = ORIENTED_EDGE ( 'NONE', *, *, #23204, .F. ) ;
#11450 = DIRECTION ( 'NONE',  ( 0.000000000000000000, 0.000000000000000000, 1.000000000000000000 ) ) ;
#11452 = VECTOR ( 'NONE', #21846, 1000.000000000000000 ) ;
#11453 = CARTESIAN_POINT ( 'NONE',  ( 74.08781496033066105, 60.06802034872734453, -3.841642203975295544 ) ) ;
#11454 = CARTESIAN_POINT ( 'NONE',  ( -69.92837670882109080, -20.91528719346852583, 5.916079783099622347 ) ) ;
#11456 = DIRECTION ( 'NONE',  ( -1.000000000000000000, 0.000000000000000000, 0.000000000000000000 ) ) ;
#11455 = CARTESIAN_POINT ( 'NONE',  ( 5.001438667734867671, -30.73314912614656436, 7.695279973900954751 ) ) ;
#11457 = LINE ( 'NONE', #20950, #22504 ) ;
#11458 = CARTESIAN_POINT ( 'NONE',  ( -38.34874870218063592, -25.49307895267003587, 6.700000000000000178 ) ) ;
#11459 = CARTESIAN_POINT ( 'NONE',  ( 24.03489882237598252, 3.326192361758713467, -3.293071421972179724 ) ) ;
#11460 = ORIENTED_EDGE ( 'NONE', *, *, #34112, .F. ) ;
#11461 = DIRECTION ( 'NONE',  ( 0.000000000000000000, 0.000000000000000000, 1.000000000000000000 ) ) ;
#11462 = EDGE_CURVE ( 'NONE', #40258, #6329, #32122, .T. ) ;
#11463 = CARTESIAN_POINT ( 'NONE',  ( 22.80949115205394406, -6.484386712482024251, -3.653976874014524867 ) ) ;
#11465 = EDGE_CURVE ( 'NONE', #31687, #15032, #16987, .T. ) ;
#11464 = CARTESIAN_POINT ( 'NONE',  ( 21.87484035781776726, 3.535422555137202494, -3.391095861098737174 ) ) ;
#11466 = CARTESIAN_POINT ( 'NONE',  ( 35.94200923520244828, 151.3264224549853907, -1.000000000000000000 ) ) ;
#11467 = CARTESIAN_POINT ( 'NONE',  ( 1.098862567954408842, -33.01645833599632596, 7.762796336881262249 ) ) ;
#11468 = CARTESIAN_POINT ( 'NONE',  ( 79.22754343383607534, 66.08014515007958778, 1.953285432047549230 ) ) ;
#11469 = CARTESIAN_POINT ( 'NONE',  ( 84.96877181165257298, 2.299433286287765554, -4.273906790846864645 ) ) ;
#11470 = FACE_OUTER_BOUND ( 'NONE', #10048, .T. ) ;
#11471 = ORIENTED_EDGE ( 'NONE', *, *, #16119, .F. ) ;
#11472 = CARTESIAN_POINT ( 'NONE',  ( 1.700390093233090871, -29.56993018339339940, 7.800000000000000711 ) ) ;
#11473 = B_SPLINE_CURVE_WITH_KNOTS ( 'NONE', 3,
 ( #25747, #16467, #26157, #13374, #19573, #21390, #17450, #14781, #8605, #21183, #11080, #2256, #33965, #33137, #2473, #27350, #36217, #20976, #14572 ),
 .UNSPECIFIED., .F., .F.,
 ( 4, 3, 3, 3, 3, 3, 4 ),
 ( 4.336808689942017736E-19, 2.546128104244632296E-05, 5.711050680483876455E-05, 8.113074941675923069E-05, 0.0001053129305727100597, 0.0001360598016347191693, 0.0001612931755713715575 ),
 .UNSPECIFIED. ) ;
#11474 = EDGE_LOOP ( 'NONE', ( #22917, #6757 ) ) ;
#11475 = MECHANICAL_DESIGN_GEOMETRIC_PRESENTATION_REPRESENTATION (  '', ( #31237 ), #12133 ) ;
#11476 = VECTOR ( 'NONE', #34368, 1000.000000000000000 ) ;
#11477 = DIRECTION ( 'NONE',  ( -0.000000000000000000, -0.000000000000000000, -1.000000000000000000 ) ) ;
#11478 = CARTESIAN_POINT ( 'NONE',  ( 17.05638849885697894, -3.260855927369440188, -2.842766561921666213 ) ) ;
#11479 = DIRECTION ( 'NONE',  ( 0.000000000000000000, 0.000000000000000000, 1.000000000000000000 ) ) ;
#11480 = LINE ( 'NONE', #36819, #20080 ) ;
#11481 = VECTOR ( 'NONE', #38736, 1000.000000000000000 ) ;
#11482 = CARTESIAN_POINT ( 'NONE',  ( 24.59788967097932044, 0.8378664169005234363, -4.794031594194660961 ) ) ;
#11483 = CARTESIAN_POINT ( 'NONE',  ( 1.910837266068588836, -26.17644932986278050, 6.949473656533215582 ) ) ;
#11484 = ORIENTED_EDGE ( 'NONE', *, *, #36133, .F. ) ;
#11485 = CARTESIAN_POINT ( 'NONE',  ( 35.45221327798894606, -1.918015286137918052, 5.739573315685131405 ) ) ;
#11486 = AXIS2_PLACEMENT_3D ( 'NONE', #22983, #19484, #19685 ) ;
#11487 = CARTESIAN_POINT ( 'NONE',  ( 31.86443645673159963, -2.967394441500424751, -5.179613972017589774 ) ) ;
#11488 = ORIENTED_EDGE ( 'NONE', *, *, #29842, .F. ) ;
#11489 = ORIENTED_EDGE ( 'NONE', *, *, #22423, .F. ) ;
#11491 = CARTESIAN_POINT ( 'NONE',  ( 33.11469321899686236, -0.1493061854001800637, 4.939395549459463908 ) ) ;
#11490 = CARTESIAN_POINT ( 'NONE',  ( 80.53345128649183948, 64.37995495044674499, -3.533418250979443176 ) ) ;
#11492 = CARTESIAN_POINT ( 'NONE',  ( 24.89998026755250393, -2.711650026429365479, 4.092642147686758491 ) ) ;
#11493 = DIRECTION ( 'NONE',  ( 1.000000000000000000, 0.000000000000000000, 0.000000000000000000 ) ) ;
#11494 = ORIENTED_EDGE ( 'NONE', *, *, #15663, .F. ) ;
#11495 = DIRECTION ( 'NONE',  ( -0.000000000000000000, -0.000000000000000000, 1.000000000000000000 ) ) ;
#11496 = VERTEX_POINT ( 'NONE', #20656 ) ;
#11497 = VERTEX_POINT ( 'NONE', #10978 ) ;
#11498 = DIRECTION ( 'NONE',  ( -0.7660444431189813441, 0.6427876096865353661, -0.000000000000000000 ) ) ;
#11499 = CARTESIAN_POINT ( 'NONE',  ( 81.19486284036338475, 61.45157923659408539, -1.862141363775748903 ) ) ;
#11500 = CARTESIAN_POINT ( 'NONE',  ( 14.74756118481574774, -5.100620622190623621, 2.500104659008372643 ) ) ;
#11501 = VERTEX_POINT ( 'NONE', #38788 ) ;
#11502 = CARTESIAN_POINT ( 'NONE',  ( -62.92837670882106238, -52.49535338866468948, -6.000000000000000000 ) ) ;
#11503 = ORIENTED_EDGE ( 'NONE', *, *, #34232, .F. ) ;
#11504 = CARTESIAN_POINT ( 'NONE',  ( 23.20559657321298275, 3.453218578186380672, 3.711049198623960432 ) ) ;
#11505 = CARTESIAN_POINT ( 'NONE',  ( 81.16810052477266879, 61.30343919788879248, -1.037317649801931863 ) ) ;
#11506 = ADVANCED_FACE ( 'NONE', ( #33030 ), #7702, .F. ) ;
#11507 = AXIS2_PLACEMENT_3D ( 'NONE', #38686, #29438, #4135 ) ;
#11508 = VECTOR ( 'NONE', #27528, 1000.000000000000000 ) ;
#11509 = CARTESIAN_POINT ( 'NONE',  ( 4.733915118986097958, -28.03444136281207832, 7.013842709614101167 ) ) ;
#11511 = CARTESIAN_POINT ( 'NONE',  ( 2.562099542307729738, -33.75548367670988625, 7.754798119455333705 ) ) ;
#11510 = FACE_OUTER_BOUND ( 'NONE', #30644, .T. ) ;
#11512 = CARTESIAN_POINT ( 'NONE',  ( -5.078675913592192614, -24.55319635012989110, 6.700000000000000178 ) ) ;
#11513 = CARTESIAN_POINT ( 'NONE',  ( 74.23991766213896426, 61.26593220986219279, 3.911020515999898528 ) ) ;
#11514 = CARTESIAN_POINT ( 'NONE',  ( 24.13946561501993671, 2.647771132776644887, -4.002951860888451563 ) ) ;
#11515 = CIRCLE ( 'NONE', #39817, 82.54614097552274643 ) ;
#11516 = PLANE ( 'NONE',  #7657 ) ;
#11518 = EDGE_CURVE ( 'NONE', #32758, #25288, #10416, .T. ) ;
#11517 = CARTESIAN_POINT ( 'NONE',  ( -51.01549048184568846, -38.28842912540938670, 6.800000000000000711 ) ) ;
#11519 = CARTESIAN_POINT ( 'NONE',  ( -62.99176104828779899, 35.53767314789729426, 6.181002566280151989 ) ) ;
#11520 = FACE_OUTER_BOUND ( 'NONE', #32645, .T. ) ;
#11521 = CARTESIAN_POINT ( 'NONE',  ( 81.94287803445145357, 63.22849810396159853, 2.713791510777069149 ) ) ;
#11522 = CARTESIAN_POINT ( 'NONE',  ( 87.74221684178165503, -0.1984978568185522818, 3.841619981418926244 ) ) ;
#11523 = CARTESIAN_POINT ( 'NONE',  ( 5.131593199136804451, -30.26047000558811106, 6.865554069792297653 ) ) ;
#11524 = CARTESIAN_POINT ( 'NONE',  ( -1.799609906766908463, -29.73166366038556419, 7.383456277641972321 ) ) ;
#11525 = DIRECTION ( 'NONE',  ( 0.000000000000000000, 0.6605219282605402364, 0.7508067542896625923 ) ) ;
#11526 = DIRECTION ( 'NONE',  ( 0.8660254037844452579, -0.4999999999999886202, 0.000000000000000000 ) ) ;
#11527 = CARTESIAN_POINT ( 'NONE',  ( 0.06039256278810246209, -26.47792186227242439, 6.867199677474203234 ) ) ;
#11528 = CARTESIAN_POINT ( 'NONE',  ( 36.64077810573005678, -3.117975142819385148, -5.925077602603106897 ) ) ;
#11529 = FILL_AREA_STYLE_COLOUR ( '', #25972 ) ;
#11530 = CARTESIAN_POINT ( 'NONE',  ( 4.637114349001293157, -31.47405327090299565, 6.998987538705429223 ) ) ;
#11531 = DIRECTION ( 'NONE',  ( -1.385724075720358314E-16, 1.000000000000000000, 0.000000000000000000 ) ) ;
#11532 = CARTESIAN_POINT ( 'NONE',  ( 4.326895721323773536, -31.86212065727518095, 7.784725160561909441 ) ) ;
#11533 = CIRCLE ( 'NONE', #30618, 6.406751979251626317 ) ;
#11534 = ORIENTED_EDGE ( 'NONE', *, *, #40244, .T. ) ;
#11535 = CARTESIAN_POINT ( 'NONE',  ( 34.57549087153120837, -0.8971447047965824817, 5.398446312640987621 ) ) ;
#11536 = CARTESIAN_POINT ( 'NONE',  ( 1.214349479236255247, -26.10391960397356925, 7.753200566781599967 ) ) ;
#11537 = ADVANCED_FACE ( 'NONE', ( #26845 ), #26049, .F. ) ;
#11538 = CARTESIAN_POINT ( 'NONE',  ( 66.98331017875999294, 58.06610265625960210, -3.998453671246410934 ) ) ;
#11539 = VECTOR ( 'NONE', #8035, 1000.000000000000000 ) ;
#11540 = CARTESIAN_POINT ( 'NONE',  ( -0.5626977249550375593, -26.90001753928526540, 7.750000000000002665 ) ) ;
#11541 = ORIENTED_EDGE ( 'NONE', *, *, #21102, .T. ) ;
#11542 = CARTESIAN_POINT ( 'NONE',  ( -0.1539201161049026934, -32.53808085965915353, 7.754798119455333705 ) ) ;
#11543 = LINE ( 'NONE', #6418, #20695 ) ;
#11544 = CYLINDRICAL_SURFACE ( 'NONE', #6406, 0.1000000000000028644 ) ;
#11545 = EDGE_CURVE ( 'NONE', #14078, #30463, #36319, .T. ) ;
#11546 = DIRECTION ( 'NONE',  ( 0.000000000000000000, 0.000000000000000000, -1.000000000000000000 ) ) ;
#11547 = CARTESIAN_POINT ( 'NONE',  ( -13.07867591359219617, -24.55319635012989110, 6.700000000000000178 ) ) ;
#11548 = VERTEX_POINT ( 'NONE', #4433 ) ;
#11549 = CARTESIAN_POINT ( 'NONE',  ( 23.73921823260045372, 3.555442417871877314, 3.202292173715798107 ) ) ;
#11550 = CARTESIAN_POINT ( 'NONE',  ( 82.35470118046110599, 62.54510421749741056, -1.103079483641125069 ) ) ;
#11551 = ADVANCED_FACE ( 'NONE', ( #29536, #11990 ), #5227, .F. ) ;
#11552 = CARTESIAN_POINT ( 'NONE',  ( 80.23319818986580287, 64.21721675003155383, 3.633989118465187129 ) ) ;
#11553 = CARTESIAN_POINT ( 'NONE',  ( -0.07136309058874676370, -32.47180727514232501, 6.870716933885665512 ) ) ;
#11554 = EDGE_LOOP ( 'NONE', ( #3609, #34169, #25102, #4622 ) ) ;
#11555 = CARTESIAN_POINT ( 'NONE',  ( 78.34663729941159716, 61.36874863982424699, -3.480716904142254986 ) ) ;
#11557 = CARTESIAN_POINT ( 'NONE',  ( 14.78182191374954080, -5.169433146903486431, -2.499999999999999556 ) ) ;
#11556 = CARTESIAN_POINT ( 'NONE',  ( 23.05624328173124482, 0.3494845576275186216, 5.956316157212953044 ) ) ;
#11558 = CARTESIAN_POINT ( 'NONE',  ( 79.72834705193074001, 65.67299761742589226, -2.773332820897498774 ) ) ;
#11559 = CARTESIAN_POINT ( 'NONE',  ( 79.02450826907198689, 62.91033389078318550, 3.791687334209853155 ) ) ;
#11560 = CARTESIAN_POINT ( 'NONE',  ( -0.9076542330089235611, -27.38860637533221976, 7.763628509615282169 ) ) ;
#11561 = ORIENTED_EDGE ( 'NONE', *, *, #37226, .F. ) ;
#11562 = EDGE_CURVE ( 'NONE', #25767, #38197, #37325, .T. ) ;
#11563 = CARTESIAN_POINT ( 'NONE',  ( 82.52664026313796342, 63.88931701666353291, 1.444831904608907092 ) ) ;
#11565 = DIRECTION ( 'NONE',  ( 0.1736481776669273336, 0.9848077530122085754, -0.000000000000000000 ) ) ;
#11564 = CARTESIAN_POINT ( 'NONE',  ( 3.389257957103017471, -26.61903871757985840, 7.756377446753170091 ) ) ;
#11566 = CARTESIAN_POINT ( 'NONE',  ( 26.73479038929921359, 2.133517298515754668, 4.055905576634827092 ) ) ;
#11567 = PRESENTATION_LAYER_ASSIGNMENT (  '', '', ( #2423 ) ) ;
#11568 = CARTESIAN_POINT ( 'NONE',  ( -70.92837670882107659, -0.7829914368874778541, 38.00000000000000711 ) ) ;
#11569 = CARTESIAN_POINT ( 'NONE',  ( -14.87867591359218977, -26.64985754041175525, 6.700000000000000178 ) ) ;
#11570 = ORIENTED_EDGE ( 'NONE', *, *, #6144, .T. ) ;
#11571 = CARTESIAN_POINT ( 'NONE',  ( -80.58722291995898956, -6.629895795999400931, 2.621518543355748854 ) ) ;
#11572 = CARTESIAN_POINT ( 'NONE',  ( 26.05452957851533924, 0.7951218899326391032, -4.421888884741046688 ) ) ;
#11573 = CARTESIAN_POINT ( 'NONE',  ( -0.5125101069461969194, -26.98863734761392053, 7.695279973900954751 ) ) ;
#11574 = FACE_OUTER_BOUND ( 'NONE', #29891, .T. ) ;
#11575 = CARTESIAN_POINT ( 'NONE',  ( 1.713892699967802136, -33.06990413752668445, 7.635761828346576685 ) ) ;
#11576 = CARTESIAN_POINT ( 'NONE',  ( 5.172816400818245341, -29.13145608706553702, 7.011627023500183853 ) ) ;
#11577 = CARTESIAN_POINT ( 'NONE',  ( -72.42837670882110501, -47.31541682994506459, 9.886859966642605357 ) ) ;
#11578 = CARTESIAN_POINT ( 'NONE',  ( 36.87014114482988703, -2.088717756108750212, -5.864854126680631552 ) ) ;
#11579 = CARTESIAN_POINT ( 'NONE',  ( 4.762748405565132792, -33.59738516060317437, 6.894806418505347700 ) ) ;
#11580 = CARTESIAN_POINT ( 'NONE',  ( 37.19747295490952155, -2.841588721108153415, -5.999818660317219887 ) ) ;
#11581 = DIRECTION ( 'NONE',  ( 1.000000000000000000, 0.000000000000000000, -0.000000000000000000 ) ) ;
#11582 = CARTESIAN_POINT ( 'NONE',  ( -72.23889801321112714, -47.87246752859122978, 5.855634630472075663 ) ) ;
#11583 = CARTESIAN_POINT ( 'NONE',  ( 2.666604916071043885, -32.82975288721481633, 6.979335674598003969 ) ) ;
#11584 = CARTESIAN_POINT ( 'NONE',  ( -20.87867591359218622, -26.64985754041175525, 6.800000000000000711 ) ) ;
#11585 = DIRECTION ( 'NONE',  ( 0.000000000000000000, 0.000000000000000000, 1.000000000000000000 ) ) ;
#11586 = EDGE_CURVE ( 'NONE', #22597, #9007, #40490, .T. ) ;
#11587 = CARTESIAN_POINT ( 'NONE',  ( 14.75256470577902057, -4.610397949049963806, -2.508547837535054725 ) ) ;
#11588 = CARTESIAN_POINT ( 'NONE',  ( 22.77766753872744232, 1.958428159634223231, -5.124684968651379791 ) ) ;
#11589 = ORIENTED_EDGE ( 'NONE', *, *, #30371, .T. ) ;
#11590 = CARTESIAN_POINT ( 'NONE',  ( 66.27376694608996388, 57.73522568913447373, 4.000000000000000000 ) ) ;
#11591 = CARTESIAN_POINT ( 'NONE',  ( 69.27779986746136842, 58.60568623525134768, -3.981537309218750487 ) ) ;
#11592 = EDGE_LOOP ( 'NONE', ( #27062, #28214, #21472, #17984, #7374 ) ) ;
#11593 = DIRECTION ( 'NONE',  ( 0.000000000000000000, 0.000000000000000000, 1.000000000000000000 ) ) ;
#11594 = CARTESIAN_POINT ( 'NONE',  ( 0.1365689545988542086, -26.55089741178066021, 6.871394612369935651 ) ) ;
#11595 = LINE ( 'NONE', #11796, #23505 ) ;
#11596 = EDGE_CURVE ( 'NONE', #11926, #8831, #6860, .T. ) ;
#11597 = AXIS2_PLACEMENT_3D ( 'NONE', #710, #22130, #28701 ) ;
#11598 = EDGE_CURVE ( 'NONE', #35091, #34454, #13716, .T. ) ;
#11599 = CARTESIAN_POINT ( 'NONE',  ( -68.19214907655110380, 40.83859674667183981, -4.000000000000000000 ) ) ;
#11600 = VECTOR ( 'NONE', #35764, 1000.000000000000000 ) ;
#11601 = CIRCLE ( 'NONE', #10962, 0.9999999999999983347 ) ;
#11602 = CARTESIAN_POINT ( 'NONE',  ( 2.172536372144526773, -32.93698858539566743, 7.757178535559533294 ) ) ;
#11603 = ORIENTED_EDGE ( 'NONE', *, *, #5785, .T. ) ;
#11604 = EDGE_CURVE ( 'NONE', #25139, #37682, #36716, .T. ) ;
#11605 = CARTESIAN_POINT ( 'NONE',  ( 3.651251297819360531, -25.49307895267003587, 6.700000000000000178 ) ) ;
#11606 = ORIENTED_EDGE ( 'NONE', *, *, #32006, .F. ) ;
#11607 = CARTESIAN_POINT ( 'NONE',  ( 78.83700374940842437, 65.31049604782703000, -2.918211652848219373 ) ) ;
#11608 = CARTESIAN_POINT ( 'NONE',  ( 15.80745346850759603, 8.002139515150915372, -3.484773916741293220 ) ) ;
#11609 = CARTESIAN_POINT ( 'NONE',  ( 81.52783586777042046, 64.51439989829013655, -2.952528780688971288 ) ) ;
#11610 = CARTESIAN_POINT ( 'NONE',  ( 80.67643653137164961, 61.85813826494483436, 2.902290250791176085 ) ) ;
#11611 = DIRECTION ( 'NONE',  ( -0.000000000000000000, -0.000000000000000000, 1.000000000000000000 ) ) ;
#11612 = LINE ( 'NONE', #8535, #28125 ) ;
#11613 = CARTESIAN_POINT ( 'NONE',  ( 21.85643539959781023, -11.34362525346678474, 8.214566034197922306 ) ) ;
#11614 = ORIENTED_EDGE ( 'NONE', *, *, #1421, .F. ) ;
#11615 = CARTESIAN_POINT ( 'NONE',  ( -79.67174074027452946, 11.50491621841984546, 4.869819349584945556 ) ) ;
#11616 = CARTESIAN_POINT ( 'NONE',  ( 14.68780169807769376, -4.611715951047749229, 2.499999999999924505 ) ) ;
#11617 = AXIS2_PLACEMENT_3D ( 'NONE', #10021, #35376, #985 ) ;
#11618 = CARTESIAN_POINT ( 'NONE',  ( -75.58662980897157979, 8.514659871459404172, -8.885563836102193136 ) ) ;
#11619 = CARTESIAN_POINT ( 'NONE',  ( -34.97867591359219830, -26.64985754041175525, 6.700000000000000178 ) ) ;
#11620 = CARTESIAN_POINT ( 'NONE',  ( -38.87867591359218977, -24.55319635012989110, 6.700000000000000178 ) ) ;
#11621 = CARTESIAN_POINT ( 'NONE',  ( -1.742489505018671725, -30.16803301939627602, 7.773839561854632763 ) ) ;
#11622 =( BOUNDED_CURVE ( )  B_SPLINE_CURVE ( 3, ( #33517, #20722, #27108, #33307 ),
 .UNSPECIFIED., .F., .T. ) 
 B_SPLINE_CURVE_WITH_KNOTS ( ( 4, 4 ),
 ( 1.381924640371168689, 1.574767692156077370 ),
 .UNSPECIFIED. ) 
 CURVE ( )  GEOMETRIC_REPRESENTATION_ITEM ( )  RATIONAL_B_SPLINE_CURVE ( ( 1.000000000000000000, 0.9969033633783032089, 0.9969033633783032089, 1.000000000000000000 ) ) 
 REPRESENTATION_ITEM ( '' )  );
#11623 = CARTESIAN_POINT ( 'NONE',  ( 14.66778827922366268, 13.14255605609920963, 2.495661121409653127 ) ) ;
#11624 = CYLINDRICAL_SURFACE ( 'NONE', #5661, 0.1000000000000028644 ) ;
#11625 = CARTESIAN_POINT ( 'NONE',  ( -77.92837670882107659, 2.429809908903242555, -12.50000000000000000 ) ) ;
#11626 = CARTESIAN_POINT ( 'NONE',  ( 5.067738213087761068, -29.09985929542945371, 7.754798119455333705 ) ) ;
#11627 = AXIS2_PLACEMENT_3D ( 'NONE', #32231, #9777, #13070 ) ;
#11628 = AXIS2_PLACEMENT_3D ( 'NONE', #27412, #22021, #21246 ) ;
#11629 = B_SPLINE_CURVE_WITH_KNOTS ( 'NONE', 3,
 ( #368, #10212, #9817, #34963, #9610, #6541, #32069, #19497, #28762, #22193 ),
 .UNSPECIFIED., .F., .F.,
 ( 4, 3, 3, 4 ),
 ( 0.0001585009270395730399, 0.0001815657551981798032, 0.0002118214035944114755, 0.0002170292169044780875 ),
 .UNSPECIFIED. ) ;
#11630 = CARTESIAN_POINT ( 'NONE',  ( -70.92837671539291478, 0.2169278822316458022, 3.999987187540717137 ) ) ;
#11631 = CARTESIAN_POINT ( 'NONE',  ( 2.183653651549320340, -33.03640625185305879, 7.750000000000000888 ) ) ;
#11632 = LINE ( 'NONE', #11226, #10231 ) ;
#11633 = ORIENTED_EDGE ( 'NONE', *, *, #9799, .F. ) ;
#11634 = CARTESIAN_POINT ( 'NONE',  ( 67.97136023280155825, 58.53559134324396496, 3.990965707299543475 ) ) ;
#11635 = CARTESIAN_POINT ( 'NONE',  ( 27.40853967452441609, 0.9677969527344274514, 4.484163512883236891 ) ) ;
#11636 = EDGE_CURVE ( 'NONE', #31330, #31687, #35428, .T. ) ;
#11637 = DIRECTION ( 'NONE',  ( -0.000000000000000000, -0.000000000000000000, 1.000000000000000000 ) ) ;
#11639 = EDGE_CURVE ( 'NONE', #36975, #18458, #18382, .T. ) ;
#11638 = CARTESIAN_POINT ( 'NONE',  ( 85.22136629666657370, 2.371628277241609517, -4.205523829021379001 ) ) ;
#11641 = CARTESIAN_POINT ( 'NONE',  ( 1.888104015524238566, -33.07173515984538170, 7.139344958878410807 ) ) ;
#11640 = DIRECTION ( 'NONE',  ( 0.000000000000000000, -1.000000000000000000, 0.000000000000000000 ) ) ;
#11642 = CARTESIAN_POINT ( 'NONE',  ( 27.60344192425479193, 81.15229837709949834, 1.000000000000000000 ) ) ;
#11643 = DIRECTION ( 'NONE',  ( 1.000000000000000000, 0.000000000000000000, 0.000000000000000000 ) ) ;
#11644 = CARTESIAN_POINT ( 'NONE',  ( -70.12941265528974100, -21.39831437159005390, 5.947290612307118529 ) ) ;
#11645 = EDGE_CURVE ( 'NONE', #28100, #22494, #33462, .T. ) ;
#11646 = ORIENTED_EDGE ( 'NONE', *, *, #38389, .F. ) ;
#11647 = CARTESIAN_POINT ( 'NONE',  ( -71.04476776058896803, -21.78243674987466605, 3.999856464806923473 ) ) ;
#11648 = AXIS2_PLACEMENT_3D ( 'NONE', #12710, #25481, #18895 ) ;
#11649 = CARTESIAN_POINT ( 'NONE',  ( 78.70885197775000108, 65.89012877898849752, -1.994058748902171496 ) ) ;
#11650 = AXIS2_PLACEMENT_3D ( 'NONE', #25858, #38601, #7719 ) ;
#11651 = LINE ( 'NONE', #8772, #27302 ) ;
#11652 = AXIS2_PLACEMENT_3D ( 'NONE', #5943, #24047, #15196 ) ;
#11653 = CARTESIAN_POINT ( 'NONE',  ( 81.06091538032737276, 61.57736434115996360, 2.238287240292558433 ) ) ;
#11654 = CARTESIAN_POINT ( 'NONE',  ( 24.11448298858268657, 0.5898710210986063407, 5.089296224101761190 ) ) ;
#11656 = VERTEX_POINT ( 'NONE', #6046 ) ;
#11655 = CARTESIAN_POINT ( 'NONE',  ( -0.7665672367818757715, -27.23024611671144157, 6.929923840112066635 ) ) ;
#11657 = COLOUR_RGB ( '',0.7921568627450980005, 0.8196078431372548767, 0.9333333333333333481 ) ;
#11658 = CARTESIAN_POINT ( 'NONE',  ( 74.03116782478153368, 60.19763641771454132, -3.876585409280477901 ) ) ;
#11659 = CARTESIAN_POINT ( 'NONE',  ( 3.215381038209046416, -32.61374398135161812, 6.959317978105166169 ) ) ;
#11661 = CARTESIAN_POINT ( 'NONE',  ( -3.078675913592197944, -26.64985754041175525, 6.700000000000000178 ) ) ;
#11660 = CARTESIAN_POINT ( 'NONE',  ( 4.973240196557726200, -30.81030636687787450, 6.880608371227952880 ) ) ;
#11662 = DIRECTION ( 'NONE',  ( 0.6427876096865379196, 0.7660444431189793457, -0.000000000000000000 ) ) ;
#11663 = PLANE ( 'NONE',  #30087 ) ;
#11664 = CARTESIAN_POINT ( 'NONE',  ( -1.594400172063576981, -30.70591517047275332, 7.785593909369613819 ) ) ;
#11665 = CARTESIAN_POINT ( 'NONE',  ( 23.14273095532835001, 4.006691610855233066, -3.147203323943627229 ) ) ;
#11666 = ORIENTED_EDGE ( 'NONE', *, *, #13112, .T. ) ;
#11667 = DIRECTION ( 'NONE',  ( -0.000000000000000000, -0.000000000000000000, 1.000000000000000000 ) ) ;
#11668 = CARTESIAN_POINT ( 'NONE',  ( 24.99455384622441301, -2.608472216378299180, -6.027016329390949778 ) ) ;
#11669 = CARTESIAN_POINT ( 'NONE',  ( 0.5502190760550982329, -32.76947806258566231, 7.635761828346577573 ) ) ;
#11670 = DIRECTION ( 'NONE',  ( -0.000000000000000000, 1.000000000000000000, -0.000000000000000000 ) ) ;
#11671 = CARTESIAN_POINT ( 'NONE',  ( 81.16101395366627003, 61.30084446962307254, 1.089225060639237519 ) ) ;
#11672 = CARTESIAN_POINT ( 'NONE',  ( 86.04767080185138184, 0.5164224212623146348, 6.001289606117265585 ) ) ;
#11673 = CARTESIAN_POINT ( 'NONE',  ( 1.300000000000000044, 4.990463472878845329E-16, 4.075022672948151126 ) ) ;
#11674 = ORIENTED_EDGE ( 'NONE', *, *, #21868, .F. ) ;
#11675 = CARTESIAN_POINT ( 'NONE',  ( 0.3856705772283747780, -32.81361829944838604, 7.750000000000000888 ) ) ;
#11676 = DIRECTION ( 'NONE',  ( 0.000000000000000000, 0.000000000000000000, -1.000000000000000000 ) ) ;
#11677 = CARTESIAN_POINT ( 'NONE',  ( 33.97225482870646118, -3.752748478265877541, -5.291075728257928823 ) ) ;
#11678 = CARTESIAN_POINT ( 'NONE',  ( -65.15514661499977933, 34.97220226750605576, -6.888442104241543795 ) ) ;
#11679 = CARTESIAN_POINT ( 'NONE',  ( -1.391746016950013320, -31.20965402480746320, 7.750000000000000888 ) ) ;
#11680 = B_SPLINE_CURVE_WITH_KNOTS ( 'NONE', 3,
 ( #25342, #6403, #3537, #435, #2930, #34833, #24722, #12363, #15449, #37470 ),
 .UNSPECIFIED., .F., .F.,
 ( 4, 3, 3, 4 ),
 ( 0.0001585009270395724165, 0.0001815657551981832726, 0.0002118214035944120176, 0.0002170292169044778436 ),
 .UNSPECIFIED. ) ;
#11681 = CARTESIAN_POINT ( 'NONE',  ( -38.44874870218063734, -26.64985754041175525, 6.700000000000000178 ) ) ;
#11682 = ORIENTED_EDGE ( 'NONE', *, *, #17454, .F. ) ;
#11683 = DIRECTION ( 'NONE',  ( 0.000000000000000000, 0.000000000000000000, 1.000000000000000000 ) ) ;
#11684 = CIRCLE ( 'NONE', #16964, 67.42751648247021024 ) ;
#11685 = CARTESIAN_POINT ( 'NONE',  ( 86.31823139319517679, 1.400990185460310844, -4.784756222713710372 ) ) ;
#11686 = ORIENTED_EDGE ( 'NONE', *, *, #35035, .T. ) ;
#11687 = ORIENTED_EDGE ( 'NONE', *, *, #26554, .F. ) ;
#11689 = CARTESIAN_POINT ( 'NONE',  ( 37.17692586084726969, -2.564445794282764979, 5.980943416423468939 ) ) ;
#11688 = CARTESIAN_POINT ( 'NONE',  ( 80.17140661427380621, 64.93185644258198863, -3.352621494407066915 ) ) ;
#11690 = CARTESIAN_POINT ( 'NONE',  ( 17.97890173384453760, -2.875347590309559553, 3.012440455584755039 ) ) ;
#11691 = FACE_OUTER_BOUND ( 'NONE', #24503, .T. ) ;
#11692 = DIRECTION ( 'NONE',  ( 0.000000000000000000, 0.000000000000000000, -1.000000000000000000 ) ) ;
#11693 = ADVANCED_FACE ( 'NONE', ( #14883 ), #27651, .F. ) ;
#11694 = ORIENTED_EDGE ( 'NONE', *, *, #17306, .F. ) ;
#11695 = CARTESIAN_POINT ( 'NONE',  ( 0.5470676372252714081, -32.88165439262409251, 7.255881584735162981 ) ) ;
#11696 = EDGE_CURVE ( 'NONE', #8305, #8931, #34069, .T. ) ;
#11697 = ORIENTED_EDGE ( 'NONE', *, *, #11319, .F. ) ;
#11698 = EDGE_CURVE ( 'NONE', #6354, #8844, #4086, .T. ) ;
#11699 = EDGE_LOOP ( 'NONE', ( #38003, #30411, #28425, #32795 ) ) ;
#11700 = CARTESIAN_POINT ( 'NONE',  ( -2.184219888937934950, -32.98850935093154391, 7.754798119455333705 ) ) ;
#11701 = CARTESIAN_POINT ( 'NONE',  ( 79.22373596144829833, 65.64748706429479341, -2.718470589328617848 ) ) ;
#11702 = AXIS2_PLACEMENT_3D ( 'NONE', #14762, #30432, #4902 ) ;
#11703 = CARTESIAN_POINT ( 'NONE',  ( 14.76534721654833504, -5.157638883270574404, 2.500001661686563015 ) ) ;
#11704 = VERTEX_POINT ( 'NONE', #21082 ) ;
#11706 = CARTESIAN_POINT ( 'NONE',  ( 4.286018331208381937, -27.36209527917707263, 7.730758795053807475 ) ) ;
#11705 = CARTESIAN_POINT ( 'NONE',  ( 24.54080388820417014, 2.535510198792493508, 4.001279714722917547 ) ) ;
#11707 = ORIENTED_EDGE ( 'NONE', *, *, #29977, .T. ) ;
#11708 = CARTESIAN_POINT ( 'NONE',  ( 80.79165360588653755, 65.97001311340675045, -2.094266784919526447 ) ) ;
#11709 = PLANE ( 'NONE',  #19327 ) ;
#11710 = ORIENTED_EDGE ( 'NONE', *, *, #19677, .F. ) ;
#11712 = CARTESIAN_POINT ( 'NONE',  ( 16.54345625214024196, -3.183194016283426908, -2.788404471784634797 ) ) ;
#11711 = CARTESIAN_POINT ( 'NONE',  ( -0.01072294803718611307, -26.63188197674012159, 7.756377446753162097 ) ) ;
#11713 = CARTESIAN_POINT ( 'NONE',  ( -70.92837670882107659, -56.35932253828835314, -6.000000000000002665 ) ) ;
#11714 = CARTESIAN_POINT ( 'NONE',  ( 73.13464764220530867, 62.20839851451114555, 3.391332960900173887 ) ) ;
#11715 = B_SPLINE_CURVE_WITH_KNOTS ( 'NONE', 3,
 ( #17350, #20063, #23560, #33239 ),
 .UNSPECIFIED., .F., .F.,
 ( 4, 4 ),
 ( 8.673617379884035472E-19, 0.0005391349717845210499 ),
 .UNSPECIFIED. ) ;
#11716 = CARTESIAN_POINT ( 'NONE',  ( 22.64042881234975724, 3.244544948583774513, -4.225217879000846999 ) ) ;
#11717 = DIRECTION ( 'NONE',  ( 1.000000000000000000, 0.000000000000000000, 0.000000000000000000 ) ) ;
#11718 = VECTOR ( 'NONE', #3646, 1000.000000000000000 ) ;
#11719 = CARTESIAN_POINT ( 'NONE',  ( 21.85643539959777470, -5.967561930184303698, -15.30482168765389694 ) ) ;
#11720 = CARTESIAN_POINT ( 'NONE',  ( -53.21549048184568420, -30.38627270959228710, 6.000000000000000000 ) ) ;
#11721 = EDGE_LOOP ( 'NONE', ( #19383, #15515, #12945, #31925 ) ) ;
#11722 = CARTESIAN_POINT ( 'NONE',  ( -1.654012860102806570, -29.01496998062980381, 7.695279973900954751 ) ) ;
#11723 = CARTESIAN_POINT ( 'NONE',  ( 80.24765655772210948, 65.96146312294942504, 2.334361474588997787 ) ) ;
#11724 = CARTESIAN_POINT ( 'NONE',  ( 86.69860591627480062, 0.9737354674733970095, 5.003702464200671329 ) ) ;
#11725 = DIRECTION ( 'NONE',  ( -0.7877517966954343809, 0.6159927814537400348, 0.000000000000000000 ) ) ;
#11726 = CARTESIAN_POINT ( 'NONE',  ( 1.713892699967800581, -32.96990337146582561, 7.635761828346577573 ) ) ;
#11727 = DIRECTION ( 'NONE',  ( 1.000000000000000000, 0.000000000000000000, 0.000000000000000000 ) ) ;
#11728 = DIRECTION ( 'NONE',  ( -0.000000000000000000, 1.000000000000000000, -0.000000000000000000 ) ) ;
#11729 = CIRCLE ( 'NONE', #14350, 0.1000000000000028644 ) ;
#11730 = CARTESIAN_POINT ( 'NONE',  ( 36.91148996621163292, -2.638676746795284078, -5.967328735622324132 ) ) ;
#11731 = CARTESIAN_POINT ( 'NONE',  ( 5.185377850561007307, -29.62128986762933280, 7.785344483711591934 ) ) ;
#11732 = CARTESIAN_POINT ( 'NONE',  ( 4.256814889047467076, -33.88948601255670212, 7.695279973900954751 ) ) ;
#11733 = CARTESIAN_POINT ( 'NONE',  ( 4.363193498965130424, -31.82791667060237728, 7.778495531946297170 ) ) ;
#11734 = CARTESIAN_POINT ( 'NONE',  ( -70.26294730757642526, -45.76915084690816826, 5.963676894908396697 ) ) ;
#11735 = ORIENTED_EDGE ( 'NONE', *, *, #3492, .T. ) ;
#11736 = CARTESIAN_POINT ( 'NONE',  ( 36.49301456553985190, -3.557456006871358323, 5.797608776528274888 ) ) ;
#11737 = CARTESIAN_POINT ( 'NONE',  ( -71.35621909400492768, 0.1208619214844364048, 5.996770606117012292 ) ) ;
#11738 = CARTESIAN_POINT ( 'NONE',  ( 66.83775678531991105, 58.01055738293738528, -3.998747512904051060 ) ) ;
#11739 = CARTESIAN_POINT ( 'NONE',  ( 5.200390093233090205, -29.56993018339339940, 7.800000000000000711 ) ) ;
#11740 = CARTESIAN_POINT ( 'NONE',  ( -12.99139449055068241, -10.90558813203967148, -6.000000000000000000 ) ) ;
#11741 = ORIENTED_EDGE ( 'NONE', *, *, #37238, .T. ) ;
#11742 = CARTESIAN_POINT ( 'NONE',  ( -0.5720469289765105492, -32.09896754572934441, 7.761597726988858525 ) ) ;
#11744 = ADVANCED_FACE ( 'NONE', ( #40009, #24780 ), #27049, .F. ) ;
#11743 = CARTESIAN_POINT ( 'NONE',  ( -72.11798225935933715, 5.092045952281377907, -9.929846635402185484 ) ) ;
#11745 = CARTESIAN_POINT ( 'NONE',  ( 71.72536746055673973, 61.26079380681123610, 3.629563705067941903 ) ) ;
#11746 = CARTESIAN_POINT ( 'NONE',  ( 0.9976637635090632727, -32.89651637730339928, 6.864276522220859711 ) ) ;
#11747 = B_SPLINE_CURVE_WITH_KNOTS ( 'NONE', 3,
 ( #3248, #24619, #21955, #15966, #27905, #37988, #338, #18851, #12878, #31424, #3040, #15558, #21547, #6302, #9584, #12471, #15767, #37173, #9789, #25442, #28323, #139, #12670, #25245 ),
 .UNSPECIFIED., .F., .F.,
 ( 4, 2, 2, 2, 1, 1, 2, 2, 2, 2, 2, 2, 4 ),
 ( 0.000000000000000000, 0.2499999999999828471, 0.3749999999999742428, 0.4374999999999711342, 0.4687499999999695799, 0.4843749999999687472, 0.4921874999999684142, 0.4999999999999680256, 0.6249999999999711342, 0.6874999999999725775, 0.7187499999999753530, 0.7499999999999780176, 1.000000000000000000 ),
 .UNSPECIFIED. ) ;
#11748 = ORIENTED_EDGE ( 'NONE', *, *, #40236, .T. ) ;
#11749 = FACE_OUTER_BOUND ( 'NONE', #2735, .T. ) ;
#11750 = CARTESIAN_POINT ( 'NONE',  ( 1.278812785396021612, -26.09541258039915590, 6.980586498568971621 ) ) ;
#11751 = ORIENTED_EDGE ( 'NONE', *, *, #13383, .F. ) ;
#11752 = CARTESIAN_POINT ( 'NONE',  ( 22.88444072573192400, 4.292063183685437266, 3.118239780378390780 ) ) ;
#11753 = CARTESIAN_POINT ( 'NONE',  ( 82.53033050081239708, 64.25366301186836893, -1.161365684106807850 ) ) ;
#11754 = CARTESIAN_POINT ( 'NONE',  ( 80.84870020435621996, 62.70902516261514847, 3.354617312347321967 ) ) ;
#11755 = LINE ( 'NONE', #24748, #2230 ) ;
#11756 = ORIENTED_EDGE ( 'NONE', *, *, #31072, .T. ) ;
#11757 = CARTESIAN_POINT ( 'NONE',  ( 79.19973406752563960, 61.05435877263160904, -2.913524936156958844 ) ) ;
#11759 = DIRECTION ( 'NONE',  ( 1.000000000000000000, 0.000000000000000000, 0.000000000000000000 ) ) ;
#11758 = CARTESIAN_POINT ( 'NONE',  ( 26.06763236307823561, 0.7305744058604376479, 4.422384865831292977 ) ) ;
#11760 = CARTESIAN_POINT ( 'NONE',  ( 78.68330935989223462, 66.05356751642949575, -1.089225060638855602 ) ) ;
#11761 = CARTESIAN_POINT ( 'NONE',  ( 77.57568143946795658, 64.97578145858237519, 2.643019404357015656 ) ) ;
#11762 = ORIENTED_EDGE ( 'NONE', *, *, #17560, .T. ) ;
#11763 = CARTESIAN_POINT ( 'NONE',  ( -0.8270868501854790056, -27.29575654199287271, 7.759451378593098525 ) ) ;
#11764 = CARTESIAN_POINT ( 'NONE',  ( 81.46661790917879387, 61.46529165999842093, 1.093381982072756164 ) ) ;
#11766 = FACE_OUTER_BOUND ( 'NONE', #34892, .T. ) ;
#11765 = CARTESIAN_POINT ( 'NONE',  ( 4.947714365125587932, -30.86868380840103043, 7.766640943994651103 ) ) ;
#11767 = CARTESIAN_POINT ( 'NONE',  ( 32.32438508616473882, -2.203219671913323019, -5.968588774572396893 ) ) ;
#11768 = EDGE_CURVE ( 'NONE', #1778, #17373, #16799, .T. ) ;
#11769 = CARTESIAN_POINT ( 'NONE',  ( 14.61802081865031688, -4.584994529579697442, -2.500000000000000444 ) ) ;
#11770 = DIRECTION ( 'NONE',  ( 1.000000000000000000, 0.000000000000000000, 0.000000000000000000 ) ) ;
#11771 = CARTESIAN_POINT ( 'NONE',  ( 1.636219183984862990, -33.06935340522112909, 6.870737987065012931 ) ) ;
#11772 = CARTESIAN_POINT ( 'NONE',  ( 26.70586447420738807, 0.9595633775789119690, -4.381173435910611147 ) ) ;
#11773 = CIRCLE ( 'NONE', #34844, 3.000000000000002665 ) ;
#11774 = CARTESIAN_POINT ( 'NONE',  ( 1.140861248955154839, -32.93077579228409490, 7.257242401810563237 ) ) ;
#11775 = LINE ( 'NONE', #33851, #33608 ) ;
#11776 = B_SPLINE_CURVE_WITH_KNOTS ( 'NONE', 3,
 ( #20397, #8796, #14220, #26795, #39333, #11123, #23693, #30086, #1900, #37015, #27951, #30862, #40300, #12090, #24664, #37216, #21589, #34171, #12716, #19306, #28782, #589, #28156, #22000, #25086 ),
 .UNSPECIFIED., .F., .F.,
 ( 4, 3, 3, 3, 3, 3, 3, 3, 4 ),
 ( 6.468151674594163625E-05, 9.076621574722140316E-05, 0.0001210204262067974922, 0.0001512763324577456252, 0.0001815301820994263905, 0.0002117781465860695401, 0.0002420274594459763731, 0.0002722905548971228900, 0.0002816827545175647511 ),
 .UNSPECIFIED. ) ;
#11777 = CARTESIAN_POINT ( 'NONE',  ( -1.058242811331675304, -31.72385899209557181, 7.753200566781599967 ) ) ;
#11778 = CARTESIAN_POINT ( 'NONE',  ( -70.92837671539291478, 0.2169278822316458022, 3.999987187540717137 ) ) ;
#11779 = CARTESIAN_POINT ( 'NONE',  ( 35.67318982790884974, -1.412481467646560462, -5.626421653071801643 ) ) ;
#11780 = CARTESIAN_POINT ( 'NONE',  ( 3.382900834235484933, -26.61540788991811013, 7.643333865083961065 ) ) ;
#11781 = CARTESIAN_POINT ( 'NONE',  ( 5.044196383407847151, -28.95432172001934035, 7.652160403243382980 ) ) ;
#11782 = DIRECTION ( 'NONE',  ( 0.000000000000000000, 0.000000000000000000, 1.000000000000000000 ) ) ;
#11783 = PRODUCT ( 'Heavy Cast Steel Frame Chassis', 'Heavy Cast Steel Frame Chassis', '', ( #27070 ) ) ;
#11784 = FACE_OUTER_BOUND ( 'NONE', #19733, .T. ) ;
#11785 = CARTESIAN_POINT ( 'NONE',  ( -72.84815947045233031, 2.429809908889422498, 10.96147798754374669 ) ) ;
#11786 = EDGE_CURVE ( 'NONE', #14653, #33732, #13279, .T. ) ;
#11787 = CARTESIAN_POINT ( 'NONE',  ( 3.504784550580148483, -26.68823612567400971, 7.754798119455333705 ) ) ;
#11788 = VECTOR ( 'NONE', #2967, 1000.000000000000000 ) ;
#11789 = EDGE_LOOP ( 'NONE', ( #27767, #15562, #31435, #21606, #16472, #27022 ) ) ;
#11790 = CARTESIAN_POINT ( 'NONE',  ( 4.404516770028684469, -31.79202354683301834, 7.695279973900954751 ) ) ;
#11791 = CARTESIAN_POINT ( 'NONE',  ( 70.73355890789336797, 59.99733340013641936, -3.925556587156273647 ) ) ;
#11792 = ORIENTED_EDGE ( 'NONE', *, *, #28704, .T. ) ;
#11793 = CARTESIAN_POINT ( 'NONE',  ( -37.07867591359219261, -26.64985754041175525, 6.700000000000000178 ) ) ;
#11795 = EDGE_CURVE ( 'NONE', #1142, #28508, #15716, .T. ) ;
#11794 = CARTESIAN_POINT ( 'NONE',  ( -2.271193562574106650, -32.88485816291451869, 7.635761828346577573 ) ) ;
#11796 = CARTESIAN_POINT ( 'NONE',  ( 4.040170416529481834, -33.73639438183194983, 7.013842709614101167 ) ) ;
#11798 = CARTESIAN_POINT ( 'NONE',  ( 1.311799688994542246, -26.19220832609979155, 6.920489980334476599 ) ) ;
#11797 = DIRECTION ( 'NONE',  ( 0.000000000000000000, 0.000000000000000000, -1.000000000000000000 ) ) ;
#11799 = SHAPE_DEFINITION_REPRESENTATION ( #19319, #39533 ) ;
#11800 = CARTESIAN_POINT ( 'NONE',  ( 2.184403768844786597, -32.93531068382346660, 7.768425012602592439 ) ) ;
#11801 = ORIENTED_EDGE ( 'NONE', *, *, #1597, .F. ) ;
#11802 = CARTESIAN_POINT ( 'NONE',  ( 21.98862019667479828, 5.618512022731773747, 3.087214410704674172 ) ) ;
#11803 = VECTOR ( 'NONE', #7326, 1000.000000000000000 ) ;
#11804 = SURFACE_STYLE_USAGE ( .BOTH. , #30581 ) ;
#11805 = CARTESIAN_POINT ( 'NONE',  ( 22.14748389186037159, -3.079134181252381808, 3.566341549651656617 ) ) ;
#11806 = VERTEX_POINT ( 'NONE', #16759 ) ;
#11807 = CARTESIAN_POINT ( 'NONE',  ( 80.58155366896997407, 61.83530676836470974, -2.934133054905257776 ) ) ;
#11808 = B_SPLINE_CURVE_WITH_KNOTS ( 'NONE', 3,
 ( #30759, #18167, #14664, #30339, #11771, #5014, #14873, #27235, #39801, #30543, #24351, #36915, #21275, #33847, #24769, #15701, #31564, #6240, #9113, #27843, #12408, #5833, #34674, #15290, #31363, #9728, #18784, #3387, #19004, #6451, #40396 ),
 .UNSPECIFIED., .F., .F.,
 ( 4, 3, 3, 3, 3, 3, 3, 3, 3, 3, 4 ),
 ( 1.084202172485504434E-18, 3.077658087705624490E-05, 6.152638666998984352E-05, 9.267501192706536313E-05, 0.0001241882240135194423, 0.0001556618703051674234, 0.0001866161554452220326, 0.0002167966385860974423, 0.0002463805737537784111, 0.0002758761370306540080, 0.0002847094172290046696 ),
 .UNSPECIFIED. ) ;
#11809 = CARTESIAN_POINT ( 'NONE',  ( 16.92333532088173698, 7.515569096285618755, -3.484773916740906863 ) ) ;
#11810 = CARTESIAN_POINT ( 'NONE',  ( 80.19490802141253027, 65.93291197049440200, -2.397965335136836629 ) ) ;
#11811 = CARTESIAN_POINT ( 'NONE',  ( 78.46701299008461206, 65.82614401021746176, 1.855758959884434400 ) ) ;
#11812 = ORIENTED_EDGE ( 'NONE', *, *, #17360, .F. ) ;
#11813 = DIRECTION ( 'NONE',  ( 0.000000000000000000, -0.000000000000000000, -1.000000000000000000 ) ) ;
#11814 = AXIS2_PLACEMENT_3D ( 'NONE', #18428, #9169, #34323 ) ;
#11816 = ORIENTED_EDGE ( 'NONE', *, *, #3950, .F. ) ;
#11815 = DIRECTION ( 'NONE',  ( 0.000000000000000000, 1.000000000000000000, 0.000000000000000000 ) ) ;
#11817 = CARTESIAN_POINT ( 'NONE',  ( 21.85643539959776760, -1.193669045901033066, -12.68912657263372346 ) ) ;
#11818 = ORIENTED_EDGE ( 'NONE', *, *, #22804, .T. ) ;
#11819 = CARTESIAN_POINT ( 'NONE',  ( -79.06493839038353144, 10.34607662704177145, 5.825634118554894769 ) ) ;
#11820 = DIRECTION ( 'NONE',  ( -0.000000000000000000, -0.000000000000000000, -1.000000000000000000 ) ) ;
#11821 = LINE ( 'NONE', #15337, #7042 ) ;
#11822 = CARTESIAN_POINT ( 'NONE',  ( -73.26201557575831202, 7.663664970033887691, -9.727200596108295017 ) ) ;
#11823 = CARTESIAN_POINT ( 'NONE',  ( -0.03129586030734986257, -26.63571487215777012, 7.257242401810563237 ) ) ;
#11824 = CARTESIAN_POINT ( 'NONE',  ( 2.495811076861738975, -26.26428262444142447, 6.969307238440507923 ) ) ;
#11825 = APPLICATION_CONTEXT ( 'automotive_design' ) ;
#11826 = FACE_OUTER_BOUND ( 'NONE', #16483, .T. ) ;
#11827 = CARTESIAN_POINT ( 'NONE',  ( 15.02955287353362124, 11.88006370660428246, 2.552123235661551526 ) ) ;
#11828 = CARTESIAN_POINT ( 'NONE',  ( -54.01549048184568846, -38.28842912540938670, -4.152976064860135708 ) ) ;
#11829 = B_SPLINE_CURVE_WITH_KNOTS ( 'NONE', 3,
 ( #20108, #16018, #35386, #10438, #19312, #10033, #22615, #10237, #10633, #25896 ),
 .UNSPECIFIED., .F., .F.,
 ( 4, 3, 3, 4 ),
 ( 0.0002170292169044822075, 0.0002420761345915959837, 0.0002723302478206999860, 0.0002816811360866905162 ),
 .UNSPECIFIED. ) ;
#11830 = CARTESIAN_POINT ( 'NONE',  ( -60.75950795826495465, 23.17721540975219696, -12.49999999999999645 ) ) ;
#11831 = EDGE_CURVE ( 'NONE', #4684, #4341, #38385, .T. ) ;
#11832 = EDGE_CURVE ( 'NONE', #36751, #462, #26262, .T. ) ;
#11833 = CARTESIAN_POINT ( 'NONE',  ( -4.448748702180642667, -26.64985754041175525, 6.700000000000000178 ) ) ;
#11834 = EDGE_CURVE ( 'NONE', #24757, #8717, #9585, .T. ) ;
#11835 = TOROIDAL_SURFACE ( 'NONE', #31594, 10.99999999999998579, 3.000000000000000000 ) ;
#11836 = DIRECTION ( 'NONE',  ( -0.000000000000000000, -1.000000000000000000, -0.000000000000000000 ) ) ;
#11837 = CARTESIAN_POINT ( 'NONE',  ( -20.97867591359219475, -26.64985754041175525, 6.700000000000000178 ) ) ;
#11838 = CARTESIAN_POINT ( 'NONE',  ( 24.67315655365684890, 2.664633189631731458, -3.911906493327204526 ) ) ;
#11839 = ORIENTED_EDGE ( 'NONE', *, *, #2406, .F. ) ;
#11840 = CARTESIAN_POINT ( 'NONE',  ( 0.7149948906900660539, -26.31585638355339185, 7.013842709614101167 ) ) ;
#11841 = VERTEX_POINT ( 'NONE', #16170 ) ;
#11842 = CARTESIAN_POINT ( 'NONE',  ( 67.39973655466486946, 58.28774108029888623, 3.995059460290580233 ) ) ;
#11843 = CARTESIAN_POINT ( 'NONE',  ( 20.42597344558877026, 3.670373271656663938, 3.394365178855436760 ) ) ;
#11844 = FACE_OUTER_BOUND ( 'NONE', #14389, .T. ) ;
#11845 = LINE ( 'NONE', #36979, #27308 ) ;
#11846 = CARTESIAN_POINT ( 'NONE',  ( 85.98118993947397826, 1.447477879098551856, 5.565446759936045318 ) ) ;
#11847 = VECTOR ( 'NONE', #27802, 1000.000000000000000 ) ;
#11848 = EDGE_CURVE ( 'NONE', #35180, #11501, #28940, .T. ) ;
#11850 = CARTESIAN_POINT ( 'NONE',  ( 2.321451664048270302, -33.01438696571141662, 7.635761828346576685 ) ) ;
#11849 = CARTESIAN_POINT ( 'NONE',  ( -71.05898624497616822, -21.78299143688729700, 5.999999999999970690 ) ) ;
#11851 = EDGE_LOOP ( 'NONE', ( #16027, #16428, #16580, #8604, #1702 ) ) ;
#11852 = CARTESIAN_POINT ( 'NONE',  ( -1.606710073356391266, -28.78057064038158686, 6.988553391373223178 ) ) ;
#11853 = CARTESIAN_POINT ( 'NONE',  ( -31.07867591359219617, -26.64985754041175525, 6.700000000000000178 ) ) ;
#11854 = CARTESIAN_POINT ( 'NONE',  ( -0.6804824730526998211, -32.13536305585522257, 7.006908160621411419 ) ) ;
#11855 = ORIENTED_EDGE ( 'NONE', *, *, #10863, .F. ) ;
#11856 = CARTESIAN_POINT ( 'NONE',  ( -70.93014222716664108, -21.78919581838237463, 4.001025162589363582 ) ) ;
#11857 = CARTESIAN_POINT ( 'NONE',  ( 81.00146336277434500, 61.29413404061270398, -1.724274471760811167 ) ) ;
#11858 = CARTESIAN_POINT ( 'NONE',  ( -1.518021638882832702, -28.19449355359958176, 6.945385021654667312 ) ) ;
#11859 = CARTESIAN_POINT ( 'NONE',  ( 79.45910779949859659, 64.84755599131123915, 3.411701596789212143 ) ) ;
#11861 = ORIENTED_EDGE ( 'NONE', *, *, #4021, .T. ) ;
#11860 = CARTESIAN_POINT ( 'NONE',  ( -0.8725572984338751947, -27.34733221711291051, 6.894806418505345036 ) ) ;
#11862 = CARTESIAN_POINT ( 'NONE',  ( 74.35309583984513893, 59.45637312398173435, -3.556895493431092348 ) ) ;
#11863 = CARTESIAN_POINT ( 'NONE',  ( 3.264211231867342189, -32.58896295500613149, 6.871394612369936539 ) ) ;
#11864 =( BOUNDED_CURVE ( )  B_SPLINE_CURVE ( 3, ( #15319, #15114, #12011, #300 ),
 .UNSPECIFIED., .F., .T. ) 
 B_SPLINE_CURVE_WITH_KNOTS ( ( 4, 4 ),
 ( 1.381924640371167579, 1.574767692156076260 ),
 .UNSPECIFIED. ) 
 CURVE ( )  GEOMETRIC_REPRESENTATION_ITEM ( )  RATIONAL_B_SPLINE_CURVE ( ( 1.000000000000000000, 0.9969033633783032089, 0.9969033633783032089, 1.000000000000000000 ) ) 
 REPRESENTATION_ITEM ( '' )  );
#11866 = PLANE ( 'NONE',  #36757 ) ;
#11865 = CARTESIAN_POINT ( 'NONE',  ( 4.921080693996054300, -30.94002217087347262, 6.921725064902942925 ) ) ;
#11867 = DIRECTION ( 'NONE',  ( 0.000000000000000000, 1.000000000000000000, 0.000000000000000000 ) ) ;
#11868 = CARTESIAN_POINT ( 'NONE',  ( 23.72560648584031640, 3.533562144730845844, -3.260337319806162704 ) ) ;
#11869 = ORIENTED_EDGE ( 'NONE', *, *, #20208, .F. ) ;
#11870 = CARTESIAN_POINT ( 'NONE',  ( -51.01549048184568846, -30.38627270959228710, 6.800000000000000711 ) ) ;
#11871 = ADVANCED_FACE ( 'NONE', ( #22774 ), #22164, .F. ) ;
#11872 = CARTESIAN_POINT ( 'NONE',  ( 25.20438522764541744, -3.119311913904994515, 5.422531462276817038 ) ) ;
#11873 = EDGE_CURVE ( 'NONE', #40686, #21186, #38710, .T. ) ;
#11874 = AXIS2_PLACEMENT_3D ( 'NONE', #12203, #21692, #25180 ) ;
#11875 = CARTESIAN_POINT ( 'NONE',  ( -0.9665011745138262222, -31.83658251679149487, 7.743886751744248009 ) ) ;
#11876 = CARTESIAN_POINT ( 'NONE',  ( 0.9786193834823287974, -32.99384626346355986, 7.761113333117547697 ) ) ;
#11877 = CARTESIAN_POINT ( 'NONE',  ( 80.07838786650494001, 65.24465706271048759, 3.189931650267152641 ) ) ;
#11878 = CARTESIAN_POINT ( 'NONE',  ( 88.01214243333713227, -2.271333487497714465, 2.136702053253976885 ) ) ;
#11879 = LINE ( 'NONE', #24454, #26611 ) ;
#11880 = VERTEX_POINT ( 'NONE', #15967 ) ;
#11881 = CARTESIAN_POINT ( 'NONE',  ( 25.91700580362422812, 2.564115597501617216, -3.561092020512977907 ) ) ;
#11882 = CARTESIAN_POINT ( 'NONE',  ( -72.42837670882109080, -47.01774489676372326, 9.886859966642603581 ) ) ;
#11883 = EDGE_CURVE ( 'NONE', #4342, #24169, #949, .T. ) ;
#11884 = EDGE_LOOP ( 'NONE', ( #26290, #20183, #23152, #11801 ) ) ;
#11885 = CARTESIAN_POINT ( 'NONE',  ( 4.045015305582563059, -26.97130747677318041, 6.867199677474202346 ) ) ;
#11886 = CARTESIAN_POINT ( 'NONE',  ( 15.23668652445202021, -3.872406382219718335, -2.583925503793695899 ) ) ;
#11887 = DIRECTION ( 'NONE',  ( 0.5991095979999722099, -0.2428960078352049856, 0.7629346098860843028 ) ) ;
#11888 = CARTESIAN_POINT ( 'NONE',  ( -5.316495087772350026, -32.84709638682603838, -6.000000000000001776 ) ) ;
#11889 = CARTESIAN_POINT ( 'NONE',  ( 1.888484868039683962, -26.17513220563941800, 6.895222827070021765 ) ) ;
#11890 = CARTESIAN_POINT ( 'NONE',  ( 36.63303770807473825, -3.078030482662974077, 5.923869526346774883 ) ) ;
#11891 = DIRECTION ( 'NONE',  ( 0.000000000000000000, 0.000000000000000000, 1.000000000000000000 ) ) ;
#11892 = CARTESIAN_POINT ( 'NONE',  ( 1.700390093233090871, -29.56993018339339940, 7.750000000000000888 ) ) ;
#11893 = ORIENTED_EDGE ( 'NONE', *, *, #11562, .T. ) ;
#11894 = ORIENTED_EDGE ( 'NONE', *, *, #35615, .T. ) ;
#11896 = CARTESIAN_POINT ( 'NONE',  ( 32.06975058867338646, 0.2538586514417362494, 4.725460599369140091 ) ) ;
#11895 = CARTESIAN_POINT ( 'NONE',  ( 79.55653453243729700, 65.56957575487831491, -2.861733672647129634 ) ) ;
#11897 = CARTESIAN_POINT ( 'NONE',  ( 30.19003827612802482, -2.952522945788203845, 4.918283640461378781 ) ) ;
#11898 = LINE ( 'NONE', #33974, #5717 ) ;
#11899 = FACE_OUTER_BOUND ( 'NONE', #39502, .T. ) ;
#11900 = ORIENTED_EDGE ( 'NONE', *, *, #3392, .F. ) ;
#11901 = CARTESIAN_POINT ( 'NONE',  ( -4.878675913592187108, -26.64985754041175525, 6.700000000000000178 ) ) ;
#11902 = ORIENTED_EDGE ( 'NONE', *, *, #19675, .T. ) ;
#11903 = CIRCLE ( 'NONE', #34972, 8.204531065793066347 ) ;
#11904 = ORIENTED_EDGE ( 'NONE', *, *, #9368, .T. ) ;
#11905 = CARTESIAN_POINT ( 'NONE',  ( -8.878675913592189772, -24.55319635012989110, 6.700000000000000178 ) ) ;
#11906 = CARTESIAN_POINT ( 'NONE',  ( 80.81256737103976207, 62.69530837521176636, -3.364061116559605935 ) ) ;
#11907 = DIRECTION ( 'NONE',  ( 0.000000000000000000, 0.000000000000000000, 1.000000000000000000 ) ) ;
#11908 = VERTEX_POINT ( 'NONE', #22570 ) ;
#11910 = CARTESIAN_POINT ( 'NONE',  ( 21.44604159357209383, 7.932351888401207418, -2.756240841243536188 ) ) ;
#11909 = CARTESIAN_POINT ( 'NONE',  ( 22.26456873610839438, 2.506020883773357966, 5.102889090039424147 ) ) ;
#11911 = EDGE_LOOP ( 'NONE', ( #33311, #29144, #30526, #24486 ) ) ;
#11912 = CARTESIAN_POINT ( 'NONE',  ( 79.87389178145686230, 66.27500989097897843, -1.700667878122840593 ) ) ;
#11913 = DIRECTION ( 'NONE',  ( -1.000000000000000000, -0.000000000000000000, -0.000000000000000000 ) ) ;
#11914 = EDGE_CURVE ( 'NONE', #160, #38778, #32437, .T. ) ;
#11915 = CARTESIAN_POINT ( 'NONE',  ( -75.45330471031414277, 33.71485196875532608, -8.800414904976364028 ) ) ;
#11916 = ORIENTED_EDGE ( 'NONE', *, *, #27061, .T. ) ;
#11918 = CARTESIAN_POINT ( 'NONE',  ( 86.16949904519324832, 1.568053417999200505, -4.594337618669723788 ) ) ;
#11917 = CARTESIAN_POINT ( 'NONE',  ( 4.890701645444022638, -28.39438256639548896, 7.635761828346577573 ) ) ;
#11919 = CARTESIAN_POINT ( 'NONE',  ( -58.92473026143653669, 13.37661300689600274, 2.500000000000000000 ) ) ;
#11920 = CARTESIAN_POINT ( 'NONE',  ( 73.50720661118039345, 61.38260725348155944, 3.841642204035220942 ) ) ;
#11921 = ORIENTED_EDGE ( 'NONE', *, *, #9276, .T. ) ;
#11922 = CARTESIAN_POINT ( 'NONE',  ( 24.44644773797692494, 2.805227876606543713, -3.838340539723811062 ) ) ;
#11923 = VERTEX_POINT ( 'NONE', #16561 ) ;
#11924 = CARTESIAN_POINT ( 'NONE',  ( 21.85643539959774273, 11.87467848218428834, -0.9583437110454642305 ) ) ;
#11925 = DIRECTION ( 'NONE',  ( 0.000000000000000000, 0.000000000000000000, 1.000000000000000000 ) ) ;
#11926 = VERTEX_POINT ( 'NONE', #4235 ) ;
#11927 = CARTESIAN_POINT ( 'NONE',  ( -1.653558785517501795, -29.01221950110802794, 7.670860738520325128 ) ) ;
#11928 = EDGE_LOOP ( 'NONE', ( #7570, #39713, #23440, #31489 ) ) ;
#11929 = CARTESIAN_POINT ( 'NONE',  ( 80.10847647497645596, 65.88576991956399809, 2.484976468875361277 ) ) ;
#11930 = CARTESIAN_POINT ( 'NONE',  ( 86.67773139875836819, 0.9971827163122055637, 5.329716871657868005 ) ) ;
#11931 = LINE ( 'NONE', #37059, #13566 ) ;
#11932 = EDGE_CURVE ( 'NONE', #32407, #25870, #7307, .T. ) ;
#11933 = CARTESIAN_POINT ( 'NONE',  ( -80.91065676098010329, -6.597313057213482601, -0.5950503846463383040 ) ) ;
#11934 = ORIENTED_EDGE ( 'NONE', *, *, #11406, .F. ) ;
#11935 = CARTESIAN_POINT ( 'NONE',  ( 0.6356603237437735698, -26.34092700757140193, 6.864651958020303368 ) ) ;
#11936 = CARTESIAN_POINT ( 'NONE',  ( 3.121324086407806231, -26.64985754041175525, 6.800000000000000711 ) ) ;
#11937 = VECTOR ( 'NONE', #33533, 1000.000000000000000 ) ;
#11938 = ADVANCED_FACE ( 'NONE', ( #3851 ), #16369, .F. ) ;
#11939 = CARTESIAN_POINT ( 'NONE',  ( 36.98002556809775854, -2.957261013591625520, -5.978025373836474365 ) ) ;
#11940 = DIRECTION ( 'NONE',  ( -0.9396926207859058744, -0.3420201433256757628, -0.000000000000000000 ) ) ;
#11941 = CARTESIAN_POINT ( 'NONE',  ( 4.630844611799306954, -31.48367946546115803, 6.951256099901584662 ) ) ;
#11942 = CYLINDRICAL_SURFACE ( 'NONE', #16478, 1.000000000000000000 ) ;
#11943 = DIRECTION ( 'NONE',  ( -0.000000000000000000, -0.000000000000000000, 1.000000000000000000 ) ) ;
#11944 = CARTESIAN_POINT ( 'NONE',  ( -70.73213213501304608, -45.61702805680359063, 6.000000000000001776 ) ) ;
#11945 = ORIENTED_EDGE ( 'NONE', *, *, #27413, .T. ) ;
#11946 = CARTESIAN_POINT ( 'NONE',  ( 35.70145850010435140, -1.358481403853448732, 5.583794832904679595 ) ) ;
#11947 = CARTESIAN_POINT ( 'NONE',  ( -71.14735168035940660, 0.1989745095792901375, 3.997008894667205769 ) ) ;
#11948 = CARTESIAN_POINT ( 'NONE',  ( 66.88492799900151908, 57.87961537897388808, -3.998747512900713730 ) ) ;
#11949 = DIRECTION ( 'NONE',  ( 0.1303762246624232679, -0.7394003126383936753, 0.6605219282605379050 ) ) ;
#11950 = ORIENTED_EDGE ( 'NONE', *, *, #33196, .F. ) ;
#11951 = CARTESIAN_POINT ( 'NONE',  ( -7.890026461918812295, -6.626103207857777159E-16, 6.000000000000000000 ) ) ;
#11952 = FACE_OUTER_BOUND ( 'NONE', #19250, .T. ) ;
#11953 = CARTESIAN_POINT ( 'NONE',  ( -38.97867591359219119, -26.64985754041175525, 6.700000000000000178 ) ) ;
#11954 = ORIENTED_EDGE ( 'NONE', *, *, #39255, .T. ) ;
#11955 = CARTESIAN_POINT ( 'NONE',  ( 0.000000000000000000, 13.37661300689600097, 6.000000000000000000 ) ) ;
#11956 = DIRECTION ( 'NONE',  ( 1.000000000000000000, 0.000000000000000000, -0.000000000000000000 ) ) ;
#11957 = ORIENTED_EDGE ( 'NONE', *, *, #14605, .F. ) ;
#11958 = CARTESIAN_POINT ( 'NONE',  ( 22.21046374329029405, 5.169589464359284570, 3.137441446710924620 ) ) ;
#11959 = CARTESIAN_POINT ( 'NONE',  ( 80.71704827558885142, 66.21292280724347279, -1.000000000000000000 ) ) ;
#11960 = CARTESIAN_POINT ( 'NONE',  ( -4.266520354791871306, -48.67644278316300444, 6.000000000000000000 ) ) ;
#11961 = CARTESIAN_POINT ( 'NONE',  ( 81.11033257497912530, 61.28231361833088897, 1.235082213173759547 ) ) ;
#11962 = CARTESIAN_POINT ( 'NONE',  ( 2.829405163535267942, -26.36285597610873310, 7.695279973900954751 ) ) ;
#11963 = ORIENTED_EDGE ( 'NONE', *, *, #34569, .F. ) ;
#11964 = CARTESIAN_POINT ( 'NONE',  ( 76.91271350297704146, 62.89131350122335817, -3.776276000685965251 ) ) ;
#11965 = B_SPLINE_CURVE_WITH_KNOTS ( 'NONE', 3,
 ( #31097, #3325, #28612, #28401, #6787, #208, #24706 ),
 .UNSPECIFIED., .F., .F.,
 ( 4, 3, 4 ),
 ( 0.006904927062941951937, 0.007395461772899652141, 0.008026723377514808841 ),
 .UNSPECIFIED. ) ;
#11966 = CARTESIAN_POINT ( 'NONE',  ( 3.877683203921740596, -32.29717309340981757, 7.780491323090171996 ) ) ;
#11967 = CARTESIAN_POINT ( 'NONE',  ( -70.92837670882107659, 28.72470171467712063, -6.000000000000005329 ) ) ;
#11968 = CARTESIAN_POINT ( 'NONE',  ( 78.81184074671398321, 66.10527324714774977, -1.416821487223371978 ) ) ;
#11969 = PRODUCT_RELATED_PRODUCT_CATEGORY ( 'part', '', ( #8239 ) ) ;
#11970 = CARTESIAN_POINT ( 'NONE',  ( 79.19973406752559697, 61.05435877263168720, 2.913524936157070755 ) ) ;
#11971 = VECTOR ( 'NONE', #37939, 1000.000000000000000 ) ;
#11972 = CARTESIAN_POINT ( 'NONE',  ( -17.69482985384421880, -29.56993018339339940, 6.000000000000000000 ) ) ;
#11973 = ORIENTED_EDGE ( 'NONE', *, *, #3214, .F. ) ;
#11974 = CARTESIAN_POINT ( 'NONE',  ( 80.30118292188606688, 66.27423127454436269, 1.564050819713522777 ) ) ;
#11977 = EDGE_LOOP ( 'NONE', ( #31554, #25764, #34651, #30185, #29918 ) ) ;
#11976 = CARTESIAN_POINT ( 'NONE',  ( -1.699138637657512829, -29.51332269405392239, 6.887041543973317026 ) ) ;
#11975 = CARTESIAN_POINT ( 'NONE',  ( 1.700390093233090871, -29.56993018339339940, 7.800000000000000711 ) ) ;
#11978 = CARTESIAN_POINT ( 'NONE',  ( 29.24730582455742578, -0.4004845594861357605, -5.905559009470326970 ) ) ;
#11979 = CARTESIAN_POINT ( 'NONE',  ( 14.70571656306172237, -5.036098275607509223, -2.499999999999940492 ) ) ;
#11980 = CARTESIAN_POINT ( 'NONE',  ( -1.649141860557009176, -30.19362195415678229, 7.257242401810564125 ) ) ;
#11981 = CARTESIAN_POINT ( 'NONE',  ( -64.46937875527800088, 36.54399046018752273, 5.728582434991126071 ) ) ;
#11982 = EDGE_CURVE ( 'NONE', #11093, #35794, #36088, .T. ) ;
#11983 = DIRECTION ( 'NONE',  ( 0.000000000000000000, 0.000000000000000000, -1.000000000000000000 ) ) ;
#11984 = FACE_OUTER_BOUND ( 'NONE', #15720, .T. ) ;
#11985 = FACE_OUTER_BOUND ( 'NONE', #39100, .T. ) ;
#11986 = EDGE_CURVE ( 'NONE', #17221, #10017, #17817, .T. ) ;
#11987 = CARTESIAN_POINT ( 'NONE',  ( 5.152995580017100785, -30.14397416824791165, 7.674970859709603133 ) ) ;
#11988 = CARTESIAN_POINT ( 'NONE',  ( 37.13786913975418713, -2.596535722758734011, -5.986194934020763192 ) ) ;
#11989 = CARTESIAN_POINT ( 'NONE',  ( 3.364361873418217463, -32.64093995024074957, 7.776484688137385248 ) ) ;
#11990 = FACE_BOUND ( 'NONE', #21791, .T. ) ;
#11991 = CARTESIAN_POINT ( 'NONE',  ( 5.042305363714541855, -28.94414881188822619, 7.695279973900954751 ) ) ;
#11992 = CARTESIAN_POINT ( 'NONE',  ( 0.4601917647012155888, -32.82718141592015115, 7.785344483711591934 ) ) ;
#11993 = LINE ( 'NONE', #37124, #19420 ) ;
#11994 = DIRECTION ( 'NONE',  ( 0.000000000000000000, 1.000000000000000000, 0.000000000000000000 ) ) ;
#11995 = CARTESIAN_POINT ( 'NONE',  ( -62.89172142731304405, 37.18122596373097366, -4.326867315595535501 ) ) ;
#11996 = CARTESIAN_POINT ( 'NONE',  ( 21.42317272044189735, 8.032848918686916306, 2.736807373248377750 ) ) ;
#11997 = CARTESIAN_POINT ( 'NONE',  ( 23.80152365654308610, 2.314069967681273710, -4.322128912501145948 ) ) ;
#11998 = CARTESIAN_POINT ( 'NONE',  ( -1.538375173488943259, -30.60457953059374248, 6.865312560952604670 ) ) ;
#11999 = VERTEX_POINT ( 'NONE', #22971 ) ;
#12000 =( NAMED_UNIT ( * ) PLANE_ANGLE_UNIT ( ) SI_UNIT ( $, .RADIAN. ) );
#12001 = CARTESIAN_POINT ( 'NONE',  ( 70.90076320674430121, 59.58500768881799559, -3.976054184260641833 ) ) ;
#12002 = VECTOR ( 'NONE', #38758, 1000.000000000000000 ) ;
#12003 = ORIENTED_EDGE ( 'NONE', *, *, #10907, .T. ) ;
#12004 = CYLINDRICAL_SURFACE ( 'NONE', #12733, 3.399999999999999911 ) ;
#12005 = FACE_OUTER_BOUND ( 'NONE', #33609, .T. ) ;
#12006 = CARTESIAN_POINT ( 'NONE',  ( 69.84993430378905543, 58.85661355152254970, 3.977789803233258148 ) ) ;
#12007 = DIRECTION ( 'NONE',  ( 1.000000000000000000, 0.000000000000000000, 0.000000000000000000 ) ) ;
#12008 = CARTESIAN_POINT ( 'NONE',  ( -13.07867591359219617, -26.64985754041175525, 6.700000000000000178 ) ) ;
#12009 = ADVANCED_FACE ( 'NONE', ( #35534 ), #31832, .F. ) ;
#12010 = CONTEXT_DEPENDENT_SHAPE_REPRESENTATION ( #10286, #8832 ) ;
#12011 = CARTESIAN_POINT ( 'NONE',  ( -1.425108829345238082, -28.21376964069959925, 7.386948897581449458 ) ) ;
#12012 = VERTEX_POINT ( 'NONE', #38188 ) ;
#12013 = CARTESIAN_POINT ( 'NONE',  ( 22.18530337611392511, 5.286255035602901664, 3.058813682531833500 ) ) ;
#12014 = DIRECTION ( 'NONE',  ( 0.000000000000000000, 0.000000000000000000, 1.000000000000000000 ) ) ;
#12015 = CARTESIAN_POINT ( 'NONE',  ( 22.14520323347436204, -3.079061112527371247, 3.566016265539754482 ) ) ;
#12016 = ORIENTED_EDGE ( 'NONE', *, *, #315, .T. ) ;
#12017 = CARTESIAN_POINT ( 'NONE',  ( 80.72339804071911828, 61.33444547702553962, -2.197205184446166637 ) ) ;
#12018 = CARTESIAN_POINT ( 'NONE',  ( -7.078675913592194391, -24.55319635012989110, 6.800000000000000711 ) ) ;
#12019 = CARTESIAN_POINT ( 'NONE',  ( 81.40473435056793505, 64.45019880697486769, -3.071899782094857034 ) ) ;
#12020 = CARTESIAN_POINT ( 'NONE',  ( 78.85457743492895588, 65.01671056748381261, 3.151254463354984825 ) ) ;
#12021 = EDGE_CURVE ( 'NONE', #7186, #3289, #35139, .T. ) ;
#12022 = DIRECTION ( 'NONE',  ( -0.000000000000000000, 0.000000000000000000, 1.000000000000000000 ) ) ;
#12023 = CARTESIAN_POINT ( 'NONE',  ( -0.9304231601246585326, -27.40494118565320392, 7.257242401810566790 ) ) ;
#12024 = CARTESIAN_POINT ( 'NONE',  ( 21.85643539959777470, 6.775053487808889940, 8.548204544396675431 ) ) ;
#12025 = VERTEX_POINT ( 'NONE', #39962 ) ;
#12026 = CARTESIAN_POINT ( 'NONE',  ( -78.25131871557718455, 11.30516684399499816, 6.821579343738465084 ) ) ;
#12027 = VECTOR ( 'NONE', #26173, 1000.000000000000000 ) ;
#12028 = DIRECTION ( 'NONE',  ( -0.1736481776669174526, -0.9848077530122102408, 0.000000000000000000 ) ) ;
#12029 = PLANE ( 'NONE',  #10328 ) ;
#12030 = CARTESIAN_POINT ( 'NONE',  ( 1.660390578422507035, -32.96970878852050646, 7.784838882742139532 ) ) ;
#12031 = EDGE_CURVE ( 'NONE', #5730, #18458, #5850, .T. ) ;
#12032 = CARTESIAN_POINT ( 'NONE',  ( 28.28109443870617312, -3.657712271061086540, -4.586391589056719731 ) ) ;
#12033 = CARTESIAN_POINT ( 'NONE',  ( 32.06979358023967563, 0.2538423115740326419, -4.725469285452410517 ) ) ;
#12034 = CARTESIAN_POINT ( 'NONE',  ( 3.733953510012606891, -32.29475398685401899, 7.006423389747790331 ) ) ;
#12035 = CARTESIAN_POINT ( 'NONE',  ( 15.64340809456564152, 11.14027857853738013, 2.614319631236162511 ) ) ;
#12036 = CARTESIAN_POINT ( 'NONE',  ( 5.113812245512664667, -30.34358980514384285, 7.013842709614101167 ) ) ;
#12037 = PLANE ( 'NONE',  #34551 ) ;
#12038 = CARTESIAN_POINT ( 'NONE',  ( 5.045426396246663003, -28.96105241937069152, 7.748216051605119503 ) ) ;
#12039 = AXIS2_PLACEMENT_3D ( 'NONE', #33460, #14073, #8294 ) ;
#12040 = CARTESIAN_POINT ( 'NONE',  ( 18.45497827215059772, 13.28099812781043276, -2.500000000000000000 ) ) ;
#12041 = CARTESIAN_POINT ( 'NONE',  ( 36.94473691932590498, -2.175944540167862762, -5.891203402125550603 ) ) ;
#12042 = CARTESIAN_POINT ( 'NONE',  ( 24.47644591641656220, 2.965209954150327842, -3.650517593455100407 ) ) ;
#12043 = VERTEX_POINT ( 'NONE', #40159 ) ;
#12044 = CARTESIAN_POINT ( 'NONE',  ( 66.98823442903206171, 58.05250069757015297, 3.998791315154375692 ) ) ;
#12045 = CARTESIAN_POINT ( 'NONE',  ( 35.33694189094937599, -3.445746785322538308, 5.711001300648953283 ) ) ;
#12046 = CARTESIAN_POINT ( 'NONE',  ( 4.969183729906043290, -30.78936915658119489, 7.781480525794718162 ) ) ;
#12047 = VECTOR ( 'NONE', #8516, 1000.000000000000000 ) ;
#12048 = DIRECTION ( 'NONE',  ( -0.000000000000000000, -0.000000000000000000, 1.000000000000000000 ) ) ;
#12049 = CARTESIAN_POINT ( 'NONE',  ( 84.83925925549863223, 2.817044135119172399, -2.844581780382558378 ) ) ;
#12051 = CARTESIAN_POINT ( 'NONE',  ( 34.16812880522524409, -3.144588050804470125, -5.539160878010015665 ) ) ;
#12050 = CARTESIAN_POINT ( 'NONE',  ( -71.72841970756384455, -21.39719814140381615, 5.947160319466099132 ) ) ;
#12052 = CARTESIAN_POINT ( 'NONE',  ( -1.559314410350653546, -30.53653586789760865, 6.929923840112069300 ) ) ;
#12053 = ORIENTED_EDGE ( 'NONE', *, *, #28783, .T. ) ;
#12054 = FACE_OUTER_BOUND ( 'NONE', #32062, .T. ) ;
#12055 = EDGE_CURVE ( 'NONE', #5814, #19731, #3149, .T. ) ;
#12056 = DIRECTION ( 'NONE',  ( 0.000000000000000000, 1.000000000000000000, 0.000000000000000000 ) ) ;
#12057 = ORIENTED_EDGE ( 'NONE', *, *, #14327, .T. ) ;
#12058 = DIRECTION ( 'NONE',  ( 1.000000000000000000, 0.000000000000000000, -0.000000000000000000 ) ) ;
#12059 = ORIENTED_EDGE ( 'NONE', *, *, #14968, .F. ) ;
#12060 = CARTESIAN_POINT ( 'NONE',  ( 80.36115745751311579, 63.17601289530517761, -3.638935937159312850 ) ) ;
#12061 = B_SPLINE_CURVE_WITH_KNOTS ( 'NONE', 3,
 ( #14521, #1791, #8339, #11222, #23990, #23601, #32879, #14936, #4669, #14320, #18018, #1586, #36165, #39639, #27291, #21129, #23788, #36365, #7944, #20496, #30181, #4862, #33287, #5068, #36763, #36560, #17601, #27093, #20914, #5269, #17810 ),
 .UNSPECIFIED., .F., .F.,
 ( 4, 3, 3, 3, 3, 3, 3, 3, 3, 3, 4 ),
 ( 0.000000000000000000, 3.077658087705648207E-05, 6.152638666998854248E-05, 9.267501192706494300E-05, 0.0001241882240135190358, 0.0001556618703051665289, 0.0001866161554452196744, 0.0002167966385860968731, 0.0002463805737537766763, 0.0002758761370306527069, 0.0002847094172290049949 ),
 .UNSPECIFIED. ) ;
#12062 = EDGE_CURVE ( 'NONE', #40343, #9636, #9440, .T. ) ;
#12063 = CARTESIAN_POINT ( 'NONE',  ( -1.567987374133025247, -28.31781895025901008, 6.873189335546978640 ) ) ;
#12064 = CARTESIAN_POINT ( 'NONE',  ( 80.52560336917662198, 62.91486207252171425, 3.518158556798114400 ) ) ;
#12066 = VERTEX_POINT ( 'NONE', #36874 ) ;
#12065 = CARTESIAN_POINT ( 'NONE',  ( -63.99293516169446150, 35.89893413629672381, -46.17089178453873188 ) ) ;
#12067 = B_SPLINE_CURVE_WITH_KNOTS ( 'NONE', 3,
 ( #19039, #31601, #24810, #9554, #6886, #37351, #28090, #9145, #37550, #21926, #34500, #3224, #9765, #12849, #6274, #18822, #15740, #15935, #22345, #521, #13054, #34915, #22546, #35108, #31804, #3618, #16146, #25616, #16939, #19646, #7685 ),
 .UNSPECIFIED., .F., .F.,
 ( 4, 3, 3, 3, 3, 3, 3, 3, 3, 3, 4 ),
 ( 0.000000000000000000, 2.999644130997671654E-05, 6.002588995694646388E-05, 8.960886084588062241E-05, 0.0001190604700446481443, 0.0001489538463052721812, 0.0001796139255494020562, 0.0002109707048517091657, 0.0002426195318110370642, 0.0002740640997890078645, 0.0002849778069099885396 ),
 .UNSPECIFIED. ) ;
#12068 = EDGE_CURVE ( 'NONE', #7879, #21734, #28856, .T. ) ;
#12069 = AXIS2_PLACEMENT_3D ( 'NONE', #33756, #40310, #5945 ) ;
#12070 = CARTESIAN_POINT ( 'NONE',  ( 74.30428547378053850, 61.12304205247700395, -3.924711207976832927 ) ) ;
#12071 = VECTOR ( 'NONE', #4948, 1000.000000000000000 ) ;
#12072 = CARTESIAN_POINT ( 'NONE',  ( 3.327612781436851463, -32.55525199569353134, 6.870716933885663735 ) ) ;
#12074 = CARTESIAN_POINT ( 'NONE',  ( 24.52423802077814585, -6.127131655257791465, 2.764126198674226931 ) ) ;
#12073 = CARTESIAN_POINT ( 'NONE',  ( -26.34874870218063947, -26.64985754041175525, 6.700000000000000178 ) ) ;
#12075 = CARTESIAN_POINT ( 'NONE',  ( 1.646239191775039412, -25.86893018339335981, 7.695279973900954751 ) ) ;
#12076 = CARTESIAN_POINT ( 'NONE',  ( 0.1778422052069661419, -26.52201895416361310, 7.386948897581448570 ) ) ;
#12077 = CARTESIAN_POINT ( 'NONE',  ( 24.34606147761258654, 3.138786336531333099, -3.389104778623087455 ) ) ;
#12078 = VERTEX_POINT ( 'NONE', #18328 ) ;
#12079 = CARTESIAN_POINT ( 'NONE',  ( -2.965417489341782176, -27.61323101669772484, 6.894806418505347700 ) ) ;
#12080 = AXIS2_PLACEMENT_3D ( 'NONE', #15729, #28281, #6264 ) ;
#12081 = CARTESIAN_POINT ( 'NONE',  ( 24.03893326528611141, 2.664202206450044130, -5.290213626918107259 ) ) ;
#12082 = CARTESIAN_POINT ( 'NONE',  ( 20.30405589181014747, 6.129815107149093834, 3.484773800364461938 ) ) ;
#12083 = EDGE_CURVE ( 'NONE', #713, #32955, #33606, .T. ) ;
#12084 = CARTESIAN_POINT ( 'NONE',  ( 5.006586777994688653, -30.36307495321339900, 6.979335674598005745 ) ) ;
#12085 = CARTESIAN_POINT ( 'NONE',  ( 79.52751932686963698, 65.84655314362326806, 2.556731990914093533 ) ) ;
#12086 = CARTESIAN_POINT ( 'NONE',  ( 86.42019152727894493, 0.2271775462534226520, 6.017476335466618309 ) ) ;
#12087 = CARTESIAN_POINT ( 'NONE',  ( 15.06184329234986663, 12.12621205208998987, 2.536020854430098836 ) ) ;
#12088 = ORIENTED_EDGE ( 'NONE', *, *, #10235, .F. ) ;
#12089 = CARTESIAN_POINT ( 'NONE',  ( 1.700390093233090871, -29.56993018339339940, 7.800000000000000711 ) ) ;
#12090 = CARTESIAN_POINT ( 'NONE',  ( 4.624684975110706198, -31.30446008192196317, 7.784838882742139532 ) ) ;
#12091 = ORIENTED_EDGE ( 'NONE', *, *, #24798, .F. ) ;
#12092 = CARTESIAN_POINT ( 'NONE',  ( -26.97867591359219475, -26.64985754041175525, 6.700000000000000178 ) ) ;
#12093 = FACE_OUTER_BOUND ( 'NONE', #18948, .T. ) ;
#12094 = CARTESIAN_POINT ( 'NONE',  ( -28.34874870218063947, -25.49307895267003587, 6.800000000000000711 ) ) ;
#12095 = PLANE ( 'NONE',  #19602 ) ;
#12096 = EDGE_LOOP ( 'NONE', ( #15293, #24510, #10450, #29370, #15732, #20483, #38020, #7661, #34594, #15314, #28070, #18705, #36792, #26521, #26071, #9746, #21794, #20028 ) ) ;
#12097 = CARTESIAN_POINT ( 'NONE',  ( 37.04568408393004830, -2.800967617106917551, 5.988272973189237902 ) ) ;
#12098 = AXIS2_PLACEMENT_3D ( 'NONE', #723, #28096, #34921 ) ;
#12099 = CARTESIAN_POINT ( 'NONE',  ( 85.94962389285764459, 1.815027625006768730, -4.252598035848374813 ) ) ;
#12100 = ORIENTED_EDGE ( 'NONE', *, *, #1837, .T. ) ;
#12102 = CARTESIAN_POINT ( 'NONE',  ( 36.87190381947284123, -2.085833083560729051, 5.863581891243574873 ) ) ;
#12101 = CARTESIAN_POINT ( 'NONE',  ( 79.42405716688904249, 65.78352207363049331, -2.615128354545405376 ) ) ;
#12103 = CARTESIAN_POINT ( 'NONE',  ( 23.67457366230596705, -2.672207667981083112, 3.901387810367294762 ) ) ;
#12104 = CARTESIAN_POINT ( 'NONE',  ( 21.39126609848262817, -3.058903647210607701, -3.458430474917000286 ) ) ;
#12105 = CARTESIAN_POINT ( 'NONE',  ( -2.878675913592191993, -26.64985754041175525, 6.700000000000000178 ) ) ;
#12106 = ORIENTED_EDGE ( 'NONE', *, *, #39787, .T. ) ;
#12107 = AXIS2_PLACEMENT_3D ( 'NONE', #39596, #21284, #2366 ) ;
#12108 = VERTEX_POINT ( 'NONE', #15045 ) ;
#12109 = EDGE_CURVE ( 'NONE', #446, #36272, #27605, .T. ) ;
#12110 = ORIENTED_EDGE ( 'NONE', *, *, #16718, .T. ) ;
#12111 = CARTESIAN_POINT ( 'NONE',  ( 81.13619541807486257, 61.97540048441254612, -2.718470589328601417 ) ) ;
#12112 =( BOUNDED_CURVE ( )  B_SPLINE_CURVE ( 3, ( #9522, #28681, #19010, #491 ),
 .UNSPECIFIED., .F., .T. ) 
 B_SPLINE_CURVE_WITH_KNOTS ( ( 4, 4 ),
 ( 1.381924640371167357, 1.574767692156076482 ),
 .UNSPECIFIED. ) 
 CURVE ( )  GEOMETRIC_REPRESENTATION_ITEM ( )  RATIONAL_B_SPLINE_CURVE ( ( 1.000000000000000000, 0.9969033633783032089, 0.9969033633783032089, 1.000000000000000000 ) ) 
 REPRESENTATION_ITEM ( '' )  );
#12113 = CARTESIAN_POINT ( 'NONE',  ( -59.14838763364237906, 27.28340689960984733, -4.628958989307211169 ) ) ;
#12114 = ADVANCED_FACE ( 'NONE', ( #30503 ), #1908, .F. ) ;
#12115 = ORIENTED_EDGE ( 'NONE', *, *, #3388, .T. ) ;
#12117 = CARTESIAN_POINT ( 'NONE',  ( 31.38403718649578877, 0.5068638959182734105, 4.596961181239236360 ) ) ;
#12116 = CARTESIAN_POINT ( 'NONE',  ( 22.91664155360341937, 2.744262553797580217, 4.428644351404614987 ) ) ;
#12118 = VERTEX_POINT ( 'NONE', #2726 ) ;
#12119 = EDGE_CURVE ( 'NONE', #39349, #38890, #21443, .T. ) ;
#12120 = CARTESIAN_POINT ( 'NONE',  ( 81.94417840557096611, 63.58970459987528301, -2.726953404243311230 ) ) ;
#12121 = PRODUCT_RELATED_PRODUCT_CATEGORY ( 'part', '', ( #4229 ) ) ;
#12122 = CARTESIAN_POINT ( 'NONE',  ( -15.07867591359219439, -26.64985754041175525, 6.800000000000000711 ) ) ;
#12123 = ORIENTED_EDGE ( 'NONE', *, *, #36221, .F. ) ;
#12125 = LINE ( 'NONE', #34813, #15728 ) ;
#12124 = DIRECTION ( 'NONE',  ( 0.000000000000000000, 0.000000000000000000, 1.000000000000000000 ) ) ;
#12126 = CYLINDRICAL_SURFACE ( 'NONE', #805, 8.080217238368755162 ) ;
#12127 = CARTESIAN_POINT ( 'NONE',  ( -64.08758708074093136, 42.49068820928864199, -3.479708933549301442 ) ) ;
#12128 = CARTESIAN_POINT ( 'NONE',  ( 73.38675137958711048, 60.10977650211887635, 3.914122288815133910 ) ) ;
#12129 = EDGE_CURVE ( 'NONE', #8931, #7569, #23163, .T. ) ;
#12130 = CARTESIAN_POINT ( 'NONE',  ( 22.85242861330229047, 3.166249937094171685, -4.146800157721144409 ) ) ;
#12131 = VERTEX_POINT ( 'NONE', #26998 ) ;
#12132 = CARTESIAN_POINT ( 'NONE',  ( 0.5099477558868652505, -26.38514651076292239, 7.661510568013098599 ) ) ;
#12133 =( GEOMETRIC_REPRESENTATION_CONTEXT ( 3 ) GLOBAL_UNCERTAINTY_ASSIGNED_CONTEXT ( ( #37395 ) ) GLOBAL_UNIT_ASSIGNED_CONTEXT ( ( #23354, #25840, #32429 ) ) REPRESENTATION_CONTEXT ( 'NONE', 'WORKASPACE' ) );
#12134 = CARTESIAN_POINT ( 'NONE',  ( 21.85643539959772497, -14.97654459006671068, 3.851724272136834326 ) ) ;
#12135 = AXIS2_PLACEMENT_3D ( 'NONE', #21790, #5520, #12508 ) ;
#12136 = CARTESIAN_POINT ( 'NONE',  ( 1.700390093233090871, -29.56993018339339940, 7.800000000000000711 ) ) ;
#12137 = ORIENTED_EDGE ( 'NONE', *, *, #12369, .F. ) ;
#12138 = CARTESIAN_POINT ( 'NONE',  ( 81.51618470504207892, 61.58087653888393476, 1.588372325568258914 ) ) ;
#12139 = AXIS2_PLACEMENT_3D ( 'NONE', #17558, #27053, #39598 ) ;
#12140 = CARTESIAN_POINT ( 'NONE',  ( 88.43294427370824451, -0.9743556922601576131, -2.623293804462837553 ) ) ;
#12141 = DIRECTION ( 'NONE',  ( 0.000000000000000000, 0.000000000000000000, 1.000000000000000000 ) ) ;
#12142 = AXIS2_PLACEMENT_3D ( 'NONE', #37486, #21859, #34435 ) ;
#12143 = CARTESIAN_POINT ( 'NONE',  ( -64.08758708074093136, 38.13199975834322686, 3.043809435734686097 ) ) ;
#12144 = EDGE_LOOP ( 'NONE', ( #30053, #34620, #27704, #23254 ) ) ;
#12145 = CARTESIAN_POINT ( 'NONE',  ( 18.25296777573797513, -2.941843506369077321, 3.053268232905335555 ) ) ;
#12146 = CARTESIAN_POINT ( 'NONE',  ( 25.01091293555841233, 3.329590545877085805, 1.936828124349011526 ) ) ;
#12147 = CARTESIAN_POINT ( 'NONE',  ( 37.04431342567128382, -2.893185755689349214, -5.988059048818550778 ) ) ;
#12148 = CARTESIAN_POINT ( 'NONE',  ( 5.098360399818202993, -29.68741740107808980, 7.759451378593097637 ) ) ;
#12149 = CARTESIAN_POINT ( 'NONE',  ( 4.666673777302699833, -31.42768917297451026, 6.867199677474199682 ) ) ;
#12150 = EDGE_LOOP ( 'NONE', ( #1013, #21347, #12642, #7209 ) ) ;
#12151 = FACE_OUTER_BOUND ( 'NONE', #14199, .T. ) ;
#12152 = B_SPLINE_CURVE_WITH_KNOTS ( 'NONE', 3,
 ( #36516, #30550, #14879, #15297, #2362, #2771, #39382, #1954, #23745, #17759, #30346, #2152, #11577, #5634 ),
 .UNSPECIFIED., .F., .F.,
 ( 4, 2, 2, 2, 2, 2, 4 ),
 ( 0.007044848506661660799, 0.007338175092571547382, 0.007631501678481433099, 0.007924828264391319682, 0.008218154850301206266, 0.008804808022120993310, 0.009391461193940780355 ),
 .UNSPECIFIED. ) ;
#12153 = CARTESIAN_POINT ( 'NONE',  ( 3.651251297819360531, -26.64985754041175525, 6.700000000000000178 ) ) ;
#12154 = DIRECTION ( 'NONE',  ( 0.000000000000000000, 0.000000000000000000, 1.000000000000000000 ) ) ;
#12155 = ORIENTED_EDGE ( 'NONE', *, *, #19678, .T. ) ;
#12156 = CARTESIAN_POINT ( 'NONE',  ( 27.78114228934722618, 1.798550533532914830, 4.024392981447666884 ) ) ;
#12157 = FACE_OUTER_BOUND ( 'NONE', #3154, .T. ) ;
#12158 = ORIENTED_EDGE ( 'NONE', *, *, #25933, .T. ) ;
#12159 = CARTESIAN_POINT ( 'NONE',  ( 66.90849722842033032, 57.81418058710544727, -3.996206253853811674 ) ) ;
#12160 = EDGE_CURVE ( 'NONE', #9154, #2808, #7479, .T. ) ;
#12161 = CARTESIAN_POINT ( 'NONE',  ( -0.5207487492606875934, -26.87946823591146384, 7.781480525794719050 ) ) ;
#12162 = CIRCLE ( 'NONE', #31269, 0.1000000000000028644 ) ;
#12163 = VERTEX_POINT ( 'NONE', #14624 ) ;
#12164 = AXIS2_PLACEMENT_3D ( 'NONE', #14791, #2485, #1865 ) ;
#12165 = CARTESIAN_POINT ( 'NONE',  ( 88.35472856589244373, -0.8865000968999163788, -0.8281635480601134969 ) ) ;
#12166 = ADVANCED_FACE ( 'NONE', ( #27197 ), #39755, .F. ) ;
#12167 = CARTESIAN_POINT ( 'NONE',  ( -71.85905498853752249, 3.863100500280893357, -9.956904411795710175 ) ) ;
#12168 = DIRECTION ( 'NONE',  ( -0.000000000000000000, -1.000000000000000000, -0.000000000000000000 ) ) ;
#12169 = CARTESIAN_POINT ( 'NONE',  ( -65.04872026876938662, 34.92042435966252611, 6.752913741461252783 ) ) ;
#12170 = ORIENTED_EDGE ( 'NONE', *, *, #3489, .T. ) ;
#12171 = CARTESIAN_POINT ( 'NONE',  ( 1.700390093233090871, -29.56993018339339940, 6.800000000000000711 ) ) ;
#12172 = LINE ( 'NONE', #12583, #21223 ) ;
#12173 = VERTEX_POINT ( 'NONE', #40356 ) ;
#12174 = CARTESIAN_POINT ( 'NONE',  ( 23.14578216353262263, 3.986807833658514877, 3.175358570212865938 ) ) ;
#12175 = EDGE_CURVE ( 'NONE', #9750, #17561, #37392, .T. ) ;
#12176 = CARTESIAN_POINT ( 'NONE',  ( 80.38645948019593845, 66.31981033314001195, -1.000000000000000000 ) ) ;
#12177 = CARTESIAN_POINT ( 'NONE',  ( 80.27036958223403929, 63.85842528439429344, 3.661914029440276774 ) ) ;
#12178 = EDGE_CURVE ( 'NONE', #16241, #8875, #22236, .T. ) ;
#12179 = CARTESIAN_POINT ( 'NONE',  ( -0.04839779602465103803, -32.48570468057000227, 6.887041543973315250 ) ) ;
#12180 = ORIENTED_EDGE ( 'NONE', *, *, #4839, .T. ) ;
#12181 = CARTESIAN_POINT ( 'NONE',  ( 77.16059773406421129, 63.78117330919809547, -3.480716904142247881 ) ) ;
#12183 = LINE ( 'NONE', #37497, #38140 ) ;
#12182 = CARTESIAN_POINT ( 'NONE',  ( 3.863278594513700259, -32.31834595185378589, 7.766640943994342905 ) ) ;
#12184 = CARTESIAN_POINT ( 'NONE',  ( 0.5402140142766861386, -26.37399660057016604, 7.769368695748487319 ) ) ;
#12185 = CARTESIAN_POINT ( 'NONE',  ( 81.11561130678553866, 63.91242180913142334, -3.402511877377342397 ) ) ;
#12186 = CARTESIAN_POINT ( 'NONE',  ( -0.8065408690586024498, -32.02206539088906112, 7.501983001166816933 ) ) ;
#12187 = CARTESIAN_POINT ( 'NONE',  ( 78.25991397077970646, 61.55280089391300891, 3.597602401604638178 ) ) ;
#12188 = ORIENTED_EDGE ( 'NONE', *, *, #9670, .F. ) ;
#12189 = CARTESIAN_POINT ( 'NONE',  ( 1.870512271622051026, -32.97271924194787829, 7.139196562012272373 ) ) ;
#12190 = ORIENTED_EDGE ( 'NONE', *, *, #25306, .T. ) ;
#12191 = CARTESIAN_POINT ( 'NONE',  ( -63.08758708074093136, 38.76906266698303227, 3.000000000000000000 ) ) ;
#12192 = CARTESIAN_POINT ( 'NONE',  ( 80.93658766080277189, 66.04709959793324003, 1.728104186157678468 ) ) ;
#12194 = CARTESIAN_POINT ( 'NONE',  ( -1.693328789480683216, -29.36335781081668017, 6.929923840112063971 ) ) ;
#12193 = CARTESIAN_POINT ( 'NONE',  ( -70.92837670882107659, -47.11702805680359063, 38.00000000000000711 ) ) ;
#12195 = CARTESIAN_POINT ( 'NONE',  ( 28.53445731760455573, 0.6922391713037714389, -5.301755952056612209 ) ) ;
#12196 = CARTESIAN_POINT ( 'NONE',  ( -1.346119371218626792, -31.29294500718514271, 6.894806418505347700 ) ) ;
#12197 = CARTESIAN_POINT ( 'NONE',  ( 1.751251297819361730, -26.64985754041175525, 6.800000000000000711 ) ) ;
#12198 = CARTESIAN_POINT ( 'NONE',  ( -64.08758708074093136, 36.14363715547680300, 3.800414904976361807 ) ) ;
#12199 = CARTESIAN_POINT ( 'NONE',  ( 24.12590274031893856, 0.5209382751000486422, -5.092299414582193151 ) ) ;
#12200 = FACE_BOUND ( 'NONE', #24942, .T. ) ;
#12201 = VERTEX_POINT ( 'NONE', #9069 ) ;
#12202 = VECTOR ( 'NONE', #2414, 1000.000000000000000 ) ;
#12203 = CARTESIAN_POINT ( 'NONE',  ( -4.444218661349752963, -35.94265729135299381, 2.500000000000000000 ) ) ;
#12204 = VECTOR ( 'NONE', #22828, 1000.000000000000000 ) ;
#12205 = CARTESIAN_POINT ( 'NONE',  ( 81.06639586472026338, 61.26627432693234709, 1.317842247490183860 ) ) ;
#12206 = CARTESIAN_POINT ( 'NONE',  ( 36.10477245413083836, -1.582022789005378849, -5.680924181711803911 ) ) ;
#12207 = DIRECTION ( 'NONE',  ( 0.000000000000000000, 0.000000000000000000, -1.000000000000000000 ) ) ;
#12208 = CARTESIAN_POINT ( 'NONE',  ( 1.145429890469515932, -32.92433313672930240, 7.693875151218753317 ) ) ;
#12209 = CARTESIAN_POINT ( 'NONE',  ( -20.44874870218064444, -26.64985754041175525, 6.700000000000000178 ) ) ;
#12210 = CARTESIAN_POINT ( 'NONE',  ( 0.4370139710353302398, -32.82074954894827812, 7.782861076432731728 ) ) ;
#12211 = LINE ( 'NONE', #25999, #11481 ) ;
#12212 = CARTESIAN_POINT ( 'NONE',  ( 5.098819578411125875, -29.67379560486689982, 6.864651958020303368 ) ) ;
#12213 = AXIS2_PLACEMENT_3D ( 'NONE', #40263, #2834, #27912 ) ;
#12214 = DIRECTION ( 'NONE',  ( -0.000000000000000000, -0.000000000000000000, 1.000000000000000000 ) ) ;
#12215 = CARTESIAN_POINT ( 'NONE',  ( 2.839160670253830343, -26.36630475908082971, 7.652160403243387421 ) ) ;
#12216 = CARTESIAN_POINT ( 'NONE',  ( 25.04641388788620304, 2.159341827801565028, -4.144791871881564838 ) ) ;
#12217 = CARTESIAN_POINT ( 'NONE',  ( -30.97867591359219119, -26.64985754041175525, 6.700000000000000178 ) ) ;
#12218 = EDGE_LOOP ( 'NONE', ( #11748, #13280, #26442, #38304 ) ) ;
#12219 = LINE ( 'NONE', #24792, #27762 ) ;
#12220 = CARTESIAN_POINT ( 'NONE',  ( 70.66749459857992122, 60.15980271599462981, -3.887826097256385172 ) ) ;
#12221 = ORIENTED_EDGE ( 'NONE', *, *, #39276, .F. ) ;
#12222 = DIRECTION ( 'NONE',  ( -1.000000000000000000, 0.000000000000000000, 0.000000000000000000 ) ) ;
#12223 = CARTESIAN_POINT ( 'NONE',  ( 0.06461229748503910519, -26.58927154175672669, 6.874555630061441214 ) ) ;
#12224 = CARTESIAN_POINT ( 'NONE',  ( 1.163078168714447802, -26.21265396905771183, 6.889465824494257262 ) ) ;
#12226 = ADVANCED_FACE ( 'NONE', ( #16959 ), #26048, .F. ) ;
#12225 = CARTESIAN_POINT ( 'NONE',  ( 5.041572579232883378, -30.19968737494692235, 7.784838882742138644 ) ) ;
#12227 = ORIENTED_EDGE ( 'NONE', *, *, #26487, .T. ) ;
#12228 = CARTESIAN_POINT ( 'NONE',  ( 22.38229058954441797, 4.940558714326160228, 3.046107694943288813 ) ) ;
#12229 = EDGE_CURVE ( 'NONE', #30583, #16084, #8181, .T. ) ;
#12230 = CARTESIAN_POINT ( 'NONE',  ( 89.09355779190869384, 24.84364830758654108, 8.800414904976364028 ) ) ;
#12231 = B_SPLINE_CURVE_WITH_KNOTS ( 'NONE', 3,
 ( #3961, #18974, #19378, #658, #29051, #19585, #19174, #10301, #25558, #22878 ),
 .UNSPECIFIED., .F., .F.,
 ( 4, 3, 3, 4 ),
 ( 0.000000000000000000, 3.025505781527808535E-05, 6.051003801291533372E-05, 6.468145402690609117E-05 ),
 .UNSPECIFIED. ) ;
#12232 = CIRCLE ( 'NONE', #6980, 0.1000000000000028644 ) ;
#12233 = EDGE_CURVE ( 'NONE', #357, #16534, #1744, .T. ) ;
#12234 = ORIENTED_EDGE ( 'NONE', *, *, #19771, .T. ) ;
#12235 = CARTESIAN_POINT ( 'NONE',  ( 80.56990227295247564, 61.62418804268438066, -2.732428818688231065 ) ) ;
#12236 = FACE_OUTER_BOUND ( 'NONE', #33884, .T. ) ;
#12237 = CARTESIAN_POINT ( 'NONE',  ( 79.13116897371943992, 66.19293011460082710, -1.571309534768106086 ) ) ;
#12238 = CARTESIAN_POINT ( 'NONE',  ( 79.52562300987042931, 63.81209149333333386, 3.741985197832885301 ) ) ;
#12239 = VECTOR ( 'NONE', #33446, 1000.000000000000000 ) ;
#12240 = FACE_OUTER_BOUND ( 'NONE', #5495, .T. ) ;
#12241 = CARTESIAN_POINT ( 'NONE',  ( 2.778501328868240083, -32.79447296704462644, 7.778050822775631978 ) ) ;
#12242 = CARTESIAN_POINT ( 'NONE',  ( 21.85643539959776760, 7.937350203533870996, 6.559150378249414715 ) ) ;
#12243 = ORIENTED_EDGE ( 'NONE', *, *, #13933, .T. ) ;
#12244 = CARTESIAN_POINT ( 'NONE',  ( -75.05519143552835715, 9.687648905246064146, 9.110330305801273454 ) ) ;
#12245 = CARTESIAN_POINT ( 'NONE',  ( 36.65806048341712398, -3.481436136677176219, 5.844384006794087760 ) ) ;
#12246 = DIRECTION ( 'NONE',  ( 0.000000000000000000, -1.000000000000000000, -0.000000000000000000 ) ) ;
#12247 = ORIENTED_EDGE ( 'NONE', *, *, #5099, .F. ) ;
#12248 = FACE_OUTER_BOUND ( 'NONE', #34330, .T. ) ;
#12249 = CARTESIAN_POINT ( 'NONE',  ( 30.69560960875148581, -3.339038624481136974, -4.972551620578038012 ) ) ;
#12250 = CARTESIAN_POINT ( 'NONE',  ( 32.07043626334714759, 0.2549077454616246463, -4.723733316502016777 ) ) ;
#12251 = CARTESIAN_POINT ( 'NONE',  ( 3.720917640761610468, -32.30442619357121004, 6.959317978105168834 ) ) ;
#12252 = CARTESIAN_POINT ( 'NONE',  ( 15.42605057732512819, 10.99993330764380950, 2.614006291671366444 ) ) ;
#12253 = CARTESIAN_POINT ( 'NONE',  ( 1.749140210850987920, -26.17027969752984973, 6.894806418505346812 ) ) ;
#12254 = CARTESIAN_POINT ( 'NONE',  ( 29.66582406763757618, -3.796006116354329052, 4.435324138597246169 ) ) ;
#12255 = DIRECTION ( 'NONE',  ( 0.000000000000000000, 0.000000000000000000, 1.000000000000000000 ) ) ;
#12256 = CARTESIAN_POINT ( 'NONE',  ( -22.44874870218064089, -26.64985754041175525, 6.700000000000000178 ) ) ;
#12257 = CARTESIAN_POINT ( 'NONE',  ( 22.66896291849731071, 0.3171684538786420648, -6.422044740241496186 ) ) ;
#12258 = CARTESIAN_POINT ( 'NONE',  ( 36.82054380567017660, -2.045509829724917683, -5.849054631016336714 ) ) ;
#12259 = CARTESIAN_POINT ( 'NONE',  ( 26.12442444200497249, 1.901572713601228148, -4.234468824312982882 ) ) ;
#12260 = B_SPLINE_CURVE_WITH_KNOTS ( 'NONE', 3,
 ( #10362, #29309, #35500, #29701 ),
 .UNSPECIFIED., .F., .F.,
 ( 4, 4 ),
 ( 0.000000000000000000, 6.391136169993780466E-06 ),
 .UNSPECIFIED. ) ;
#12261 = EDGE_LOOP ( 'NONE', ( #16256, #37034, #20679, #24149 ) ) ;
#12262 = PRESENTATION_LAYER_ASSIGNMENT (  '', '', ( #35967 ) ) ;
#12263 = CARTESIAN_POINT ( 'NONE',  ( 67.45521008556633547, 58.13638817365040978, 3.998402061830689025 ) ) ;
#12264 = CARTESIAN_POINT ( 'NONE',  ( 36.91763012405728972, -3.049005243583072566, 5.968287055754437631 ) ) ;
#12265 = DIRECTION ( 'NONE',  ( 1.047444401652940007E-14, -1.000000000000000000, -0.000000000000000000 ) ) ;
#12266 = AXIS2_PLACEMENT_3D ( 'NONE', #38423, #16794, #32674 ) ;
#12267 = PLANE ( 'NONE',  #17441 ) ;
#12268 = CARTESIAN_POINT ( 'NONE',  ( 86.36811837411410409, 0.9377611381114191458, -5.884791073222536362 ) ) ;
#12270 = CARTESIAN_POINT ( 'NONE',  ( 21.71197053136906163, 6.328941705067348877, 3.193005318136709736 ) ) ;
#12269 = CARTESIAN_POINT ( 'NONE',  ( 33.14263624204154723, -3.231821542972313388, 5.586707398679605419 ) ) ;
#12271 = VERTEX_POINT ( 'NONE', #17348 ) ;
#12272 = CARTESIAN_POINT ( 'NONE',  ( 24.50294889293943257, 2.766753032866218653, 3.859934611448354591 ) ) ;
#12273 = DIRECTION ( 'NONE',  ( 0.000000000000000000, -0.000000000000000000, -1.000000000000000000 ) ) ;
#12274 = ORIENTED_EDGE ( 'NONE', *, *, #34161, .F. ) ;
#12275 = CARTESIAN_POINT ( 'NONE',  ( -33.07867591359219972, -24.55319635012989110, 6.700000000000000178 ) ) ;
#12276 = UNCERTAINTY_MEASURE_WITH_UNIT (LENGTH_MEASURE( 1.000000000000000082E-05 ), #15675, 'distance_accuracy_value', 'NONE');
#12277 = ADVANCED_FACE ( 'NONE', ( #7902 ), #23558, .F. ) ;
#12278 = ORIENTED_EDGE ( 'NONE', *, *, #34628, .F. ) ;
#12279 = CARTESIAN_POINT ( 'NONE',  ( 78.65528874306559715, 65.84149099381058079, -2.048264032867935569 ) ) ;
#12280 = CARTESIAN_POINT ( 'NONE',  ( -1.746138059369836570, -28.96840265811469806, 7.762796336881261361 ) ) ;
#12281 = CARTESIAN_POINT ( 'NONE',  ( 80.74625401487976717, 62.12052764141679262, 3.052025427726071438 ) ) ;
#12283 = ORIENTED_EDGE ( 'NONE', *, *, #10172, .T. ) ;
#12282 = DIRECTION ( 'NONE',  ( 1.000000000000000000, 0.000000000000000000, 0.000000000000000000 ) ) ;
#12284 = DIRECTION ( 'NONE',  ( 0.000000000000000000, 0.000000000000000000, 1.000000000000000000 ) ) ;
#12285 = VECTOR ( 'NONE', #30601, 1000.000000000000000 ) ;
#12286 = CARTESIAN_POINT ( 'NONE',  ( -80.19065981525227471, 31.27226540113725051, 8.800414904976364028 ) ) ;
#12288 = DIRECTION ( 'NONE',  ( -0.000000000000000000, -0.000000000000000000, 1.000000000000000000 ) ) ;
#12287 = CARTESIAN_POINT ( 'NONE',  ( 4.940354242878053803, -30.89383239149909599, 6.870724624169665340 ) ) ;
#12289 = FACE_OUTER_BOUND ( 'NONE', #38351, .T. ) ;
#12290 = CIRCLE ( 'NONE', #10326, 34.02204673211314656 ) ;
#12291 = CARTESIAN_POINT ( 'NONE',  ( 33.89725028478159174, -5.465908938576614418, 0.4877600842561391481 ) ) ;
#12292 = AXIS2_PLACEMENT_3D ( 'NONE', #34002, #8643, #6342 ) ;
#12293 = CARTESIAN_POINT ( 'NONE',  ( 24.64255241942672114, 2.987807242327306767, -3.517570117124183771 ) ) ;
#12294 = ORIENTED_EDGE ( 'NONE', *, *, #23161, .F. ) ;
#12295 = FACE_OUTER_BOUND ( 'NONE', #20875, .T. ) ;
#12296 = AXIS2_PLACEMENT_3D ( 'NONE', #790, #34786, #10236 ) ;
#12297 = CARTESIAN_POINT ( 'NONE',  ( 25.36335546794393281, -3.584835346285432767, 4.690180580146940059 ) ) ;
#12298 = CARTESIAN_POINT ( 'NONE',  ( -80.88559923893718917, -5.699916044423376960, -1.011431130875308337 ) ) ;
#12299 = FACE_OUTER_BOUND ( 'NONE', #8021, .T. ) ;
#12300 = CARTESIAN_POINT ( 'NONE',  ( 81.26611686294327797, 61.37229692769314227, 1.428845309148520037 ) ) ;
#12301 = CARTESIAN_POINT ( 'NONE',  ( 86.54108089765607303, -0.3148381559440514010, -5.858094985366312457 ) ) ;
#12302 = DIRECTION ( 'NONE',  ( 1.000000000000000000, 0.000000000000000000, 0.000000000000000000 ) ) ;
#12303 = ORIENTED_EDGE ( 'NONE', *, *, #12933, .T. ) ;
#12304 = CARTESIAN_POINT ( 'NONE',  ( -64.52609798206562175, 34.68664092740665694, -5.853076040061139906 ) ) ;
#12305 = CARTESIAN_POINT ( 'NONE',  ( 5.628486912222185445, -26.20317660986373909, 7.695279973900954751 ) ) ;
#12306 = EDGE_CURVE ( 'NONE', #15467, #15868, #4037, .T. ) ;
#12307 = FACE_BOUND ( 'NONE', #9229, .T. ) ;
#12308 = CARTESIAN_POINT ( 'NONE',  ( 14.98150154961487068, -6.080694961501129647, -2.528993159681567793 ) ) ;
#12309 = CARTESIAN_POINT ( 'NONE',  ( -66.90228649916429049, 37.07846761000594427, -9.592188357273899513 ) ) ;
#12310 = DIRECTION ( 'NONE',  ( 1.000000000000000000, 0.000000000000000000, -0.000000000000000000 ) ) ;
#12311 = CARTESIAN_POINT ( 'NONE',  ( 1.774094287987110441, -26.17071518185239754, 6.874555630061442990 ) ) ;
#12312 = ORIENTED_EDGE ( 'NONE', *, *, #27516, .T. ) ;
#12313 = CARTESIAN_POINT ( 'NONE',  ( 36.63332213572625307, -3.079482314827179934, 5.923913918160702785 ) ) ;
#12314 = EDGE_CURVE ( 'NONE', #27368, #7875, #4627, .T. ) ;
#12315 = CARTESIAN_POINT ( 'NONE',  ( 87.00024757794628272, 0.6349172363070331171, 4.931108601852515427 ) ) ;
#12316 = ORIENTED_EDGE ( 'NONE', *, *, #8302, .T. ) ;
#12318 = LINE ( 'NONE', #37430, #40162 ) ;
#12317 = CARTESIAN_POINT ( 'NONE',  ( 80.98576866654174466, 63.46339031992854984, -3.471690071579498493 ) ) ;
#12319 = CARTESIAN_POINT ( 'NONE',  ( 22.17363360563139452, -2.652663328054713165, 3.667129814150781097 ) ) ;
#12320 = CARTESIAN_POINT ( 'NONE',  ( -69.79768788248055955, -46.12641766718275704, 9.936119964364207746 ) ) ;
#12321 = AXIS2_PLACEMENT_3D ( 'NONE', #32425, #19456, #32029 ) ;
#12322 = CARTESIAN_POINT ( 'NONE',  ( 4.273337484900067373, -31.79252814967387053, 6.894806418505345036 ) ) ;
#12323 = VECTOR ( 'NONE', #8667, 1000.000000000000000 ) ;
#12324 = ORIENTED_EDGE ( 'NONE', *, *, #24891, .T. ) ;
#12325 = CARTESIAN_POINT ( 'NONE',  ( 27.29202159548859896, -4.463074182346106866, -3.652272488581413512 ) ) ;
#12326 = ORIENTED_EDGE ( 'NONE', *, *, #14859, .F. ) ;
#12327 = MANIFOLD_SOLID_BREP ( 'Boss-Extrude8', #12401 ) ;
#12328 = ORIENTED_EDGE ( 'NONE', *, *, #32300, .F. ) ;
#12329 = EDGE_CURVE ( 'NONE', #2870, #37024, #33029, .T. ) ;
#12330 = CARTESIAN_POINT ( 'NONE',  ( 81.17223480711247419, 61.34085670634290466, -1.541060042019461340 ) ) ;
#12331 = DIRECTION ( 'NONE',  ( -0.000000000000000000, -0.000000000000000000, 1.000000000000000000 ) ) ;
#12332 = VERTEX_POINT ( 'NONE', #4819 ) ;
#12334 = CARTESIAN_POINT ( 'NONE',  ( 33.57045594063073679, -0.3384725396225634619, 5.045718172883097097 ) ) ;
#12333 = CARTESIAN_POINT ( 'NONE',  ( 22.89135895909411644, 2.899355188632806613, 4.326634353261504806 ) ) ;
#12335 = VERTEX_POINT ( 'NONE', #29926 ) ;
#12336 = CARTESIAN_POINT ( 'NONE',  ( 80.91683595914862792, 65.70075836866568864, -2.460680857249041509 ) ) ;
#12337 = CARTESIAN_POINT ( 'NONE',  ( 4.681048734869769135, -27.93415238764535857, 6.874555630061442990 ) ) ;
#12338 = AXIS2_PLACEMENT_3D ( 'NONE', #24191, #5257, #33065 ) ;
#12340 = CARTESIAN_POINT ( 'NONE',  ( 86.03410341386039306, 1.720136217376576848, -4.402104626801674137 ) ) ;
#12339 = CARTESIAN_POINT ( 'NONE',  ( 4.883069014757387194, -28.37387203058899487, 7.680992449362118002 ) ) ;
#12341 = DIRECTION ( 'NONE',  ( -0.000000000000000000, -0.000000000000000000, -1.000000000000000000 ) ) ;
#12342 = CARTESIAN_POINT ( 'NONE',  ( 0.5135240150758065836, -26.28321512987682596, 7.773839561854632763 ) ) ;
#12343 = CARTESIAN_POINT ( 'NONE',  ( 74.19779514372055473, 59.81543539827580958, 3.749455561448977736 ) ) ;
#12344 = ORIENTED_EDGE ( 'NONE', *, *, #6847, .T. ) ;
#12345 = CARTESIAN_POINT ( 'NONE',  ( 23.05884816843563456, 3.162798540487469001, -4.037182842946084982 ) ) ;
#12346 = ORIENTED_EDGE ( 'NONE', *, *, #12696, .T. ) ;
#12347 = ADVANCED_FACE ( 'NONE', ( #10175 ), #22765, .F. ) ;
#12348 = AXIS2_PLACEMENT_3D ( 'NONE', #35166, #373, #21990 ) ;
#12349 = CARTESIAN_POINT ( 'NONE',  ( 21.85643539959774984, 9.043776176932434296, -7.298091200098202336 ) ) ;
#12350 = CARTESIAN_POINT ( 'NONE',  ( 3.435265683109236967, -26.53015935524666347, 7.750000000000001776 ) ) ;
#12351 = VERTEX_POINT ( 'NONE', #22961 ) ;
#12352 = DIRECTION ( 'NONE',  ( -0.000000000000000000, -0.000000000000000000, 1.000000000000000000 ) ) ;
#12353 = CARTESIAN_POINT ( 'NONE',  ( 80.02729359676493459, 65.84138187185888569, 2.563845612517933858 ) ) ;
#12354 = CARTESIAN_POINT ( 'NONE',  ( 85.61973765214487742, 2.185571507920985646, -3.964146163151171187 ) ) ;
#12355 = ORIENTED_EDGE ( 'NONE', *, *, #35636, .F. ) ;
#12356 = AXIS2_PLACEMENT_3D ( 'NONE', #39536, #11322, #4576 ) ;
#12357 = CARTESIAN_POINT ( 'NONE',  ( -66.99872204295122913, 28.48507918597134037, 6.999999999999999112 ) ) ;
#12358 = ORIENTED_EDGE ( 'NONE', *, *, #36340, .F. ) ;
#12359 = CARTESIAN_POINT ( 'NONE',  ( 19.71439828684868445, -2.982188169833531521, 3.242426474250064583 ) ) ;
#12360 = CARTESIAN_POINT ( 'NONE',  ( -1.681553744649562532, -29.97427170972491695, 7.405500484323178867 ) ) ;
#12361 = CARTESIAN_POINT ( 'NONE',  ( 20.48006656716360041, 3.803899341377876109, -3.402807718724278452 ) ) ;
#12362 = CARTESIAN_POINT ( 'NONE',  ( -1.715618416584987704, -30.36287436211992130, 7.139344958878412584 ) ) ;
#12363 = CARTESIAN_POINT ( 'NONE',  ( -1.348492144037532814, -27.85111747872926813, 7.698786668945014178 ) ) ;
#12364 = B_SPLINE_CURVE_WITH_KNOTS ( 'NONE', 3,
 ( #15244, #12974, #40351, #37270, #31319, #5992, #18530, #37875, #9682, #31114, #2929, #15448, #37469, #19569, #38887, #13180, #22462, #31932, #32342 ),
 .UNSPECIFIED., .F., .F.,
 ( 4, 3, 3, 3, 3, 3, 4 ),
 ( 8.673617379884035472E-19, 2.546128104245028707E-05, 5.711050680484775665E-05, 8.113074941676622380E-05, 0.0001053129305727147218, 0.0001360598016347234519, 0.0001612931755702011341 ),
 .UNSPECIFIED. ) ;
#12365 = EDGE_CURVE ( 'NONE', #9599, #2897, #10461, .T. ) ;
#12366 = EDGE_CURVE ( 'NONE', #30637, #10351, #25217, .T. ) ;
#12367 = ORIENTED_EDGE ( 'NONE', *, *, #32984, .F. ) ;
#12368 = DIRECTION ( 'NONE',  ( 0.8459487642040833810, 0.000000000000000000, 0.5332641825039293737 ) ) ;
#12369 = EDGE_CURVE ( 'NONE', #28633, #31670, #2364, .T. ) ;
#12370 = PLANE ( 'NONE',  #7272 ) ;
#12371 = ORIENTED_EDGE ( 'NONE', *, *, #23183, .F. ) ;
#12372 = ORIENTED_EDGE ( 'NONE', *, *, #33305, .T. ) ;
#12373 = CARTESIAN_POINT ( 'NONE',  ( 33.94504222670371973, -0.4898145577208962709, 5.123711933742746361 ) ) ;
#12374 =( BOUNDED_CURVE ( )  B_SPLINE_CURVE ( 3, ( #33607, #17921, #30505, #3540 ),
 .UNSPECIFIED., .F., .T. ) 
 B_SPLINE_CURVE_WITH_KNOTS ( ( 4, 4 ),
 ( 1.347909859412853351, 1.534781240595298302 ),
 .UNSPECIFIED. ) 
 CURVE ( )  GEOMETRIC_REPRESENTATION_ITEM ( )  RATIONAL_B_SPLINE_CURVE ( ( 1.000000000000000000, 0.9970920404276226723, 0.9970920404276226723, 1.000000000000000000 ) ) 
 REPRESENTATION_ITEM ( '' )  );
#12375 = DIRECTION ( 'NONE',  ( -1.000000000000000000, 0.000000000000000000, 0.000000000000000000 ) ) ;
#12376 = ORIENTED_EDGE ( 'NONE', *, *, #29299, .F. ) ;
#12377 = CARTESIAN_POINT ( 'NONE',  ( 66.58157743075884127, 57.80130068828511014, -3.999688274311175906 ) ) ;
#12378 = ORIENTED_EDGE ( 'NONE', *, *, #25406, .F. ) ;
#12379 = CARTESIAN_POINT ( 'NONE',  ( 88.35188732102578513, -0.8833086758121115878, 0.5115122137427119409 ) ) ;
#12380 = CARTESIAN_POINT ( 'NONE',  ( -73.10036559450711025, 7.400480790150822941, -9.764070703836081222 ) ) ;
#12381 = LINE ( 'NONE', #24323, #38446 ) ;
#12382 = ORIENTED_EDGE ( 'NONE', *, *, #25074, .T. ) ;
#12383 = DIRECTION ( 'NONE',  ( -0.000000000000000000, -0.000000000000000000, 1.000000000000000000 ) ) ;
#12384 = PLANE ( 'NONE',  #27146 ) ;
#12385 = EDGE_LOOP ( 'NONE', ( #23391, #7072, #31799, #9327, #24593 ) ) ;
#12386 = CARTESIAN_POINT ( 'NONE',  ( 23.73355850457707206, 3.546588217239842411, 3.226370594130565816 ) ) ;
#12387 = CARTESIAN_POINT ( 'NONE',  ( 81.46190421581948726, 61.46294189193148583, -1.114595100209338163 ) ) ;
#12388 = VECTOR ( 'NONE', #8292, 1000.000000000000000 ) ;
#12389 = CARTESIAN_POINT ( 'NONE',  ( 81.17225696364401699, 61.44517649410260418, 1.881209715725439269 ) ) ;
#12390 = DIRECTION ( 'NONE',  ( 0.000000000000000000, 0.000000000000000000, 1.000000000000000000 ) ) ;
#12391 = ORIENTED_EDGE ( 'NONE', *, *, #7991, .F. ) ;
#12392 = CARTESIAN_POINT ( 'NONE',  ( 76.69853897424475520, 64.65515986876398813, -2.498359881428370066 ) ) ;
#12393 = APPLICATION_CONTEXT ( 'automotive_design' ) ;
#12395 = CARTESIAN_POINT ( 'NONE',  ( -22.97867591359219119, -24.55319635012989110, 6.800000000000000711 ) ) ;
#12394 = CARTESIAN_POINT ( 'NONE',  ( 2.344207582906673970, -26.12964968137214683, 6.888594555015730592 ) ) ;
#12396 = CARTESIAN_POINT ( 'NONE',  ( 18.58232099604030552, 8.030589776515261846, -3.022115281584475621 ) ) ;
#12397 = CARTESIAN_POINT ( 'NONE',  ( 81.39943925848315587, 61.85181198611487474, -2.332991218130514355 ) ) ;
#12398 = CARTESIAN_POINT ( 'NONE',  ( 77.20018789615933485, 65.00686241173514190, 2.285396881590278984 ) ) ;
#12399 = VERTEX_POINT ( 'NONE', #18381 ) ;
#12400 = CARTESIAN_POINT ( 'NONE',  ( 2.088670072939348366, -32.95477192119402332, 7.386948897581450346 ) ) ;
#12401 = CLOSED_SHELL ( 'NONE', ( #39691, #1987, #25949, #21027, #39842, #35251, #13945, #36039, #9900, #12166, #13085, #28260, #37481, #27739, #13394, #11551, #29530, #1331, #38039, #26954, #37778, #38983, #571, #20533, #3212, #9618, #37540 ) ) ;
#12402 = CARTESIAN_POINT ( 'NONE',  ( -57.16504416091206053, 33.41445838748276742, 4.000000000000000000 ) ) ;
#12403 = CARTESIAN_POINT ( 'NONE',  ( 82.21758965863736535, 62.47540435105901935, 1.725837398062986638 ) ) ;
#12405 = CARTESIAN_POINT ( 'NONE',  ( 14.69558838330753581, -65.19654454972992141, 2.500000000000000444 ) ) ;
#12404 = CARTESIAN_POINT ( 'NONE',  ( 4.258720360809321370, -31.95843491878680354, 6.989977667959444751 ) ) ;
#12406 = CARTESIAN_POINT ( 'NONE',  ( 30.73735125564872916, -2.095387222228427770, 5.934458408524426076 ) ) ;
#12407 = CARTESIAN_POINT ( 'NONE',  ( -1.357913867432435362, -31.27192221750447487, 6.875671892026062437 ) ) ;
#12408 = CARTESIAN_POINT ( 'NONE',  ( 1.508613083882804684, -33.06467219138443880, 6.941203072598477242 ) ) ;
#12409 = CARTESIAN_POINT ( 'NONE',  ( 24.72159449605993231, 0.6340518189776346292, -4.784391175910871929 ) ) ;
#12410 = ADVANCED_FACE ( 'NONE', ( #40206 ), #12789, .T. ) ;
#12411 = DIRECTION ( 'NONE',  ( 1.000000000000000000, 0.000000000000000000, 0.000000000000000000 ) ) ;
#12412 = CARTESIAN_POINT ( 'NONE',  ( -7.890026461918810519, -29.56993018339340651, 6.000000000000000000 ) ) ;
#12413 = DIRECTION ( 'NONE',  ( 1.000000000000000000, 0.000000000000000000, 0.000000000000000000 ) ) ;
#12414 = EDGE_CURVE ( 'NONE', #40359, #5482, #26844, .T. ) ;
#12415 = CARTESIAN_POINT ( 'NONE',  ( 33.91388920362712867, -0.5462387119675344849, -5.194274413794256695 ) ) ;
#12416 = LINE ( 'NONE', #34472, #36476 ) ;
#12417 = CARTESIAN_POINT ( 'NONE',  ( 32.21384408659537968, -3.775819508426534465, 4.843400441209068319 ) ) ;
#12418 = CARTESIAN_POINT ( 'NONE',  ( -0.9609532066394848027, -31.68588194093026189, 7.778050822775630202 ) ) ;
#12419 = CARTESIAN_POINT ( 'NONE',  ( -14.87867591359218977, -26.64985754041175525, 6.700000000000000178 ) ) ;
#12420 = CARTESIAN_POINT ( 'NONE',  ( 8.290806648384990041, -33.63722727088462250, 2.499999999999998668 ) ) ;
#12421 = CARTESIAN_POINT ( 'NONE',  ( 2.119804661062819839, -32.94396210681857440, 6.882085323592686876 ) ) ;
#12422 = EDGE_CURVE ( 'NONE', #3833, #26349, #26609, .T. ) ;
#12423 = CARTESIAN_POINT ( 'NONE',  ( -62.81463675898083210, 36.67811266762162603, -4.600311178732272133 ) ) ;
#12424 = AXIS2_PLACEMENT_3D ( 'NONE', #21032, #17920, #2107 ) ;
#12425 = CARTESIAN_POINT ( 'NONE',  ( -24.44874870218064089, -26.64985754041175525, 6.700000000000000178 ) ) ;
#12426 = CARTESIAN_POINT ( 'NONE',  ( -80.92837670882107659, 2.429809908903242555, -12.50000000000000000 ) ) ;
#12427 = ORIENTED_EDGE ( 'NONE', *, *, #31745, .T. ) ;
#12428 = ORIENTED_EDGE ( 'NONE', *, *, #32159, .F. ) ;
#12429 = CARTESIAN_POINT ( 'NONE',  ( 35.94200923520244828, 151.3264224549853907, 4.000000000000000000 ) ) ;
#12430 = CARTESIAN_POINT ( 'NONE',  ( 69.41850365747683327, 58.24027689931818230, -3.921432738910689331 ) ) ;
#12431 = ORIENTED_EDGE ( 'NONE', *, *, #35860, .T. ) ;
#12432 = CARTESIAN_POINT ( 'NONE',  ( -0.9068966613934061893, -27.23885067285716843, 7.766640943994647550 ) ) ;
#12433 = EDGE_CURVE ( 'NONE', #14367, #21155, #36000, .T. ) ;
#12434 = CARTESIAN_POINT ( 'NONE',  ( 1.212983646527633130, -26.10426722441512837, 7.754798119455333705 ) ) ;
#12435 = DIRECTION ( 'NONE',  ( -0.000000000000000000, 0.000000000000000000, 1.000000000000000000 ) ) ;
#12436 = CARTESIAN_POINT ( 'NONE',  ( 5.054793046568992310, -30.12489038615697012, 7.695279973900954751 ) ) ;
#12437 = ORIENTED_EDGE ( 'NONE', *, *, #17829, .T. ) ;
#12438 = CARTESIAN_POINT ( 'NONE',  ( 24.41077649390761550, 3.166270396914395935, 3.259050073679078618 ) ) ;
#12439 = DIRECTION ( 'NONE',  ( 1.000000000000000000, 0.000000000000000000, 0.000000000000000000 ) ) ;
#12440 = ORIENTED_EDGE ( 'NONE', *, *, #22710, .T. ) ;
#12441 = ORIENTED_EDGE ( 'NONE', *, *, #2886, .T. ) ;
#12442 = CARTESIAN_POINT ( 'NONE',  ( 80.49182418769539993, 61.81278841749718822, -2.961936469198068078 ) ) ;
#12444 = CARTESIAN_POINT ( 'NONE',  ( -34.24874870218063450, -25.49307895267003587, 6.700000000000000178 ) ) ;
#12443 = CARTESIAN_POINT ( 'NONE',  ( 22.07198986276520714, 0.3265494727465731439, 7.434200068064451550 ) ) ;
#12445 = CARTESIAN_POINT ( 'NONE',  ( 78.68779346184201984, 66.05675297672225099, -1.054034669008010905 ) ) ;
#12446 = CARTESIAN_POINT ( 'NONE',  ( 79.93872656714209768, 63.00306196921508217, 3.690346394509887773 ) ) ;
#12447 = AXIS2_PLACEMENT_3D ( 'NONE', #33798, #24304, #2926 ) ;
#12448 = CARTESIAN_POINT ( 'NONE',  ( 4.336009428051142756, -27.42202173051807890, 6.894806418505345924 ) ) ;
#12449 = CARTESIAN_POINT ( 'NONE',  ( 82.26973386304365476, 64.90130211351629441, 1.000000000000000000 ) ) ;
#12450 = CARTESIAN_POINT ( 'NONE',  ( -1.000637662739485290, -31.79578935716557453, 6.894806418505347700 ) ) ;
#12451 = CARTESIAN_POINT ( 'NONE',  ( 21.85643539959775694, 1.480681348264278219, 12.33944218828100325 ) ) ;
#12452 = CARTESIAN_POINT ( 'NONE',  ( -1.599034431228576247, -30.73774772367137942, 6.894806418505347700 ) ) ;
#12453 = ORIENTED_EDGE ( 'NONE', *, *, #38331, .F. ) ;
#12454 = CARTESIAN_POINT ( 'NONE',  ( -72.84051408678523387, 2.240445720093386051, 10.96224446246069206 ) ) ;
#12455 = CARTESIAN_POINT ( 'NONE',  ( 36.72314012181375631, -3.448745041943457323, 5.863009582911698381 ) ) ;
#12456 = ORIENTED_EDGE ( 'NONE', *, *, #33575, .T. ) ;
#12457 = DIRECTION ( 'NONE',  ( 0.000000000000000000, 0.000000000000000000, 1.000000000000000000 ) ) ;
#12458 = CARTESIAN_POINT ( 'NONE',  ( -80.90861860399087391, 11.45717611192839591, 0.6283086135788882309 ) ) ;
#12459 = AXIS2_PLACEMENT_3D ( 'NONE', #1988, #10808, #36548 ) ;
#12460 = CARTESIAN_POINT ( 'NONE',  ( 4.200390093233091093, -29.56993018339339940, -6.000000000000000000 ) ) ;
#12461 = CARTESIAN_POINT ( 'NONE',  ( 36.44575679768344401, -1.731622218426172921, -5.730272923922282935 ) ) ;
#12462 = CARTESIAN_POINT ( 'NONE',  ( -0.8786759135921904385, -24.55319635012989110, 6.700000000000000178 ) ) ;
#12463 = CARTESIAN_POINT ( 'NONE',  ( 22.07127107929524357, 4.795919128869573278, 3.651153666268970532 ) ) ;
#12464 = DIRECTION ( 'NONE',  ( 1.000000000000000000, 0.000000000000000000, 0.000000000000000000 ) ) ;
#12465 = PLANE ( 'NONE',  #33289 ) ;
#12466 = CARTESIAN_POINT ( 'NONE',  ( 3.480798653453814673, -32.58325819489262187, 7.710604733652628440 ) ) ;
#12467 = EDGE_CURVE ( 'NONE', #24834, #5389, #27243, .T. ) ;
#12468 = EDGE_CURVE ( 'NONE', #13597, #33127, #24155, .T. ) ;
#12469 = CARTESIAN_POINT ( 'NONE',  ( 3.896194328649233984, -32.16578144256224903, 7.635761828346577573 ) ) ;
#12470 = CARTESIAN_POINT ( 'NONE',  ( 23.61265236088880215, 0.4553577143438285457, -5.501100469002734528 ) ) ;
#12471 = CARTESIAN_POINT ( 'NONE',  ( 31.69270225732497082, -3.760796806013388505, -4.741932875280792103 ) ) ;
#12472 = EDGE_CURVE ( 'NONE', #10309, #13597, #324, .T. ) ;
#12473 = CARTESIAN_POINT ( 'NONE',  ( 24.36839190658592358, 2.936743033212012577, -3.728160028041425988 ) ) ;
#12474 = ORIENTED_EDGE ( 'NONE', *, *, #32427, .T. ) ;
#12475 = CARTESIAN_POINT ( 'NONE',  ( 67.04239844378345481, 57.90286417203066094, 3.997553359131193584 ) ) ;
#12476 = CARTESIAN_POINT ( 'NONE',  ( 33.67582729204764291, -3.265305600472629077, 5.462325320484106683 ) ) ;
#12477 = DIRECTION ( 'NONE',  ( 0.9848077530122075762, 0.1736481776669329402, 0.000000000000000000 ) ) ;
#12478 = VECTOR ( 'NONE', #26746, 1000.000000000000000 ) ;
#12479 = DIRECTION ( 'NONE',  ( -0.6834397476448844655, 0.000000000000000000, -0.7300069255418721870 ) ) ;
#12480 = CARTESIAN_POINT ( 'NONE',  ( 88.08925887309592895, -2.022426073114577338, 2.982665067064442788 ) ) ;
#12482 = CARTESIAN_POINT ( 'NONE',  ( 35.96707384839896093, -3.154842221623805454, -5.819929759647552991 ) ) ;
#12481 = FACE_OUTER_BOUND ( 'NONE', #28647, .T. ) ;
#12483 = PRODUCT_DEFINITION_SHAPE ( 'NONE', 'NONE',  #40726 ) ;
#12484 = VERTEX_POINT ( 'NONE', #2569 ) ;
#12485 = CARTESIAN_POINT ( 'NONE',  ( 25.64725611152496398, 2.152986409533134804, 4.135202000189527993 ) ) ;
#12486 = B_SPLINE_CURVE_WITH_KNOTS ( 'NONE', 3,
 ( #16137, #10145, #28699, #22736, #6875, #19430, #35299, #32004, #7071, #19636, #32210, #906, #13444, #26019, #30113, #5194, #1510, #24327, #2123, #23530, #20421, #5396, #39153, #36284, #11750, #10948, #27212, #39561, #26618, #14244, #33621 ),
 .UNSPECIFIED., .F., .F.,
 ( 4, 3, 3, 3, 3, 3, 3, 3, 3, 3, 4 ),
 ( 0.000000000000000000, 3.077658087705726812E-05, 6.152638666999176798E-05, 9.267501192706665062E-05, 0.0001241882240135210144, 0.0001556618703051689684, 0.0001866161554452226018, 0.0002167966385860985265, 0.0002463805737537792784, 0.0002758761370306543332, 0.0002847094172290032059 ),
 .UNSPECIFIED. ) ;
#12487 = DIRECTION ( 'NONE',  ( 1.000000000000000000, 0.000000000000000000, 0.000000000000000000 ) ) ;
#12488 = LINE ( 'NONE', #3655, #27876 ) ;
#12489 = ORIENTED_EDGE ( 'NONE', *, *, #19307, .T. ) ;
#12490 = VECTOR ( 'NONE', #13254, 1000.000000000000000 ) ;
#12491 = ORIENTED_EDGE ( 'NONE', *, *, #25453, .F. ) ;
#12492 = CARTESIAN_POINT ( 'NONE',  ( 79.52504771873071832, 64.52527500529767224, -3.543129918319044780 ) ) ;
#12493 = CARTESIAN_POINT ( 'NONE',  ( 4.207321055524802844, -27.11779497589776255, 7.501983001166816045 ) ) ;
#12494 = CARTESIAN_POINT ( 'NONE',  ( 79.70130230958179141, 64.28379252955069489, 3.649417990092605368 ) ) ;
#12496 = VERTEX_POINT ( 'NONE', #38134 ) ;
#12495 = CARTESIAN_POINT ( 'NONE',  ( -0.8561835264942624368, -27.32849620891636633, 6.874555630061441214 ) ) ;
#12497 = CARTESIAN_POINT ( 'NONE',  ( -0.06469087068677582819, -26.54759843608177761, 7.750000000000000888 ) ) ;
#12498 = CARTESIAN_POINT ( 'NONE',  ( -64.08758708074093136, 38.60011822860993647, -4.018727294472382638 ) ) ;
#12499 = DIRECTION ( 'NONE',  ( -0.4826092789263580207, -0.5751513419797943394, -0.6605219282605403475 ) ) ;
#12500 = CYLINDRICAL_SURFACE ( 'NONE', #10988, 3.499999999999999556 ) ;
#12501 = CARTESIAN_POINT ( 'NONE',  ( 21.71676751225188795, 6.286869429030311984, -3.207926565813705277 ) ) ;
#12502 = ORIENTED_EDGE ( 'NONE', *, *, #7388, .F. ) ;
#12503 = CARTESIAN_POINT ( 'NONE',  ( -65.15514661499977933, 34.97220226750606997, -6.888442104241543795 ) ) ;
#12504 = CARTESIAN_POINT ( 'NONE',  ( -76.99182769667817183, -4.628834071841179565, -9.484053338739713013 ) ) ;
#12505 = DIRECTION ( 'NONE',  ( 0.000000000000000000, 0.000000000000000000, 1.000000000000000000 ) ) ;
#12506 = CARTESIAN_POINT ( 'NONE',  ( 81.45253739226701839, 61.71286443377144337, 1.983726836936649196 ) ) ;
#12507 = CARTESIAN_POINT ( 'NONE',  ( 85.98972789526511917, 0.6168376674493800671, -5.987237289632960646 ) ) ;
#12508 = DIRECTION ( 'NONE',  ( 0.8660254037844252739, 0.5000000000000230926, 0.000000000000000000 ) ) ;
#12509 = VERTEX_POINT ( 'NONE', #9935 ) ;
#12510 = DIRECTION ( 'NONE',  ( 0.000000000000000000, 0.6662082868431838945, 0.7457657263118692148 ) ) ;
#12511 = CARTESIAN_POINT ( 'NONE',  ( 22.07069217792962590, 4.357467706526993112, -1.544973507881162167 ) ) ;
#12512 = CARTESIAN_POINT ( 'NONE',  ( 4.021697826674504483, -26.95045787073729215, 6.863805608295730387 ) ) ;
#12513 = AXIS2_PLACEMENT_3D ( 'NONE', #21231, #23893, #26996 ) ;
#12514 = CARTESIAN_POINT ( 'NONE',  ( -1.799609906766908685, -29.77832925049299462, 7.162856560672855366 ) ) ;
#12515 = EDGE_CURVE ( 'NONE', #38606, #5089, #22516, .T. ) ;
#12516 = DIRECTION ( 'NONE',  ( -0.000000000000000000, -1.000000000000000000, -0.000000000000000000 ) ) ;
#12517 = ORIENTED_EDGE ( 'NONE', *, *, #31818, .T. ) ;
#12518 = CARTESIAN_POINT ( 'NONE',  ( 27.40535003225689792, 0.9587719845282556275, 4.483665692065598840 ) ) ;
#12519 = B_SPLINE_CURVE_WITH_KNOTS ( 'NONE', 3,
 ( #23513, #17305, #13838, #1102, #3993, #10533, #26407, #29883, #35680, #32590, #7656, #16513, #7855, #14230, #4388, #11130, #38937, #23113, #1301 ),
 .UNSPECIFIED., .F., .F.,
 ( 4, 3, 3, 3, 3, 3, 4 ),
 ( 0.000000000000000000, 2.546128104244680068E-05, 5.711050680483461070E-05, 8.113074941675478546E-05, 0.0001053129305727011422, 0.0001360598016347041802, 0.0001612931755713763551 ),
 .UNSPECIFIED. ) ;
#12520 = CARTESIAN_POINT ( 'NONE',  ( 86.92636418897033934, 0.7179065655219835085, -4.964803926638174048 ) ) ;
#12521 = ORIENTED_EDGE ( 'NONE', *, *, #2333, .T. ) ;
#12523 = CARTESIAN_POINT ( 'NONE',  ( -66.99872204295122913, 28.48507918597134037, -4.000000000000000000 ) ) ;
#12522 = CARTESIAN_POINT ( 'NONE',  ( 81.23686708412716939, 61.78859655676697571, -2.419967184825706497 ) ) ;
#12524 = CARTESIAN_POINT ( 'NONE',  ( 2.915650558103385137, -32.85217667056087265, 7.643192810543821381 ) ) ;
#12525 = CARTESIAN_POINT ( 'NONE',  ( 14.77277131670251364, 13.03059887336277356, -2.498940285545853346 ) ) ;
#12526 = ORIENTED_EDGE ( 'NONE', *, *, #23701, .F. ) ;
#12527 = VECTOR ( 'NONE', #11330, 1000.000000000000000 ) ;
#12528 = CARTESIAN_POINT ( 'NONE',  ( 27.53908758452205419, -4.370590091868444382, -3.734973139623710026 ) ) ;
#12529 = VERTEX_POINT ( 'NONE', #6658 ) ;
#12530 = CARTESIAN_POINT ( 'NONE',  ( -79.80088323097261593, 11.50896648099637432, 4.631886560738033509 ) ) ;
#12532 = EDGE_LOOP ( 'NONE', ( #20558, #31342 ) ) ;
#12531 = ORIENTED_EDGE ( 'NONE', *, *, #19547, .T. ) ;
#12533 = CARTESIAN_POINT ( 'NONE',  ( 79.12626349118841063, 65.57005066984849861, -2.769656700700048990 ) ) ;
#12534 = CARTESIAN_POINT ( 'NONE',  ( 35.93061354739079150, -3.156855339584533127, 5.814239247879517514 ) ) ;
#12535 = ORIENTED_EDGE ( 'NONE', *, *, #22799, .F. ) ;
#12536 = ADVANCED_FACE ( 'NONE', ( #28263 ), #13025, .F. ) ;
#12538 = CARTESIAN_POINT ( 'NONE',  ( 36.01495275453719813, -1.469146332022411405, 5.615055713102431234 ) ) ;
#12537 = CARTESIAN_POINT ( 'NONE',  ( 23.58159892518875012, 2.786089680335510188, 4.075354304694349672 ) ) ;
#12539 = ORIENTED_EDGE ( 'NONE', *, *, #21900, .T. ) ;
#12540 = CARTESIAN_POINT ( 'NONE',  ( 80.36115181822145814, 66.02274906846022873, -2.190303691588677104 ) ) ;
#12541 = VECTOR ( 'NONE', #28168, 1000.000000000000000 ) ;
#12542 = CARTESIAN_POINT ( 'NONE',  ( 1.869561550574128761, -26.07402100007339740, 7.013842709614101167 ) ) ;
#12544 = CARTESIAN_POINT ( 'NONE',  ( 86.51911666896515385, 1.175346309125120836, -4.933042343133747565 ) ) ;
#12543 = CARTESIAN_POINT ( 'NONE',  ( 4.883850366368126750, -28.37594736283919516, 7.670860738520327793 ) ) ;
#12545 = DIRECTION ( 'NONE',  ( 1.000000000000000000, 0.000000000000000000, 0.000000000000000000 ) ) ;
#12546 = CARTESIAN_POINT ( 'NONE',  ( -64.08758708074093136, 42.32104734179812766, -3.571363574845913380 ) ) ;
#12547 = CARTESIAN_POINT ( 'NONE',  ( 73.23371602657820745, 61.99063567959824894, 3.556895493546552878 ) ) ;
#12548 = ORIENTED_EDGE ( 'NONE', *, *, #38740, .F. ) ;
#12549 = CARTESIAN_POINT ( 'NONE',  ( 22.22094290343520839, 3.703924387003111995, -4.206398560386165109 ) ) ;
#12550 = ORIENTED_EDGE ( 'NONE', *, *, #16773, .T. ) ;
#12551 = CARTESIAN_POINT ( 'NONE',  ( 21.85643539959779602, 6.788858854521340191, -12.70575755685024610 ) ) ;
#12552 = CARTESIAN_POINT ( 'NONE',  ( -59.00110696496998486, 28.68040728033255249, -6.866973098862638736 ) ) ;
#12553 = VERTEX_POINT ( 'NONE', #25184 ) ;
#12554 = CARTESIAN_POINT ( 'NONE',  ( 1.070857224836541999, -26.12700842969462656, 7.743886751744251562 ) ) ;
#12555 = CARTESIAN_POINT ( 'NONE',  ( 81.56442676284315496, 64.14391357696001705, 3.071899782094677178 ) ) ;
#12556 = CARTESIAN_POINT ( 'NONE',  ( 87.18644375116411993, 0.4257728571452945587, -5.011944538332810062 ) ) ;
#12557 = ORIENTED_EDGE ( 'NONE', *, *, #23536, .F. ) ;
#12558 = VECTOR ( 'NONE', #5693, 1000.000000000000114 ) ;
#12559 = CARTESIAN_POINT ( 'NONE',  ( 14.77222812468949620, 12.33286846116140190, 2.511961485181804843 ) ) ;
#12560 = CARTESIAN_POINT ( 'NONE',  ( 14.82260051658036559, -5.954777973940915459, 2.519088763667999498 ) ) ;
#12561 = EDGE_CURVE ( 'NONE', #7366, #35091, #32088, .T. ) ;
#12562 = CARTESIAN_POINT ( 'NONE',  ( 35.33511103386211971, -3.172769356962385601, -5.721296678360661581 ) ) ;
#12563 = CARTESIAN_POINT ( 'NONE',  ( 3.222937981259239582, -32.61784141262317860, 7.386948897581449458 ) ) ;
#12564 = FACE_OUTER_BOUND ( 'NONE', #24546, .T. ) ;
#12565 = PRODUCT_DEFINITION_SHAPE ( 'NONE', 'NONE',  #27315 ) ;
#12566 = CIRCLE ( 'NONE', #29006, 3.499999999999999556 ) ;
#12567 = DIRECTION ( 'NONE',  ( -0.000000000000000000, -0.000000000000000000, 1.000000000000000000 ) ) ;
#12568 = CARTESIAN_POINT ( 'NONE',  ( -1.227874773494582961, -31.29772208934977229, 7.721096864323905073 ) ) ;
#12569 = CIRCLE ( 'NONE', #4078, 3.499999999999999556 ) ;
#12570 = VERTEX_POINT ( 'NONE', #22315 ) ;
#12571 = ORIENTED_EDGE ( 'NONE', *, *, #19360, .F. ) ;
#12572 = CARTESIAN_POINT ( 'NONE',  ( 36.44417780280348040, -1.734285983370489781, 5.731955937638065990 ) ) ;
#12573 = CARTESIAN_POINT ( 'NONE',  ( -20.34874870218063947, -25.49307895267003587, 6.800000000000000711 ) ) ;
#12574 = CARTESIAN_POINT ( 'NONE',  ( 66.69694663263604184, 57.94160696200565042, -3.999246569073970026 ) ) ;
#12575 = CARTESIAN_POINT ( 'NONE',  ( 87.73256103596717992, -2.278636154477776454, -2.442743118526013557 ) ) ;
#12576 = ADVANCED_FACE ( 'NONE', ( #34683 ), #6458, .F. ) ;
#12577 = EDGE_LOOP ( 'NONE', ( #35836, #25705, #32115, #7112, #28957 ) ) ;
#12578 = CARTESIAN_POINT ( 'NONE',  ( -58.07367359896441172, 31.71941035118960883, 4.399945119674323557 ) ) ;
#12579 = DIRECTION ( 'NONE',  ( 0.9848077530122083534, -0.1736481776669292765, 0.000000000000000000 ) ) ;
#12580 = CARTESIAN_POINT ( 'NONE',  ( 4.960873579530714395, -28.60595147853699416, 6.939395833800442226 ) ) ;
#12581 = EDGE_LOOP ( 'NONE', ( #18524, #8807 ) ) ;
#12582 = FACE_BOUND ( 'NONE', #15518, .T. ) ;
#12583 = CARTESIAN_POINT ( 'NONE',  ( -58.92473026143653669, 13.37661300689600274, 2.500000000000000000 ) ) ;
#12584 = ORIENTED_EDGE ( 'NONE', *, *, #22230, .T. ) ;
#12585 = CARTESIAN_POINT ( 'NONE',  ( 22.62710517823844114, 4.569975501755447311, 3.100331212370438294 ) ) ;
#12586 = CARTESIAN_POINT ( 'NONE',  ( 80.01568814228012627, 66.35127795588805100, -1.246975333547555742 ) ) ;
#12587 = CARTESIAN_POINT ( 'NONE',  ( 80.30796587587546753, 63.87804906342756084, 3.654032574946330936 ) ) ;
#12588 = CARTESIAN_POINT ( 'NONE',  ( 2.975028622394660260, -26.41789893177788784, 7.757178535559533294 ) ) ;
#12589 = ORIENTED_EDGE ( 'NONE', *, *, #19173, .T. ) ;
#12590 = CARTESIAN_POINT ( 'NONE',  ( 77.22142874756843867, 60.78359660874937020, -3.498861892161951648 ) ) ;
#12592 = CARTESIAN_POINT ( 'NONE',  ( 1.822194502883780931, -26.07228119081829476, 7.754798119455333705 ) ) ;
#12591 = CARTESIAN_POINT ( 'NONE',  ( -71.91909284412787429, -45.98648324524150865, 5.918062715858019018 ) ) ;
#12593 = CARTESIAN_POINT ( 'NONE',  ( 18.30399930829332789, 7.732246112693302642, -3.063179794592037375 ) ) ;
#12594 = EDGE_CURVE ( 'NONE', #30463, #15830, #40259, .T. ) ;
#12595 = EDGE_CURVE ( 'NONE', #18869, #2937, #9529, .T. ) ;
#12596 = CARTESIAN_POINT ( 'NONE',  ( 80.58645273467564607, 64.40825618792592877, -3.509897338575004078 ) ) ;
#12597 = CARTESIAN_POINT ( 'NONE',  ( 78.33250027093573920, 62.86460196216437168, 3.816136337383051025 ) ) ;
#12598 = ORIENTED_EDGE ( 'NONE', *, *, #36526, .T. ) ;
#12599 = ORIENTED_EDGE ( 'NONE', *, *, #20409, .F. ) ;
#12600 = EDGE_CURVE ( 'NONE', #17652, #21194, #12112, .T. ) ;
#12601 = LINE ( 'NONE', #15894, #30655 ) ;
#12602 = VECTOR ( 'NONE', #37253, 1000.000000000000000 ) ;
#12603 = CARTESIAN_POINT ( 'NONE',  ( -1.000637662739485290, -31.79578935716557453, 6.894806418505347700 ) ) ;
#12604 = CARTESIAN_POINT ( 'NONE',  ( 81.16926347961613430, 61.30386509772021242, 1.017094602978565909 ) ) ;
#12606 = CARTESIAN_POINT ( 'NONE',  ( -1.576479427848138437, -30.79961771809308502, 7.678495282201401650 ) ) ;
#12605 = CARTESIAN_POINT ( 'NONE',  ( 4.265822965694919588, -31.95080274967918044, 7.006908160621414083 ) ) ;
#12607 = CARTESIAN_POINT ( 'NONE',  ( 28.57954844588206811, 0.5947805351201630453, 5.396286122280502084 ) ) ;
#12608 = CARTESIAN_POINT ( 'NONE',  ( -81.45877670850643426, 35.14220020903839270, 15.50000000000000000 ) ) ;
#12609 = CARTESIAN_POINT ( 'NONE',  ( -63.05388691672963830, 35.53807678487858368, -6.298580386186273472 ) ) ;
#12610 = CARTESIAN_POINT ( 'NONE',  ( -64.72110749213834424, 34.74377494905843378, 6.240054254829134450 ) ) ;
#12611 = CARTESIAN_POINT ( 'NONE',  ( -25.07867591359219617, -26.64985754041175525, 6.700000000000000178 ) ) ;
#12612 = CARTESIAN_POINT ( 'NONE',  ( 1.672399062804430070, -26.07003816115788553, 7.733670252284492008 ) ) ;
#12613 = DIRECTION ( 'NONE',  ( 1.000000000000000000, 0.000000000000000000, 0.000000000000000000 ) ) ;
#12614 = DIRECTION ( 'NONE',  ( -0.000000000000000000, -0.000000000000000000, -1.000000000000000000 ) ) ;
#12615 = ADVANCED_FACE ( 'NONE', ( #25590 ), #15299, .F. ) ;
#12616 = CARTESIAN_POINT ( 'NONE',  ( 34.60566713630616675, -0.8402458443559904788, -5.339578216116290577 ) ) ;
#12617 = CARTESIAN_POINT ( 'NONE',  ( 6.921324086407803833, -26.64985754041175525, 6.700000000000000178 ) ) ;
#12618 = CARTESIAN_POINT ( 'NONE',  ( -0.9425575444375865475, -31.70881488915268420, 7.785172627573962778 ) ) ;
#12619 =( BOUNDED_CURVE ( )  B_SPLINE_CURVE ( 3, ( #18340, #37079, #39972, #8871 ),
 .UNSPECIFIED., .F., .T. ) 
 B_SPLINE_CURVE_WITH_KNOTS ( ( 4, 4 ),
 ( 1.347909859412855793, 1.534781240595300744 ),
 .UNSPECIFIED. ) 
 CURVE ( )  GEOMETRIC_REPRESENTATION_ITEM ( )  RATIONAL_B_SPLINE_CURVE ( ( 1.000000000000000000, 0.9970920404276226723, 0.9970920404276226723, 1.000000000000000000 ) ) 
 REPRESENTATION_ITEM ( '' )  );
#12620 = LINE ( 'NONE', #30556, #25212 ) ;
#12621 = CARTESIAN_POINT ( 'NONE',  ( 2.685785295776140114, -32.82400398323339630, 7.013842709614101167 ) ) ;
#12622 = CARTESIAN_POINT ( 'NONE',  ( 0.7510407426356037197, -34.24246986869614773, 6.954324564059724878 ) ) ;
#12623 = CARTESIAN_POINT ( 'NONE',  ( 21.88052003412104440, -13.33610013990758247, 2.500000000000000444 ) ) ;
#12624 = FACE_OUTER_BOUND ( 'NONE', #9666, .T. ) ;
#12625 = ORIENTED_EDGE ( 'NONE', *, *, #11982, .F. ) ;
#12626 = DIRECTION ( 'NONE',  ( 1.000000000000000000, 0.000000000000000000, -0.000000000000000000 ) ) ;
#12627 = CARTESIAN_POINT ( 'NONE',  ( 68.80725167329416081, 58.08536582812667604, -3.941639393089865440 ) ) ;
#12628 = ORIENTED_EDGE ( 'NONE', *, *, #6199, .F. ) ;
#12629 = CARTESIAN_POINT ( 'NONE',  ( 4.180804271322692500, -31.89534315857266122, 7.013842709614101167 ) ) ;
#12630 = EDGE_CURVE ( 'NONE', #6110, #8281, #12416, .T. ) ;
#12631 = LINE ( 'NONE', #25201, #13416 ) ;
#12632 = CARTESIAN_POINT ( 'NONE',  ( 22.42221550662346630, 3.548445137936078186, 4.163436039515404197 ) ) ;
#12633 = CARTESIAN_POINT ( 'NONE',  ( 5.045511443222842729, -28.54026521025475205, 6.903112506833890549 ) ) ;
#12634 = CARTESIAN_POINT ( 'NONE',  ( 3.505675341739891593, -26.57142622932152420, 6.870737987065012931 ) ) ;
#12635 = CIRCLE ( 'NONE', #22535, 21.28220113893567245 ) ;
#12636 = CARTESIAN_POINT ( 'NONE',  ( 5.035802448256832875, -30.22957069796434837, 7.784476445165073422 ) ) ;
#12637 = EDGE_LOOP ( 'NONE', ( #30860, #1977, #32030, #16234 ) ) ;
#12638 = CARTESIAN_POINT ( 'NONE',  ( 21.71101792114980000, 6.337217689991505587, 3.190087676312844955 ) ) ;
#12639 = CARTESIAN_POINT ( 'NONE',  ( 17.98299319363433924, -3.166408508134356925, 2.970447345965724573 ) ) ;
#12640 = VERTEX_POINT ( 'NONE', #18795 ) ;
#12641 = EDGE_CURVE ( 'NONE', #30400, #18363, #31369, .T. ) ;
#12642 = ORIENTED_EDGE ( 'NONE', *, *, #13323, .F. ) ;
#12643 = CARTESIAN_POINT ( 'NONE',  ( 78.49476978275076533, 65.27812458131612061, -2.797036776683045733 ) ) ;
#12645 = CARTESIAN_POINT ( 'NONE',  ( -1.001783842385659096, -27.34545920416798737, 7.720710062488897130 ) ) ;
#12644 = CARTESIAN_POINT ( 'NONE',  ( 21.80387297355334653, 0.2465413692211569363, 8.289364210318115767 ) ) ;
#12646 = CARTESIAN_POINT ( 'NONE',  ( 80.42837321984433174, 65.43835520823199658, -2.971291902545808217 ) ) ;
#12647 = CARTESIAN_POINT ( 'NONE',  ( 79.74939209361063774, 63.58699539661090228, 3.734652355492745990 ) ) ;
#12648 = ADVANCED_FACE ( 'NONE', ( #7852 ), #35677, .T. ) ;
#12649 = CARTESIAN_POINT ( 'NONE',  ( 89.09355779190869384, 24.84364830758654108, -8.800414904976364028 ) ) ;
#12650 = CARTESIAN_POINT ( 'NONE',  ( 2.750046964866756927, -32.80384806160494549, 7.757178535559533294 ) ) ;
#12651 = CARTESIAN_POINT ( 'NONE',  ( 21.85643539959781023, -9.626920734992143736, 7.250399157909895642 ) ) ;
#12652 = CARTESIAN_POINT ( 'NONE',  ( 0.9267304714826871681, -32.98335233567298275, 7.013842709614101167 ) ) ;
#12653 = ORIENTED_EDGE ( 'NONE', *, *, #36340, .T. ) ;
#12654 = CARTESIAN_POINT ( 'NONE',  ( -73.13416264966082281, 4.597384000621623557, 10.93019976426635154 ) ) ;
#12655 = CARTESIAN_POINT ( 'NONE',  ( -1.799561124051049621, -29.58932634693233865, 7.642460958331693810 ) ) ;
#12656 = EDGE_LOOP ( 'NONE', ( #33837, #21910, #37615, #24732 ) ) ;
#12657 = PLANE ( 'NONE',  #30715 ) ;
#12658 = FACE_OUTER_BOUND ( 'NONE', #36347, .T. ) ;
#12659 = CARTESIAN_POINT ( 'NONE',  ( 1.643782603893625849, -32.96945891428400444, 6.887041543973315250 ) ) ;
#12660 = CARTESIAN_POINT ( 'NONE',  ( 20.92045457785759410, 4.581795454354830710, -2.649697436696578645 ) ) ;
#12661 = DIRECTION ( 'NONE',  ( -0.000000000000000000, -0.000000000000000000, 1.000000000000000000 ) ) ;
#12662 = CARTESIAN_POINT ( 'NONE',  ( -1.799601224800568167, -29.57893194075474597, 7.630645770930537530 ) ) ;
#12663 = CARTESIAN_POINT ( 'NONE',  ( 17.61160109935129370, 8.414362448292965979, 2.955114308372669196 ) ) ;
#12664 = CARTESIAN_POINT ( 'NONE',  ( -0.06478834963175583717, -26.54765481601611654, 7.640616322432097540 ) ) ;
#12665 = CARTESIAN_POINT ( 'NONE',  ( 30.11812385294796002, -3.708574960581302982, 4.582163967512324021 ) ) ;
#12666 = CARTESIAN_POINT ( 'NONE',  ( -42.83131703149249603, -32.06993018339340296, 6.800000000000000711 ) ) ;
#12667 = VECTOR ( 'NONE', #40574, 1000.000000000000000 ) ;
#12668 = CARTESIAN_POINT ( 'NONE',  ( -80.92837670882107659, 2.429809908903242555, -12.50000000000000000 ) ) ;
#12669 = CARTESIAN_POINT ( 'NONE',  ( 23.59088344076351973, 0.9244265036794051538, -5.301842884707729020 ) ) ;
#12670 = CARTESIAN_POINT ( 'NONE',  ( 33.05009345505028051, -3.812300322207410996, -5.013107131247908299 ) ) ;
#12671 = CARTESIAN_POINT ( 'NONE',  ( 24.94694396431675187, 2.517674699171826624, -3.979827897743033471 ) ) ;
#12672 = VERTEX_POINT ( 'NONE', #39135 ) ;
#12673 = CARTESIAN_POINT ( 'NONE',  ( 67.04731915158012612, 57.88926793091046363, 3.996990690923977407 ) ) ;
#12674 = CARTESIAN_POINT ( 'NONE',  ( 20.48007155163331205, 3.803897258032066908, 3.402808496671325678 ) ) ;
#12675 = EDGE_CURVE ( 'NONE', #17561, #2391, #1298, .T. ) ;
#12676 = CARTESIAN_POINT ( 'NONE',  ( -70.92837670882107659, 28.72470171467712063, 0.000000000000000000 ) ) ;
#12677 = CARTESIAN_POINT ( 'NONE',  ( 85.11033487576473533, 2.122656363318763173, 4.626068480629312418 ) ) ;
#12678 = FACE_OUTER_BOUND ( 'NONE', #33567, .T. ) ;
#12679 = CARTESIAN_POINT ( 'NONE',  ( 2.119043635923744784, -33.04480253866695705, 6.971170733404100872 ) ) ;
#12680 = ORIENTED_EDGE ( 'NONE', *, *, #14574, .T. ) ;
#12681 = CARTESIAN_POINT ( 'NONE',  ( 26.50466346464379086, 1.691181880056894737, 4.311557507100089559 ) ) ;
#12682 = SHAPE_REPRESENTATION_RELATIONSHIP ( 'NONE' , 'NONE' ,  #32460, #31867 ) ;
#12683 = EDGE_CURVE ( 'NONE', #39450, #32407, #35823, .T. ) ;
#12684 = LINE ( 'NONE', #37790, #37133 ) ;
#12685 = EDGE_LOOP ( 'NONE', ( #18921, #14335, #10105, #7395 ) ) ;
#12686 = DIRECTION ( 'NONE',  ( -0.000000000000000000, 0.000000000000000000, 1.000000000000000000 ) ) ;
#12687 = EDGE_CURVE ( 'NONE', #35977, #20092, #16313, .T. ) ;
#12688 = EDGE_LOOP ( 'NONE', ( #14952, #14458, #32153, #8188 ) ) ;
#12689 = CARTESIAN_POINT ( 'NONE',  ( 79.20958446297056810, 65.00485465208042513, -3.275607309966719338 ) ) ;
#12690 = CARTESIAN_POINT ( 'NONE',  ( 4.792526203416204389, -27.93020634197934982, 7.750000000000000888 ) ) ;
#12691 = CARTESIAN_POINT ( 'NONE',  ( 80.99919828920802445, 61.56308015027072145, 2.277920705665342993 ) ) ;
#12695 = EDGE_LOOP ( 'NONE', ( #14818, #9445, #9175, #30546 ) ) ;
#12694 = VERTEX_POINT ( 'NONE', #38327 ) ;
#12693 = CARTESIAN_POINT ( 'NONE',  ( -70.92837670882107659, -37.87473357531881391, 0.000000000000000000 ) ) ;
#12692 = VECTOR ( 'NONE', #37963, 1000.000000000000000 ) ;
#12696 = EDGE_CURVE ( 'NONE', #24696, #16350, #22715, .T. ) ;
#12698 = ADVANCED_FACE ( 'NONE', ( #26597 ), #3789, .T. ) ;
#12697 = CARTESIAN_POINT ( 'NONE',  ( -2.297321782777200561, -26.28614060416741438, 7.695279973900954751 ) ) ;
#12699 = DIRECTION ( 'NONE',  ( -0.000000000000000000, -1.000000000000000000, -0.000000000000000000 ) ) ;
#12700 = DIRECTION ( 'NONE',  ( 0.1736481776669404897, -0.9848077530122062440, -0.000000000000000000 ) ) ;
#12701 = LINE ( 'NONE', #25275, #3146 ) ;
#12702 = CARTESIAN_POINT ( 'NONE',  ( 21.99292708584655998, 5.590793479290228518, -3.105521760628916272 ) ) ;
#12703 = VERTEX_POINT ( 'NONE', #13228 ) ;
#12704 = CARTESIAN_POINT ( 'NONE',  ( -64.84514717441444986, 36.26677316194228951, -6.475000919363135488 ) ) ;
#12705 = VERTEX_POINT ( 'NONE', #32789 ) ;
#12706 = CARTESIAN_POINT ( 'NONE',  ( 7.021324086407807030, -26.64985754041175525, 6.700000000000000178 ) ) ;
#12707 = CARTESIAN_POINT ( 'NONE',  ( -1.652934641495917178, -29.00849165296052234, 7.661510568013094158 ) ) ;
#12708 = AXIS2_PLACEMENT_3D ( 'NONE', #25639, #20064, #19860 ) ;
#12709 = DIRECTION ( 'NONE',  ( -0.000000000000000000, -0.000000000000000000, 1.000000000000000000 ) ) ;
#12710 = CARTESIAN_POINT ( 'NONE',  ( -68.98442902999595105, 21.93515443114010210, -8.800414904976364028 ) ) ;
#12711 = CARTESIAN_POINT ( 'NONE',  ( 79.10630237408686583, 66.00617110148432687, 2.043563575549256495 ) ) ;
#12712 = CARTESIAN_POINT ( 'NONE',  ( 87.82658540711466344, -2.392274210255118216, -1.851534029869310816 ) ) ;
#12713 = CARTESIAN_POINT ( 'NONE',  ( -0.5767923600352592439, -26.91202874155498037, 7.695279973900954751 ) ) ;
#12714 = EDGE_LOOP ( 'NONE', ( #37433, #13169, #24068, #21564, #13752, #13002 ) ) ;
#12715 = CARTESIAN_POINT ( 'NONE',  ( 2.873744954996579892, -26.27246564945127716, 7.651421919295144036 ) ) ;
#12716 = CARTESIAN_POINT ( 'NONE',  ( 4.598967362590697050, -31.34707672027869307, 7.778050822775632867 ) ) ;
#12717 = AXIS2_PLACEMENT_3D ( 'NONE', #15588, #34153, #28141 ) ;
#12718 = CARTESIAN_POINT ( 'NONE',  ( 4.052584231663811210, -26.97816100332664035, 6.870724624169668004 ) ) ;
#12719 = DIRECTION ( 'NONE',  ( 0.000000000000000000, 0.000000000000000000, -1.000000000000000000 ) ) ;
#12720 = DIRECTION ( 'NONE',  ( 0.000000000000000000, 0.000000000000000000, -1.000000000000000000 ) ) ;
#12721 = LINE ( 'NONE', #37423, #3016 ) ;
#12722 = ORIENTED_EDGE ( 'NONE', *, *, #33278, .T. ) ;
#12723 = CARTESIAN_POINT ( 'NONE',  ( 36.42079407071754815, -3.114107480780474280, 5.890743773605413125 ) ) ;
#12724 = CARTESIAN_POINT ( 'NONE',  ( 87.54465900634191655, 0.02340848060778613626, -4.593250482506632260 ) ) ;
#12725 = EDGE_LOOP ( 'NONE', ( #2810, #29199, #5005, #32306 ) ) ;
#12726 = CARTESIAN_POINT ( 'NONE',  ( 81.13780861853922488, 61.29235415973831635, -1.171933751919293831 ) ) ;
#12727 = CARTESIAN_POINT ( 'NONE',  ( -1.339690083386215758, -31.27506463679495496, 7.785096263473212375 ) ) ;
#12728 = CARTESIAN_POINT ( 'NONE',  ( 2.931185808669443116, -32.84638282411072652, 7.686927408461905920 ) ) ;
#12729 = ORIENTED_EDGE ( 'NONE', *, *, #9428, .T. ) ;
#12730 = CARTESIAN_POINT ( 'NONE',  ( -1.652160870483347921, -29.00385851250623404, 7.740055089680398126 ) ) ;
#12731 = ORIENTED_EDGE ( 'NONE', *, *, #8343, .T. ) ;
#12732 = CARTESIAN_POINT ( 'NONE',  ( -71.83276077574569740, 0.9916882426457708233, 9.959148848844533219 ) ) ;
#12733 = AXIS2_PLACEMENT_3D ( 'NONE', #23955, #8923, #12222 ) ;
#12734 = VECTOR ( 'NONE', #2956, 1000.000000000000114 ) ;
#12735 = ORIENTED_EDGE ( 'NONE', *, *, #25028, .F. ) ;
#12736 = CARTESIAN_POINT ( 'NONE',  ( 79.57367618494546946, 64.93149010139244126, -3.380189700376623474 ) ) ;
#12737 = CARTESIAN_POINT ( 'NONE',  ( -71.80187797986816634, -0.2787227296414631073, 5.936291904728147273 ) ) ;
#12739 = CARTESIAN_POINT ( 'NONE',  ( 31.10600218134772987, 0.6115860487915156796, 4.541982612545634623 ) ) ;
#12738 = CARTESIAN_POINT ( 'NONE',  ( 22.04424169242247089, 2.368281942274926166, 5.447058248131960490 ) ) ;
#12740 = ORIENTED_EDGE ( 'NONE', *, *, #19659, .T. ) ;
#12741 = CARTESIAN_POINT ( 'NONE',  ( 79.21008177357728641, 66.23692415242760489, -1.465632304122640228 ) ) ;
#12742 = EDGE_CURVE ( 'NONE', #25329, #38606, #14771, .T. ) ;
#12743 = VECTOR ( 'NONE', #24799, 1000.000000000000000 ) ;
#12745 = EDGE_CURVE ( 'NONE', #18362, #13356, #38734, .T. ) ;
#12744 = CARTESIAN_POINT ( 'NONE',  ( 4.705320599239643187, -27.97917511340586927, 6.863904403958575706 ) ) ;
#12747 = CARTESIAN_POINT ( 'NONE',  ( 85.65652580503477509, 2.144249308523916042, -3.546142381197787241 ) ) ;
#12746 = CARTESIAN_POINT ( 'NONE',  ( 4.882868366733327470, -28.37333834040810032, 7.693875151218753317 ) ) ;
#12748 = CARTESIAN_POINT ( 'NONE',  ( 1.700390093233090871, -29.56993018339339940, 7.750000000000000888 ) ) ;
#12749 = CARTESIAN_POINT ( 'NONE',  ( 0.4917814316705931832, -26.28522446336723561, 7.756742906098588186 ) ) ;
#12750 = CARTESIAN_POINT ( 'NONE',  ( 69.50581201620700256, 59.72791825745761685, 3.883859131414829413 ) ) ;
#12751 = CARTESIAN_POINT ( 'NONE',  ( 24.36246139054879833, 2.879672585629011738, -3.789350523822255568 ) ) ;
#12752 = ORIENTED_EDGE ( 'NONE', *, *, #39407, .T. ) ;
#12753 = CARTESIAN_POINT ( 'NONE',  ( 21.85643539959779957, -10.54057479330554159, -5.012605957032298498 ) ) ;
#12754 = CARTESIAN_POINT ( 'NONE',  ( -57.69456667414278428, 32.53259245237469344, -4.116672578207452915 ) ) ;
#12755 = DIRECTION ( 'NONE',  ( 0.8459487642040750544, 0.000000000000000000, -0.5332641825039424743 ) ) ;
#12756 = CARTESIAN_POINT ( 'NONE',  ( 79.35885969106158200, 66.15515411851721694, 1.832274617051027121 ) ) ;
#12757 = CARTESIAN_POINT ( 'NONE',  ( 87.85599567641696694, -0.3262996441500809475, -4.386575958041428080 ) ) ;
#12758 = ORIENTED_EDGE ( 'NONE', *, *, #26497, .F. ) ;
#12759 = CARTESIAN_POINT ( 'NONE',  ( 10.58508780786439374, 19.59913305159139441, 2.500000000000000000 ) ) ;
#12760 = CARTESIAN_POINT ( 'NONE',  ( 33.94050681485320098, -3.428830454661854432, 5.491199649958280027 ) ) ;
#12761 = AXIS2_PLACEMENT_3D ( 'NONE', #10459, #23040, #35606 ) ;
#12762 = VECTOR ( 'NONE', #32424, 1000.000000000000000 ) ;
#12763 = CARTESIAN_POINT ( 'NONE',  ( 36.91076444475422136, -2.639566709576531611, -5.967215500452092591 ) ) ;
#12764 = CARTESIAN_POINT ( 'NONE',  ( 3.412070287718869999, -32.50764203308273181, 7.635761828346577573 ) ) ;
#12765 = CARTESIAN_POINT ( 'NONE',  ( -36.87867591359218977, -26.64985754041175525, 6.700000000000000178 ) ) ;
#12766 = CARTESIAN_POINT ( 'NONE',  ( 4.404516770028684469, -31.79202354683301834, 7.695279973900954751 ) ) ;
#12767 = ORIENTED_EDGE ( 'NONE', *, *, #4660, .T. ) ;
#12768 = CARTESIAN_POINT ( 'NONE',  ( 1.700390093233090871, -29.56993018339339940, 7.800000000000000711 ) ) ;
#12769 = CIRCLE ( 'NONE', #17363, 3.499999999999999556 ) ;
#12770 = CARTESIAN_POINT ( 'NONE',  ( -1.283534637189521543, -31.19973968173253098, 7.782034975670475418 ) ) ;
#12771 = CARTESIAN_POINT ( 'NONE',  ( 1.021324086407808585, -26.64985754041175525, 6.700000000000000178 ) ) ;
#12772 = EDGE_LOOP ( 'NONE', ( #38357, #10753, #33911, #39489 ) ) ;
#12773 = VECTOR ( 'NONE', #10311, 1000.000000000000000 ) ;
#12774 = ORIENTED_EDGE ( 'NONE', *, *, #40218, .F. ) ;
#12775 = CARTESIAN_POINT ( 'NONE',  ( 37.00880725212909539, -2.250639250997623630, 5.913624440729033260 ) ) ;
#12776 = CARTESIAN_POINT ( 'NONE',  ( 4.839780649812301938, -28.24624522621548195, 7.139196562012268821 ) ) ;
#12777 = CARTESIAN_POINT ( 'NONE',  ( 66.55809347730310321, 57.86716763633229021, -3.999802976172705193 ) ) ;
#12778 = ORIENTED_EDGE ( 'NONE', *, *, #9592, .F. ) ;
#12779 = CARTESIAN_POINT ( 'NONE',  ( 88.20160905653106909, -0.7145089964949031813, -2.080387601684223320 ) ) ;
#12780 = CARTESIAN_POINT ( 'NONE',  ( 1.295029243323604806, -26.19418099523372945, 7.013842709614101167 ) ) ;
#12781 = CARTESIAN_POINT ( 'NONE',  ( 4.939155359955127444, -28.53528083619306699, 6.865312560952603782 ) ) ;
#12782 = ORIENTED_EDGE ( 'NONE', *, *, #23306, .F. ) ;
#12783 = FACE_OUTER_BOUND ( 'NONE', #14182, .T. ) ;
#12784 = CARTESIAN_POINT ( 'NONE',  ( -58.99948754145754037, 28.61410076184115070, -6.947368380125259257 ) ) ;
#12785 = EDGE_LOOP ( 'NONE', ( #7229, #37012, #2916, #8808 ) ) ;
#12786 = CARTESIAN_POINT ( 'NONE',  ( 23.15296705429070556, 3.944850500700754825, 3.230105547710554248 ) ) ;
#12787 = CARTESIAN_POINT ( 'NONE',  ( 81.72179206571539112, 61.68197623675723662, -1.214491505233944002 ) ) ;
#12789 = TOROIDAL_SURFACE ( 'NONE', #22690, 3.778021175560965172, 0.2000000000000000111 ) ;
#12788 = CARTESIAN_POINT ( 'NONE',  ( 79.86701161339794908, 64.38869582053085594, 3.619557188109057133 ) ) ;
#12790 = VECTOR ( 'NONE', #27444, 1000.000000000000000 ) ;
#12792 = EDGE_CURVE ( 'NONE', #14030, #4303, #35282, .T. ) ;
#12791 = CARTESIAN_POINT ( 'NONE',  ( 2.873739498108726309, -26.37879873393239905, 7.775108481317164255 ) ) ;
#12793 = ORIENTED_EDGE ( 'NONE', *, *, #1649, .T. ) ;
#12794 = CARTESIAN_POINT ( 'NONE',  ( 77.53347081925224415, 60.09046002684883803, -2.805892758502992468 ) ) ;
#12796 = CARTESIAN_POINT ( 'NONE',  ( -55.16612787639756732, 31.23053227951973199, 1.484562114140385747 ) ) ;
#12795 = CARTESIAN_POINT ( 'NONE',  ( -37.07867591359219261, -26.64985754041175525, 6.700000000000000178 ) ) ;
#12797 = CARTESIAN_POINT ( 'NONE',  ( 14.71117645488784120, 12.53769967753948578, -2.502432895569043136 ) ) ;
#12798 = CARTESIAN_POINT ( 'NONE',  ( 80.03255827398538713, 65.21842193378445529, -3.211742283750908644 ) ) ;
#12799 = CARTESIAN_POINT ( 'NONE',  ( 77.48714025262371763, 64.49898405264991652, 3.102003663616900830 ) ) ;
#12800 = EDGE_LOOP ( 'NONE', ( #36155, #4073 ) ) ;
#12801 = ORIENTED_EDGE ( 'NONE', *, *, #16275, .T. ) ;
#12802 = VECTOR ( 'NONE', #15785, 1000.000000000000000 ) ;
#12803 = DIRECTION ( 'NONE',  ( -0.000000000000000000, -1.000000000000000000, -0.000000000000000000 ) ) ;
#12804 = CARTESIAN_POINT ( 'NONE',  ( -59.00110696496997775, 28.68040728033253473, 6.866925925439470113 ) ) ;
#12805 = CARTESIAN_POINT ( 'NONE',  ( 82.39984057372362258, 63.46184634947046987, 2.021051955676536505 ) ) ;
#12807 = CARTESIAN_POINT ( 'NONE',  ( 17.62552235143947854, 11.92971608769965997, 2.500000000000007550 ) ) ;
#12806 = CARTESIAN_POINT ( 'NONE',  ( 4.305930965742039263, -31.90684198354446721, 6.865482280155368322 ) ) ;
#12808 = CARTESIAN_POINT ( 'NONE',  ( 29.95345716813442749, -1.222334143750352764, -6.038643835265099291 ) ) ;
#12809 = CARTESIAN_POINT ( 'NONE',  ( -5.078675913592192614, -26.64985754041175525, 6.700000000000000178 ) ) ;
#12810 = CARTESIAN_POINT ( 'NONE',  ( 19.23685618013880472, -6.968822543817719151, 2.500000000000000444 ) ) ;
#12811 = CARTESIAN_POINT ( 'NONE',  ( -64.25913952751501768, 36.58001704789108288, 5.467911005455182938 ) ) ;
#12812 = DIRECTION ( 'NONE',  ( 0.000000000000000000, 0.000000000000000000, 1.000000000000000000 ) ) ;
#12813 = CARTESIAN_POINT ( 'NONE',  ( -0.6395917686905666644, -32.03660811739485581, 6.979335674598003969 ) ) ;
#12814 = DIRECTION ( 'NONE',  ( 1.000000000000000000, 0.000000000000000000, 0.000000000000000000 ) ) ;
#12815 = CARTESIAN_POINT ( 'NONE',  ( 36.84678844362374406, -3.231065898219810162, -5.943761196008794379 ) ) ;
#12816 = DIRECTION ( 'NONE',  ( 1.000000000000000000, -0.000000000000000000, 0.000000000000000000 ) ) ;
#12817 = CARTESIAN_POINT ( 'NONE',  ( -0.8920574397464721139, -31.76975194634333732, 7.748216051605121280 ) ) ;
#12818 = CARTESIAN_POINT ( 'NONE',  ( 23.83223587884036831, -2.668011125867791211, -3.925994812332605388 ) ) ;
#12819 = LINE ( 'NONE', #22318, #39771 ) ;
#12820 = EDGE_CURVE ( 'NONE', #301, #10798, #8838, .T. ) ;
#12821 = LINE ( 'NONE', #6463, #25449 ) ;
#12822 = AXIS2_PLACEMENT_3D ( 'NONE', #27956, #34582, #8802 ) ;
#12823 = CARTESIAN_POINT ( 'NONE',  ( 3.021324086407803478, -24.55319635012989110, 6.800000000000000711 ) ) ;
#12824 = AXIS2_PLACEMENT_3D ( 'NONE', #37614, #24247, #12302 ) ;
#12826 = VERTEX_POINT ( 'NONE', #13633 ) ;
#12825 = VECTOR ( 'NONE', #28524, 1000.000000000000114 ) ;
#12827 = EDGE_CURVE ( 'NONE', #8844, #19268, #11316, .T. ) ;
#12828 = VERTEX_POINT ( 'NONE', #18119 ) ;
#12829 = CARTESIAN_POINT ( 'NONE',  ( -70.92837670882107659, -65.19654454972992141, -6.000000000000002665 ) ) ;
#12830 = CARTESIAN_POINT ( 'NONE',  ( 67.92345958529671179, 58.66354838738842403, -3.978477839347868361 ) ) ;
#12831 = AXIS2_PLACEMENT_3D ( 'NONE', #17177, #17994, #33674 ) ;
#12832 = EDGE_CURVE ( 'NONE', #33252, #10847, #27637, .T. ) ;
#12833 = ORIENTED_EDGE ( 'NONE', *, *, #351, .F. ) ;
#12834 = LINE ( 'NONE', #31788, #16684 ) ;
#12835 = CARTESIAN_POINT ( 'NONE',  ( -12.97867591359219297, -26.64985754041175525, 6.800000000000000711 ) ) ;
#12836 = CARTESIAN_POINT ( 'NONE',  ( 21.85231751869008932, 4.115031571714823144, 4.273325978632851907 ) ) ;
#12837 = CARTESIAN_POINT ( 'NONE',  ( 5.026985514822023937, -28.48192149727754696, 6.865482280155368322 ) ) ;
#12838 = CARTESIAN_POINT ( 'NONE',  ( 3.574567904444611255, -26.61401111617210802, 6.875780273367531947 ) ) ;
#12839 = FACE_OUTER_BOUND ( 'NONE', #35044, .T. ) ;
#12840 = ORIENTED_EDGE ( 'NONE', *, *, #33683, .T. ) ;
#12841 = CARTESIAN_POINT ( 'NONE',  ( 23.14138885347819041, 4.047734147674228566, 3.078156626778878469 ) ) ;
#12842 = PLANE ( 'NONE',  #13592 ) ;
#12843 = VERTEX_POINT ( 'NONE', #14829 ) ;
#12845 = EDGE_CURVE ( 'NONE', #16562, #6115, #39958, .T. ) ;
#12844 = CARTESIAN_POINT ( 'NONE',  ( 0.4761165981717114803, -26.29103488020206569, 7.730015791551946513 ) ) ;
#12846 = ORIENTED_EDGE ( 'NONE', *, *, #407, .F. ) ;
#12847 = CARTESIAN_POINT ( 'NONE',  ( 80.12095330986326758, 62.19218463582609502, -3.375657603866087264 ) ) ;
#12849 = CARTESIAN_POINT ( 'NONE',  ( -1.675495590043027727, -29.97419347324715133, 6.895222827070023541 ) ) ;
#12848 = CARTESIAN_POINT ( 'NONE',  ( 27.28763074894343887, 1.166087062639404870, 4.463145202650028232 ) ) ;
#12850 = CARTESIAN_POINT ( 'NONE',  ( 81.44856608406118426, 64.08396523683251189, -3.179853676209052793 ) ) ;
#12851 = CARTESIAN_POINT ( 'NONE',  ( 78.35540530300707474, 65.82096406625564100, 1.612955153530279295 ) ) ;
#12852 = CIRCLE ( 'NONE', #26031, 4.075022672948151126 ) ;
#12853 = VECTOR ( 'NONE', #13550, 1000.000000000000000 ) ;
#12854 = PLANE ( 'NONE',  #34418 ) ;
#12855 =( BOUNDED_SURFACE ( )  B_SPLINE_SURFACE ( 3, 2, ( 
 ( #25679, #31664, #3680 ),
 ( #37814, #12298, #25282 ),
 ( #21992, #31261, #2865 ),
 ( #12913, #3479, #34973 ),
 ( #6550, #24871, #31461 ),
 ( #21786, #9826, #582 ),
 ( #34772, #28570, #377 ),
 ( #22206, #13121, #37410 ),
 ( #16005, #15388, #173 ),
 ( #34364, #9619, #15806 ),
 ( #34570, #9002, #21582 ),
 ( #27943, #31054, #25480 ),
 ( #38025, #9206, #6747 ),
 ( #34164, #6344, #19298 ),
 ( #28775, #40486, #31869 ),
 ( #6134, #5930, #18674 ),
 ( #18893, #3077, #15597 ),
 ( #28149, #40703, #12504 ),
 ( #25079, #37609, #28360 ),
 ( #20287, #32279, #1579 ),
 ( #23194, #32871, #35766 ),
 ( #23393, #4269, #10619 ),
 ( #29373, #26489, #14110 ),
 ( #16792, #1193, #13730 ),
 ( #29571, #32470, #3885 ),
 ( #32672, #7539, #26293 ),
 ( #35959, #1387, #778 ),
 ( #16401, #38223, #4661 ),
 ( #4079, #7740, #13309 ),
 ( #28975, #35171, #25882 ),
 ( #16592, #10020, #38421 ),
 ( #20095, #10222, #6944 ),
 ( #38629, #19506, #17197 ),
 ( #38825, #4473, #29764 ),
 ( #22805, #32081, #16994 ),
 ( #13918, #35375, #39014 ),
 ( #7143, #19704, #10818 ),
 ( #29175, #22603, #984 ),
 ( #13520, #26091, #10427 ),
 ( #23003, #35570, #7339 ),
 ( #19898, #8742, #27087 ),
 ( #36158, #40048, #21326 ),
 ( #2614, #5262, #30173 ),
 ( #33071, #21122, #27285 ),
 ( #11822, #33494, #39850 ),
 ( #17803, #14930, #30809 ),
 ( #30388, #2193, #14711 ),
 ( #18012, #20908, #4856 ),
 ( #33690, #11618, #24197 ),
 ( #24406, #30600, #29970 ),
 ( #36756, #8542, #23594 ),
 ( #20697, #36962, #1784 ),
 ( #17388, #7937, #14312 ),
 ( #5061, #5469, #33901 ),
 ( #20489, #5675, #2409 ),
 ( #8126, #27498, #26882 ),
 ( #39424, #23983, #17594 ),
 ( #18217, #26689, #11214 ),
 ( #39223, #11013, #23780 ),
 ( #36359, #33280, #1995 ),
 ( #8333, #14513, #39634 ),
 ( #11419, #36554, #3238 ),
 ( #34113, #127, #15754 ),
 ( #18839, #2814, #25029 ),
 ( #25431, #15548, #25234 ),
 ( #22360, #37765, #34926 ),
 ( #15954, #31009, #40245 ),
 ( #12458, #6086, #18421 ) ),
 .UNSPECIFIED., .F., .F., .T. ) 
 B_SPLINE_SURFACE_WITH_KNOTS ( ( 4, 2, 2, 2, 2, 2, 2, 2, 2, 2, 2, 2, 2, 2, 2, 2, 2, 2, 2, 2, 2, 2, 2, 2, 2, 2, 2, 2, 2, 2, 2, 2, 2, 4 ),
 ( 3, 3 ),
 ( 0.04252856423674911124, 0.04385758186914752443, 0.04518659950154593069, 0.04651561713394433695, 0.04784463476634275014, 0.05050267003113956960, 0.05116717884733877619, 0.05183168766353797585, 0.05316070529593638905, 0.05382521411213559565, 0.05448972292833480224, 0.05581874056073320850, 0.05648324937693241510, 0.05714775819313161476, 0.05847677582553002795, 0.05980579345792844115, 0.06113481109032684740, 0.06246382872272525366, 0.06379284635512366686, 0.06512186398752208005, 0.06645088161992049325, 0.06777989925231889257, 0.06910891688471730576, 0.07043793451711571896, 0.07176695214951411828, 0.07309596978191253147, 0.07442498741431094467, 0.07575400504670935786, 0.07708302267910777106, 0.07841204031150618425, 0.07974105794390459745, 0.08107007557630301064, 0.08239909320870142384, 0.08505712847349823635 ),
 ( 0.000000000000000000, 1.000000000000000000 ),
 .UNSPECIFIED. ) 
 GEOMETRIC_REPRESENTATION_ITEM ( )  RATIONAL_B_SPLINE_SURFACE ( (
 ( 1.000000000000000000, 0.7442417417348949904, 1.000000000000000000),
 ( 1.000000000000000000, 0.7431783020712605659, 1.000000000000000000),
 ( 1.000000000000000000, 0.7409760979376766032, 1.000000000000000000),
 ( 1.000000000000000000, 0.7345856213530946865, 1.000000000000000000),
 ( 1.000000000000000000, 0.7304004294511651230, 1.000000000000000000),
 ( 1.000000000000000000, 0.7203431566566479427, 1.000000000000000000),
 ( 1.000000000000000000, 0.7144690456092649411, 1.000000000000000000),
 ( 1.000000000000000000, 0.7013913408706143882, 1.000000000000000000),
 ( 1.000000000000000000, 0.6941559842080995413, 1.000000000000000000),
 ( 1.000000000000000000, 0.6719163496680571335, 1.000000000000000000),
 ( 1.000000000000000000, 0.6561249043233500222, 1.000000000000000000),
 ( 1.000000000000000000, 0.6392825574178745418, 1.000000000000000000),
 ( 1.000000000000000000, 0.6360685153987252205, 1.000000000000000000),
 ( 1.000000000000000000, 0.6301773797663908772, 1.000000000000000000),
 ( 1.000000000000000000, 0.6274839287509237362, 1.000000000000000000),
 ( 1.000000000000000000, 0.6202923972654608153, 1.000000000000000000),
 ( 1.000000000000000000, 0.6166918370340956912, 1.000000000000000000),
 ( 1.000000000000000000, 0.6134846856060413023, 1.000000000000000000),
 ( 1.000000000000000000, 0.6127846890635409993, 1.000000000000000000),
 ( 1.000000000000000000, 0.6121417544835984215, 1.000000000000000000),
 ( 1.000000000000000000, 0.6121919490915220807, 1.000000000000000000),
 ( 1.000000000000000000, 0.6133751910668664431, 1.000000000000000000),
 ( 1.000000000000000000, 0.6155490712539813947, 1.000000000000000000),
 ( 1.000000000000000000, 0.6203878072413371303, 1.000000000000000000),
 ( 1.000000000000000000, 0.6222638419436984369, 1.000000000000000000),
 ( 1.000000000000000000, 0.6263429184244624359, 1.000000000000000000),
 ( 1.000000000000000000, 0.6285529934538920394, 1.000000000000000000),
 ( 1.000000000000000000, 0.6354958318040264675, 1.000000000000000000),
 ( 1.000000000000000000, 0.6405374649603885473, 1.000000000000000000),
 ( 1.000000000000000000, 0.6504850597404820967, 1.000000000000000000),
 ( 1.000000000000000000, 0.6552989879275363805, 1.000000000000000000),
 ( 1.000000000000000000, 0.6637694919636900615, 1.000000000000000000),
 ( 1.000000000000000000, 0.6674481112988286391, 1.000000000000000000),
 ( 1.000000000000000000, 0.6731606607313684876, 1.000000000000000000),
 ( 1.000000000000000000, 0.6751501093762943828, 1.000000000000000000),
 ( 1.000000000000000000, 0.6771367351906749654, 1.000000000000000000),
 ( 1.000000000000000000, 0.6771517807286357993, 1.000000000000000000),
 ( 1.000000000000000000, 0.6751929488707926197, 1.000000000000000000),
 ( 1.000000000000000000, 0.6731945361681611617, 1.000000000000000000),
 ( 1.000000000000000000, 0.6675581016157797754, 1.000000000000000000),
 ( 1.000000000000000000, 0.6639163920490709359, 1.000000000000000000),
 ( 1.000000000000000000, 0.6554729574460654851, 1.000000000000000000),
 ( 1.000000000000000000, 0.6506196326805566699, 1.000000000000000000),
 ( 1.000000000000000000, 0.6407412944952491918, 1.000000000000000000),
 ( 1.000000000000000000, 0.6357223030003761322, 1.000000000000000000),
 ( 1.000000000000000000, 0.6264724816114001227, 1.000000000000000000),
 ( 1.000000000000000000, 0.6222236727237925313, 1.000000000000000000),
 ( 1.000000000000000000, 0.6156853169344688181, 1.000000000000000000),
 ( 1.000000000000000000, 0.6134690707966352630, 1.000000000000000000),
 ( 1.000000000000000000, 0.6117931279243551401, 1.000000000000000000),
 ( 1.000000000000000000, 0.6123370218337945703, 1.000000000000000000),
 ( 1.000000000000000000, 0.6165118084860213843, 1.000000000000000000),
 ( 1.000000000000000000, 0.6200744837291712885, 1.000000000000000000),
 ( 1.000000000000000000, 0.6295916762275356460, 1.000000000000000000),
 ( 1.000000000000000000, 0.6355670384684388718, 1.000000000000000000),
 ( 1.000000000000000000, 0.6490362627856776090, 1.000000000000000000),
 ( 1.000000000000000000, 0.6564052266140359970, 1.000000000000000000),
 ( 1.000000000000000000, 0.6715002995394828700, 1.000000000000000000),
 ( 1.000000000000000000, 0.6792468330939857024, 1.000000000000000000),
 ( 1.000000000000000000, 0.6942451427572285949, 1.000000000000000000),
 ( 1.000000000000000000, 0.7013942707229733342, 1.000000000000000000),
 ( 1.000000000000000000, 0.7144494188210194219, 1.000000000000000000),
 ( 1.000000000000000000, 0.7203582787926783304, 1.000000000000000000),
 ( 1.000000000000000000, 0.7305132205854709682, 1.000000000000000000),
 ( 1.000000000000000000, 0.7347357360980601992, 1.000000000000000000),
 ( 1.000000000000000000, 0.7442195004274780867, 1.000000000000000000),
 ( 1.000000000000000000, 0.7464355310270405219, 1.000000000000000000),
 ( 1.000000000000000000, 0.7441515679388579496, 1.000000000000000000) ) ) 
 REPRESENTATION_ITEM ( '' )  SURFACE ( )  );
#12856 = CARTESIAN_POINT ( 'NONE',  ( 4.732352950855482909, -31.12399458443864120, 7.139196562012272373 ) ) ;
#12857 = CARTESIAN_POINT ( 'NONE',  ( 25.51884215448320958, -4.718317418738882552, 0.4603789867971156413 ) ) ;
#12858 = CARTESIAN_POINT ( 'NONE',  ( 5.103179151787565537, -29.39980800500447344, 7.139196562012274150 ) ) ;
#12859 = ORIENTED_EDGE ( 'NONE', *, *, #24489, .T. ) ;
#12860 = CARTESIAN_POINT ( 'NONE',  ( -74.02829583808838265, 6.653335707795791087, 9.562392075533951541 ) ) ;
#12861 = CARTESIAN_POINT ( 'NONE',  ( -11.07867591359219794, -26.64985754041175525, 6.800000000000000711 ) ) ;
#12862 = ORIENTED_EDGE ( 'NONE', *, *, #31206, .F. ) ;
#12863 = VECTOR ( 'NONE', #19504, 1000.000000000000114 ) ;
#12864 = EDGE_CURVE ( 'NONE', #4851, #24034, #36871, .T. ) ;
#12865 = ORIENTED_EDGE ( 'NONE', *, *, #23790, .F. ) ;
#12866 = CARTESIAN_POINT ( 'NONE',  ( 1.610624680721678414, -32.96874500193186464, 7.778050822775632867 ) ) ;
#12867 = CARTESIAN_POINT ( 'NONE',  ( 28.18609449851297910, -3.183177124052247287, -4.605519748400973334 ) ) ;
#12868 = CARTESIAN_POINT ( 'NONE',  ( 36.20103906056434795, -3.651302259472223533, -5.717550162322121210 ) ) ;
#12869 = CARTESIAN_POINT ( 'NONE',  ( -1.560095160591656205, -30.53389918434378458, 6.969307238440510588 ) ) ;
#12870 = CARTESIAN_POINT ( 'NONE',  ( 3.394528066554050927, -32.63260504671350759, 6.870737987065015595 ) ) ;
#12871 = CARTESIAN_POINT ( 'NONE',  ( 19.96668899214778747, 6.747717534392478456, 3.285463770674537543 ) ) ;
#12872 = CARTESIAN_POINT ( 'NONE',  ( 5.195169754196312439, -29.76104218084410036, 6.971170733404093767 ) ) ;
#12873 = CARTESIAN_POINT ( 'NONE',  ( 28.67087680535204797, -4.024283280459782119, 4.110896467804376009 ) ) ;
#12874 = LINE ( 'NONE', #6712, #3332 ) ;
#12875 = DIRECTION ( 'NONE',  ( -0.000000000000000000, -0.000000000000000000, 1.000000000000000000 ) ) ;
#12876 = MANIFOLD_SOLID_BREP ( 'Boss-Extrude14', #22940 ) ;
#12877 = CARTESIAN_POINT ( 'NONE',  ( 22.48654264114678369, 0.6042035298600259008, -6.567991110914350728 ) ) ;
#12878 = CARTESIAN_POINT ( 'NONE',  ( 30.85399364833475744, -3.769658692124774113, -4.573109180878241808 ) ) ;
#12879 = DIRECTION ( 'NONE',  ( -0.000000000000000000, -1.000000000000000000, -0.000000000000000000 ) ) ;
#12880 = ORIENTED_EDGE ( 'NONE', *, *, #6414, .T. ) ;
#12881 = ADVANCED_FACE ( 'NONE', ( #40156 ), #27194, .F. ) ;
#12883 = EDGE_CURVE ( 'NONE', #4585, #22121, #8043, .T. ) ;
#12882 = CARTESIAN_POINT ( 'NONE',  ( 66.88885785885000246, 57.86870549787170859, 3.998465113252547720 ) ) ;
#12884 = ADVANCED_FACE ( 'NONE', ( #15041 ), #36267, .F. ) ;
#12885 = AXIS2_PLACEMENT_3D ( 'NONE', #28107, #31416, #9166 ) ;
#12886 = CARTESIAN_POINT ( 'NONE',  ( -28.24874870218063805, -26.64985754041175525, 6.800000000000000711 ) ) ;
#12887 = AXIS2_PLACEMENT_3D ( 'NONE', #28026, #2949, #8876 ) ;
#12888 = CARTESIAN_POINT ( 'NONE',  ( 87.06687503756165825, -0.7302844941506287935, -5.541598948305895611 ) ) ;
#12889 = LINE ( 'NONE', #25256, #37913 ) ;
#12890 = ORIENTED_EDGE ( 'NONE', *, *, #38711, .T. ) ;
#12891 = CARTESIAN_POINT ( 'NONE',  ( 24.67487267398843542, 2.663866308026491492, 3.912183617538783409 ) ) ;
#12892 = CARTESIAN_POINT ( 'NONE',  ( 24.98423877875683985, 3.112984909006376810, -2.906875866008173936 ) ) ;
#12893 = CARTESIAN_POINT ( 'NONE',  ( 11.65737507970504439, -23.60493063168009442, 6.800000000000000711 ) ) ;
#12894 = EDGE_LOOP ( 'NONE', ( #2219, #23507, #26684, #12326 ) ) ;
#12895 = CARTESIAN_POINT ( 'NONE',  ( 3.999421017872402562, -26.94725929646187268, 7.782861076432729952 ) ) ;
#12896 = VERTEX_POINT ( 'NONE', #39541 ) ;
#12897 = CARTESIAN_POINT ( 'NONE',  ( 80.51397140397763508, 62.59311809350356981, -3.432573985763844426 ) ) ;
#12898 = CARTESIAN_POINT ( 'NONE',  ( -1.697910808162383267, -29.46219841264419514, 7.768425012602595103 ) ) ;
#12899 = CARTESIAN_POINT ( 'NONE',  ( 80.90366483818405641, 61.70104970548236878, 2.590854534519439145 ) ) ;
#12901 = ORIENTED_EDGE ( 'NONE', *, *, #26104, .T. ) ;
#12900 = CARTESIAN_POINT ( 'NONE',  ( -1.699609906766908596, -29.72725013975003350, 7.398254066345574920 ) ) ;
#12902 = CARTESIAN_POINT ( 'NONE',  ( -57.37129370382410798, 30.38064075563917044, 3.769987657317164231 ) ) ;
#12903 = CARTESIAN_POINT ( 'NONE',  ( -1.641525177248355227, -30.19571155489859393, 7.695279973900954751 ) ) ;
#12904 = CARTESIAN_POINT ( 'NONE',  ( 3.428517765372728121, -26.52631247858627006, 7.651421919295140484 ) ) ;
#12905 = CARTESIAN_POINT ( 'NONE',  ( 0.5834512725888432172, -26.35863018636138122, 6.894806418505347700 ) ) ;
#12906 = CARTESIAN_POINT ( 'NONE',  ( 23.14060042872244694, 4.027402677322106328, -3.115282196985579954 ) ) ;
#12907 = ORIENTED_EDGE ( 'NONE', *, *, #31991, .F. ) ;
#12908 = CARTESIAN_POINT ( 'NONE',  ( -65.04873975080087689, 34.92043383559632019, -6.752938550805224871 ) ) ;
#12909 = EDGE_LOOP ( 'NONE', ( #5077, #5699, #5802, #33984, #7210 ) ) ;
#12910 = ADVANCED_FACE ( 'NONE', ( #4768 ), #1905, .F. ) ;
#12911 = CARTESIAN_POINT ( 'NONE',  ( -1.113355428119774393, -31.66294493508353014, 7.387053503561886281 ) ) ;
#12912 = CARTESIAN_POINT ( 'NONE',  ( 4.291939159219374744, -27.36903995105183185, 7.643333865083957512 ) ) ;
#12913 = CARTESIAN_POINT ( 'NONE',  ( -80.68970021994135777, -6.620776169903922259, -2.209499440123503522 ) ) ;
#12914 = CARTESIAN_POINT ( 'NONE',  ( 0.9232239867627912711, -33.77039094905028804, 7.695279973900954751 ) ) ;
#12915 = FACE_OUTER_BOUND ( 'NONE', #7866, .T. ) ;
#12916 = CARTESIAN_POINT ( 'NONE',  ( 78.79418933159148253, 66.09338072887962312, 1.439474762807422703 ) ) ;
#12917 = CARTESIAN_POINT ( 'NONE',  ( 86.53727031679849802, -0.6854317443871157378, -5.678301933988063155 ) ) ;
#12918 = DIRECTION ( 'NONE',  ( 0.000000000000000000, 0.000000000000000000, 1.000000000000000000 ) ) ;
#12919 = EDGE_LOOP ( 'NONE', ( #33317, #19019, #6185, #10256 ) ) ;
#12920 = CARTESIAN_POINT ( 'NONE',  ( -67.52519766902113929, 36.12526529565825939, 8.800414904976360475 ) ) ;
#12921 = LINE ( 'NONE', #25487, #34101 ) ;
#12922 = VECTOR ( 'NONE', #37189, 1000.000000000000000 ) ;
#12923 = B_SPLINE_CURVE_WITH_KNOTS ( 'NONE', 3,
 ( #2080, #30261, #10900, #8419, #39309, #8208, #4549, #36046, #27164, #23478, #4941, #32954, #17272, #23670, #1873, #33376, #36639, #23860, #1462, #14396, #17074, #17679, #13996, #20783, #11098, #26771, #7822, #26967, #17888, #39720, #2276 ),
 .UNSPECIFIED., .F., .F.,
 ( 4, 3, 3, 3, 3, 3, 3, 3, 3, 3, 4 ),
 ( 5.204170427930421283E-18, 3.077658087706037842E-05, 6.152638666999422099E-05, 9.267501192707186834E-05, 0.0001241882240135245381, 0.0001556618703051713265, 0.0001866161554452296491, 0.0002167966385861026736, 0.0002463805737537830189, 0.0002758761370306596458, 0.0002847094172290124217 ),
 .UNSPECIFIED. ) ;
#12924 = EDGE_CURVE ( 'NONE', #5805, #18940, #4972, .T. ) ;
#12925 = VECTOR ( 'NONE', #1195, 1000.000000000000000 ) ;
#12926 = CARTESIAN_POINT ( 'NONE',  ( -64.75098741874282382, 36.24760096809094989, 6.319851154869007281 ) ) ;
#12927 = ADVANCED_FACE ( 'NONE', ( #17499 ), #11326, .F. ) ;
#12928 = CARTESIAN_POINT ( 'NONE',  ( 33.13586453634747642, -3.753881462307791850, -5.125994689951091310 ) ) ;
#12929 = DIRECTION ( 'NONE',  ( -0.000000000000000000, -0.000000000000000000, -1.000000000000000000 ) ) ;
#12930 = FACE_OUTER_BOUND ( 'NONE', #5751, .T. ) ;
#12931 = B_SPLINE_CURVE_WITH_KNOTS ( 'NONE', 3,
 ( #15052, #2733, #28848, #13191 ),
 .UNSPECIFIED., .F., .F.,
 ( 4, 4 ),
 ( 9.697399036122160616E-19, 6.391136169992784355E-06 ),
 .UNSPECIFIED. ) ;
#12932 = CARTESIAN_POINT ( 'NONE',  ( 20.42279120405673609, 3.662518919516934535, 3.393868513101561124 ) ) ;
#12933 = EDGE_CURVE ( 'NONE', #1854, #25414, #33404, .T. ) ;
#12934 = CARTESIAN_POINT ( 'NONE',  ( 86.21492201224262431, 1.517032185505227559, -5.007191195300914721 ) ) ;
#12935 = VERTEX_POINT ( 'NONE', #2103 ) ;
#12937 = CARTESIAN_POINT ( 'NONE',  ( -62.92837670882107659, -49.49506129533733656, 6.000000000000000000 ) ) ;
#12936 = CARTESIAN_POINT ( 'NONE',  ( 80.34143827441936025, 64.27643806731579446, -3.602832836245127623 ) ) ;
#12938 = CARTESIAN_POINT ( 'NONE',  ( -1.161450586000340790, -31.41865484090261518, 7.139196562012271485 ) ) ;
#12939 = ORIENTED_EDGE ( 'NONE', *, *, #8395, .F. ) ;
#12940 = CARTESIAN_POINT ( 'NONE',  ( -1.653803645021777902, -29.01370129510289431, 7.712764235869101093 ) ) ;
#12941 = ORIENTED_EDGE ( 'NONE', *, *, #13147, .T. ) ;
#12942 = CARTESIAN_POINT ( 'NONE',  ( -80.29545004356899085, -6.646483628119856490, 3.526391997555196056 ) ) ;
#12943 = AXIS2_PLACEMENT_3D ( 'NONE', #37766, #40440, #3239 ) ;
#12945 = ORIENTED_EDGE ( 'NONE', *, *, #26812, .T. ) ;
#12944 = ORIENTED_EDGE ( 'NONE', *, *, #31401, .T. ) ;
#12946 = CARTESIAN_POINT ( 'NONE',  ( 79.41630106684689849, 65.17102571570140412, -3.206617288017370448 ) ) ;
#12947 = AXIS2_PLACEMENT_3D ( 'NONE', #32008, #38353, #12439 ) ;
#12948 = CARTESIAN_POINT ( 'NONE',  ( 5.153279172109078488, -30.14225614731512337, 7.695279973900954751 ) ) ;
#12949 = VECTOR ( 'NONE', #31409, 1000.000000000000114 ) ;
#12950 = CARTESIAN_POINT ( 'NONE',  ( 24.86342019672374448, 1.896585702110065164, 4.289962101907669023 ) ) ;
#12951 = ORIENTED_EDGE ( 'NONE', *, *, #32559, .F. ) ;
#12952 = AXIS2_PLACEMENT_3D ( 'NONE', #25326, #40534, #40335 ) ;
#12953 = CARTESIAN_POINT ( 'NONE',  ( 81.31254497084465527, 65.18305021144011846, -2.731810022748015321 ) ) ;
#12954 = CARTESIAN_POINT ( 'NONE',  ( -3.078675913592197944, -26.64985754041175525, 6.800000000000000711 ) ) ;
#12956 = CARTESIAN_POINT ( 'NONE',  ( 86.24677872985614613, 1.481249208270744466, 4.702149241800761992 ) ) ;
#12955 = CARTESIAN_POINT ( 'NONE',  ( 4.543174969189649026, -31.43502378668323161, 6.903372536218457256 ) ) ;
#12957 = CARTESIAN_POINT ( 'NONE',  ( -32.24874870218063450, -25.49307895267003587, 6.700000000000000178 ) ) ;
#12958 = CARTESIAN_POINT ( 'NONE',  ( -64.08758708074093136, 41.04287353446839148, -3.000000000000000000 ) ) ;
#12959 = CARTESIAN_POINT ( 'NONE',  ( 70.66749459857992122, 60.15980271599462981, 3.887826097256385172 ) ) ;
#12960 = CARTESIAN_POINT ( 'NONE',  ( 23.87989460547934684, 3.092228747732352456, -3.719817981150454145 ) ) ;
#12961 = ORIENTED_EDGE ( 'NONE', *, *, #31350, .T. ) ;
#12962 = B_SPLINE_CURVE_WITH_KNOTS ( 'NONE', 3,
 ( #39761, #24734, #11336, #2316 ),
 .UNSPECIFIED., .F., .F.,
 ( 4, 4 ),
 ( 8.673617379884035472E-19, 6.391136169996031032E-06 ),
 .UNSPECIFIED. ) ;
#12963 = ORIENTED_EDGE ( 'NONE', *, *, #25818, .T. ) ;
#12964 = CARTESIAN_POINT ( 'NONE',  ( 21.85643539959776760, -12.33099359671888884, 6.023794913588264244 ) ) ;
#12965 = CARTESIAN_POINT ( 'NONE',  ( 16.12938719712982660, 15.26369590459581360, 1.887449634883829663 ) ) ;
#12966 = ORIENTED_EDGE ( 'NONE', *, *, #19481, .T. ) ;
#12967 = CARTESIAN_POINT ( 'NONE',  ( -55.02847197064691898, 31.32671726583495442, -1.333002506602602999 ) ) ;
#12968 = CARTESIAN_POINT ( 'NONE',  ( 81.68688842593508070, 61.98347795596147591, 2.134710458528625843 ) ) ;
#12969 = CARTESIAN_POINT ( 'NONE',  ( 86.60363381072151867, 0.9779648536402296699, 5.693185077828528229 ) ) ;
#12970 = ORIENTED_EDGE ( 'NONE', *, *, #32659, .T. ) ;
#12971 = CARTESIAN_POINT ( 'NONE',  ( 14.71640407924273219, 12.89631605138042403, 2.500000000000011546 ) ) ;
#12972 = CARTESIAN_POINT ( 'NONE',  ( 17.14784120125169409, -3.222914996324496517, 2.862138963676726711 ) ) ;
#12973 = CARTESIAN_POINT ( 'NONE',  ( 34.33288252766027426, -1.486090089270978298, -5.564874680979682964 ) ) ;
#12974 = CARTESIAN_POINT ( 'NONE',  ( 5.145066444271201966, -28.95006616558363888, 7.756742906098589074 ) ) ;
#12975 = CARTESIAN_POINT ( 'NONE',  ( -0.4513664592218429861, -26.80950562565463358, 7.750000000000000888 ) ) ;
#12976 = VECTOR ( 'NONE', #22482, 1000.000000000000114 ) ;
#12977 = CARTESIAN_POINT ( 'NONE',  ( 30.67406393699503298, -3.593393542108534344, -4.777508688867102116 ) ) ;
#12978 = ORIENTED_EDGE ( 'NONE', *, *, #4155, .T. ) ;
#12979 = VECTOR ( 'NONE', #10743, 1000.000000000000000 ) ;
#12980 = EDGE_CURVE ( 'NONE', #31466, #15576, #40353, .T. ) ;
#12981 = EDGE_CURVE ( 'NONE', #18407, #19773, #30794, .T. ) ;
#12982 = DIRECTION ( 'NONE',  ( 0.000000000000000000, 0.000000000000000000, 1.000000000000000000 ) ) ;
#12983 = EDGE_CURVE ( 'NONE', #30200, #27310, #28007, .T. ) ;
#12984 = CARTESIAN_POINT ( 'NONE',  ( 28.44546091714163438, -4.072879259825384679, 4.061366448452340627 ) ) ;
#12985 = ORIENTED_EDGE ( 'NONE', *, *, #1279, .T. ) ;
#12986 = ORIENTED_EDGE ( 'NONE', *, *, #3855, .T. ) ;
#12987 = CARTESIAN_POINT ( 'NONE',  ( 36.13125622736320253, -1.533072422867240325, 5.645132520243028473 ) ) ;
#12988 = DIRECTION ( 'NONE',  ( 1.000000000000000000, 0.000000000000000000, 0.000000000000000000 ) ) ;
#12989 = CARTESIAN_POINT ( 'NONE',  ( 66.71166677010936041, 57.90060579507158423, -3.999756211082797996 ) ) ;
#12990 = ORIENTED_EDGE ( 'NONE', *, *, #16842, .T. ) ;
#12991 = CARTESIAN_POINT ( 'NONE',  ( -77.46169046775075628, 11.07004784189294000, -7.581925507970804112 ) ) ;
#12992 = CARTESIAN_POINT ( 'NONE',  ( 4.932661409899757210, -28.51521593988763570, 6.864276522220859711 ) ) ;
#12993 = ORIENTED_EDGE ( 'NONE', *, *, #34334, .T. ) ;
#12994 = FACE_BOUND ( 'NONE', #28579, .T. ) ;
#12995 = CARTESIAN_POINT ( 'NONE',  ( 3.817924346030161509, -32.35669330361569962, 7.013842709614101167 ) ) ;
#12996 = VERTEX_POINT ( 'NONE', #40550 ) ;
#12997 = CARTESIAN_POINT ( 'NONE',  ( 81.94344439483582221, 61.95170768642834958, -1.250177805244664375 ) ) ;
#12998 = CARTESIAN_POINT ( 'NONE',  ( 78.61848929481175219, 66.00753381999014380, 1.284346554836966581 ) ) ;
#12999 = VECTOR ( 'NONE', #24457, 1000.000000000000000 ) ;
#13000 = CARTESIAN_POINT ( 'NONE',  ( 2.970800673062078179, -26.41619320027978191, 7.761597726988848756 ) ) ;
#13001 = EDGE_LOOP ( 'NONE', ( #33023, #457, #9851, #28548 ) ) ;
#13002 = ORIENTED_EDGE ( 'NONE', *, *, #125, .F. ) ;
#13003 = CARTESIAN_POINT ( 'NONE',  ( 74.79578028543750179, 61.54621940999656715, -3.896954863271601788 ) ) ;
#13005 = CARTESIAN_POINT ( 'NONE',  ( 3.811648262644349985E-18, -0.6000000000000000888, 3.780227049350623147 ) ) ;
#13004 = CARTESIAN_POINT ( 'NONE',  ( -1.660455515657601300, -29.01040133911542540, 7.257242401810563237 ) ) ;
#13006 = CARTESIAN_POINT ( 'NONE',  ( 14.89600225145155576, 12.34220076978314751, -2.524950096939041266 ) ) ;
#13007 = PRODUCT_DEFINITION_FORMATION_WITH_SPECIFIED_SOURCE ( 'ANY', '', #15521, .NOT_KNOWN. ) ;
#13008 = CARTESIAN_POINT ( 'NONE',  ( 78.67891909395969208, 66.05044883183083471, -1.113695828830620016 ) ) ;
#13009 = CARTESIAN_POINT ( 'NONE',  ( 78.14662766244083514, 60.27555255246360133, 2.661196496289686575 ) ) ;
#13010 = VECTOR ( 'NONE', #24122, 1000.000000000000000 ) ;
#13011 = VERTEX_POINT ( 'NONE', #31518 ) ;
#13012 = ORIENTED_EDGE ( 'NONE', *, *, #35537, .T. ) ;
#13013 = DIRECTION ( 'NONE',  ( 1.000000000000000000, 0.000000000000000000, 0.000000000000000000 ) ) ;
#13014 = CARTESIAN_POINT ( 'NONE',  ( -58.94604240597273304, 28.88056450265317210, 6.383919085388007453 ) ) ;
#13015 = CARTESIAN_POINT ( 'NONE',  ( 78.68944183191024422, 66.05792399308623430, 1.032522165606396092 ) ) ;
#13016 = CARTESIAN_POINT ( 'NONE',  ( -0.9575113486053222767, -31.84711263666175540, 7.695279973900954751 ) ) ;
#13017 = CARTESIAN_POINT ( 'NONE',  ( 26.62075075102985267, 2.678422205045695392, 2.704210781993271695 ) ) ;
#13018 = CARTESIAN_POINT ( 'NONE',  ( 2.259077079022228318, -26.21614592499068408, 7.721096864323904185 ) ) ;
#13019 = CARTESIAN_POINT ( 'NONE',  ( 3.576488244632886726, -26.73439304370792513, 6.979335674598003081 ) ) ;
#13020 = CARTESIAN_POINT ( 'NONE',  ( 4.702397412420262768, -31.34397018411862845, 7.783750581861601958 ) ) ;
#13021 = CARTESIAN_POINT ( 'NONE',  ( -0.5945065188923343014, -32.07860504069461172, 6.868387053540520704 ) ) ;
#13022 = CARTESIAN_POINT ( 'NONE',  ( 67.10243339269433704, 57.83959038316312729, 3.993403965430729841 ) ) ;
#13023 = LINE ( 'NONE', #18577, #5825 ) ;
#13024 = CARTESIAN_POINT ( 'NONE',  ( 27.58412137558927313, 1.448149839084869051, -4.473612028233096005 ) ) ;
#13025 = PLANE ( 'NONE',  #27272 ) ;
#13026 = CARTESIAN_POINT ( 'NONE',  ( -0.8809027425463855643, -31.78283038357269419, 7.695279973900954751 ) ) ;
#13027 = VECTOR ( 'NONE', #31049, 1000.000000000000000 ) ;
#13028 = CARTESIAN_POINT ( 'NONE',  ( 1.729779804934170606, -32.96980315820380270, 7.661510568013096822 ) ) ;
#13029 = CARTESIAN_POINT ( 'NONE',  ( 2.105750943142600029, -32.94567937155306225, 7.013842709614101167 ) ) ;
#13030 = CARTESIAN_POINT ( 'NONE',  ( 21.88434783170197662, -13.24225184460187776, -2.500000000000000000 ) ) ;
#13031 = AXIS2_PLACEMENT_3D ( 'NONE', #28983, #40710, #34981 ) ;
#13032 = CARTESIAN_POINT ( 'NONE',  ( -1.480676134522186382, -28.36955016868974511, 7.784838882742138644 ) ) ;
#13033 = EDGE_CURVE ( 'NONE', #9668, #13794, #30537, .T. ) ;
#13034 = FACE_OUTER_BOUND ( 'NONE', #37630, .T. ) ;
#13035 = VERTEX_POINT ( 'NONE', #28204 ) ;
#13036 = CARTESIAN_POINT ( 'NONE',  ( -1.439000463346111536, -30.89361514057134173, 7.139196562012272373 ) ) ;
#13037 = CARTESIAN_POINT ( 'NONE',  ( 68.09143390058649459, 58.21448531840948704, -3.990965707299596321 ) ) ;
#13038 = AXIS2_PLACEMENT_3D ( 'NONE', #35722, #1349, #36122 ) ;
#13039 = ORIENTED_EDGE ( 'NONE', *, *, #29011, .T. ) ;
#13040 = DIRECTION ( 'NONE',  ( 0.000000000000000000, 1.000000000000000000, 0.000000000000000000 ) ) ;
#13041 = CARTESIAN_POINT ( 'NONE',  ( 30.19003827612802482, -2.952522945788203845, 4.918283640461378781 ) ) ;
#13042 = CARTESIAN_POINT ( 'NONE',  ( 22.22390872265649620, 3.654499484256482855, 4.238281575154772440 ) ) ;
#13043 = CARTESIAN_POINT ( 'NONE',  ( 1.700390093233090871, -29.56993018339339940, 7.750000000000000888 ) ) ;
#13044 = CARTESIAN_POINT ( 'NONE',  ( -1.629504578382812818, -30.64779913458552230, 7.750000000000000888 ) ) ;
#13045 = ORIENTED_EDGE ( 'NONE', *, *, #22748, .T. ) ;
#13046 = CARTESIAN_POINT ( 'NONE',  ( -10.97867591359219475, -26.64985754041175525, 6.700000000000000178 ) ) ;
#13047 = CARTESIAN_POINT ( 'NONE',  ( 79.10769140560611845, 65.82222301601623826, 2.432199249741004987 ) ) ;
#13048 = CLOSED_SHELL ( 'NONE', ( #10965, #38238, #7578, #10810, #37190, #7160, #5316, #23753, #37043, #1937, #40677, #75, #34038, #12576, #13260, #17682, #16627, #10858, #6368, #27931, #36312, #11331, #22300, #31120, #5295, #23411, #34758, #25075, #17919, #13683, #1587, #33726, #36806, #546, #37827, #4250, #34103, #35707, #18586, #3292, #37761, #36628, #18216, #14921, #28692, #38063, #36501, #18351, #35730, #29753, #26600, #8924, #14969, #10730, #1120, #24682, #684, #16623, #1145, #12277, #28889, #8381, #31584, #36765, #19768, #6722, #10685, #6897, #13367, #32657, #2106, #20398, #7024, #1878, #36803, #37272, #30659, #15380, #3793, #15883, #4645, #16051, #23170, #4114, #32253, #21000, #19845, #5169, #21205, #4929, #15421, #2299, #29252, #14450, #28176, #25310, #3343, #1770, #16825, #32093, #5399, #6889, #31809, #21439, #39762, #22350, #7854, #35586, #2822, #34559, #6005, #32246, #30412, #33107 ) ) ;
#13049 = CARTESIAN_POINT ( 'NONE',  ( -1.060034464505671403, -31.72168673584834053, 7.750000000000000888 ) ) ;
#13050 = ORIENTED_EDGE ( 'NONE', *, *, #36358, .T. ) ;
#13051 = CARTESIAN_POINT ( 'NONE',  ( 79.76387963405315418, 62.93107248426419176, -3.707164540951496168 ) ) ;
#13052 = AXIS2_PLACEMENT_3D ( 'NONE', #3430, #15942, #34919 ) ;
#13054 = CARTESIAN_POINT ( 'NONE',  ( -1.667391206268897141, -30.03700422179043272, 6.863904403958576594 ) ) ;
#13053 = CARTESIAN_POINT ( 'NONE',  ( 23.62521421733200810, 0.5032721505374657678, 5.478091647691247346 ) ) ;
#13055 = CARTESIAN_POINT ( 'NONE',  ( 81.16306007146947366, 61.30159356321330932, -1.077711394953977386 ) ) ;
#13056 = ADVANCED_FACE ( 'NONE', ( #30915 ), #434, .F. ) ;
#13057 = CARTESIAN_POINT ( 'NONE',  ( 80.39537321288027272, 61.58102678004054553, 2.797036776683078596 ) ) ;
#13058 = ORIENTED_EDGE ( 'NONE', *, *, #19487, .F. ) ;
#13059 = CARTESIAN_POINT ( 'NONE',  ( -17.69482985384422236, -39.37473357531881391, -6.000000000000000000 ) ) ;
#13060 = CARTESIAN_POINT ( 'NONE',  ( -1.585154604418644197, -30.77225614172792589, 7.762796336881262249 ) ) ;
#13062 = EDGE_LOOP ( 'NONE', ( #4154, #31398, #14602, #30656, #35550 ) ) ;
#13061 = CARTESIAN_POINT ( 'NONE',  ( -64.08758708074093136, 43.62395174008263865, 2.468800635787086417 ) ) ;
#13063 = CARTESIAN_POINT ( 'NONE',  ( 22.80949115205394406, -6.484386712482024251, -3.653976874014524867 ) ) ;
#13064 = CARTESIAN_POINT ( 'NONE',  ( 4.197725314243516692, -27.25233838877152692, 7.139196562012272373 ) ) ;
#13065 = ORIENTED_EDGE ( 'NONE', *, *, #452, .F. ) ;
#13066 = CARTESIAN_POINT ( 'NONE',  ( -73.23935992792370087, 4.942735534762467964, 9.788940037685113893 ) ) ;
#13067 = FACE_OUTER_BOUND ( 'NONE', #2748, .T. ) ;
#13068 = AXIS2_PLACEMENT_3D ( 'NONE', #32043, #19063, #31626 ) ;
#13069 = EDGE_CURVE ( 'NONE', #37904, #21810, #12364, .T. ) ;
#13070 = DIRECTION ( 'NONE',  ( 1.000000000000000000, 0.000000000000000000, 0.000000000000000000 ) ) ;
#13071 = ORIENTED_EDGE ( 'NONE', *, *, #28296, .T. ) ;
#13072 = CYLINDRICAL_SURFACE ( 'NONE', #5219, 0.1000000000000028644 ) ;
#13073 = CARTESIAN_POINT ( 'NONE',  ( 32.90368182600108327, -3.810879906198540112, -4.978789352745470964 ) ) ;
#13074 = CARTESIAN_POINT ( 'NONE',  ( 37.10982994964820847, -2.403900326362613971, -5.951681757502289116 ) ) ;
#13075 = CARTESIAN_POINT ( 'NONE',  ( -1.526829923184012339, -28.21528965334980654, 7.013842709614101167 ) ) ;
#13076 = CARTESIAN_POINT ( 'NONE',  ( 17.01637594748899218, 9.184973690624572029, 2.862215027849857929 ) ) ;
#13077 = DIRECTION ( 'NONE',  ( 0.7660444431189771253, 0.6427876096865405842, -0.000000000000000000 ) ) ;
#13078 = PLANE ( 'NONE',  #35195 ) ;
#13079 = DIRECTION ( 'NONE',  ( 1.000000000000000000, -0.000000000000000000, 0.000000000000000000 ) ) ;
#13080 = CARTESIAN_POINT ( 'NONE',  ( 1.738310589916949978, -26.07012892756137035, 6.887161170156906209 ) ) ;
#13081 = CARTESIAN_POINT ( 'NONE',  ( 25.66313521821469479, 1.726747700288609799, -4.270219735217844814 ) ) ;
#13082 = CARTESIAN_POINT ( 'NONE',  ( 35.68902945888083167, -1.289468566711789554, -5.530809620460434672 ) ) ;
#13083 = VECTOR ( 'NONE', #33164, 1000.000000000000000 ) ;
#13084 = DIRECTION ( 'NONE',  ( 0.6605219282605377940, 0.000000000000000000, -0.7508067542896645907 ) ) ;
#13085 = ADVANCED_FACE ( 'NONE', ( #644 ), #35029, .T. ) ;
#13086 = ORIENTED_EDGE ( 'NONE', *, *, #15951, .F. ) ;
#13087 = CARTESIAN_POINT ( 'NONE',  ( 66.83775678531991105, 58.01055738293738528, 3.998747512904051060 ) ) ;
#13088 = CARTESIAN_POINT ( 'NONE',  ( 2.272716057154847924, -26.11704110451741556, 7.701614758090453705 ) ) ;
#13089 = CARTESIAN_POINT ( 'NONE',  ( 85.94684271633954609, 0.9790069142357779031, 5.868308835085408681 ) ) ;
#13090 = DIRECTION ( 'NONE',  ( 0.6427876096865481337, -0.7660444431189707970, -0.000000000000000000 ) ) ;
#13091 = ORIENTED_EDGE ( 'NONE', *, *, #31861, .F. ) ;
#13092 = CARTESIAN_POINT ( 'NONE',  ( -76.84400769949562005, 9.411604022321832019, -9.587408972141622243 ) ) ;
#13093 =( NAMED_UNIT ( * ) PLANE_ANGLE_UNIT ( ) SI_UNIT ( $, .RADIAN. ) );
#13094 = CARTESIAN_POINT ( 'NONE',  ( -4.444218661349752963, -35.94265729135299381, 2.500000000000000000 ) ) ;
#13095 = CARTESIAN_POINT ( 'NONE',  ( 1.195000870879840749, -26.11132176225047985, 7.771081512783698741 ) ) ;
#13096 = VECTOR ( 'NONE', #38732, 1000.000000000000000 ) ;
#13097 = EDGE_CURVE ( 'NONE', #15366, #18497, #33232, .T. ) ;
#13098 = EDGE_LOOP ( 'NONE', ( #17647, #38272, #35398, #9823 ) ) ;
#13099 = CARTESIAN_POINT ( 'NONE',  ( 4.031469603769337162, -26.96264342876691700, 7.766640943994645774 ) ) ;
#13100 = UNCERTAINTY_MEASURE_WITH_UNIT (LENGTH_MEASURE( 1.000000000000000082E-05 ), #32951, 'distance_accuracy_value', 'NONE');
#13101 = EDGE_LOOP ( 'NONE', ( #22190, #38287, #27299, #27416 ) ) ;
#13102 = EDGE_LOOP ( 'NONE', ( #15968, #1081, #34348, #25716, #23085 ) ) ;
#13103 = CARTESIAN_POINT ( 'NONE',  ( 78.54140637431730454, 65.95282500403628489, -1.409197735201547674 ) ) ;
#13104 = DIRECTION ( 'NONE',  ( 1.000000000000000000, 0.000000000000000000, 0.000000000000000000 ) ) ;
#13105 = CARTESIAN_POINT ( 'NONE',  ( 78.89219914629886432, 65.63660985470716014, 2.576318598473995802 ) ) ;
#13108 = VERTEX_POINT ( 'NONE', #1046 ) ;
#13107 = ORIENTED_EDGE ( 'NONE', *, *, #4123, .T. ) ;
#13106 = DIRECTION ( 'NONE',  ( 0.000000000000000000, -0.000000000000000000, -1.000000000000000000 ) ) ;
#13109 = FACE_OUTER_BOUND ( 'NONE', #13001, .T. ) ;
#13110 = CARTESIAN_POINT ( 'NONE',  ( 1.025391769970868561, -33.00423873498635174, 6.869132338375688818 ) ) ;
#13111 = CARTESIAN_POINT ( 'NONE',  ( -22.87867591359218977, -26.64985754041175525, 6.700000000000000178 ) ) ;
#13112 = EDGE_CURVE ( 'NONE', #17239, #29803, #33889, .T. ) ;
#13113 = EDGE_CURVE ( 'NONE', #26273, #6408, #20155, .T. ) ;
#13114 = CARTESIAN_POINT ( 'NONE',  ( 21.85643539959778892, 11.01376456104441104, -6.033145431426138572 ) ) ;
#13115 = CARTESIAN_POINT ( 'NONE',  ( 21.72163592607151728, 6.243142354532070115, -3.223666675097538459 ) ) ;
#13116 = ORIENTED_EDGE ( 'NONE', *, *, #36358, .F. ) ;
#13117 = CARTESIAN_POINT ( 'NONE',  ( -1.361968219098981914, -25.54247520618363509, 6.894806418505347700 ) ) ;
#13118 = ADVANCED_FACE ( 'NONE', ( #26154 ), #840, .F. ) ;
#13119 = PLANE ( 'NONE',  #6288 ) ;
#13120 = CARTESIAN_POINT ( 'NONE',  ( -0.6411629333918610341, -32.17099039281331585, 7.754798119455333705 ) ) ;
#13121 = CARTESIAN_POINT ( 'NONE',  ( -79.87442750853132623, -5.634526803139693563, -4.486596260177802442 ) ) ;
#13122 = DIRECTION ( 'NONE',  ( -1.000000000000000000, 0.000000000000000000, 0.000000000000000000 ) ) ;
#13123 = CARTESIAN_POINT ( 'NONE',  ( -80.92837670882107659, 2.429809908903242555, -12.50000000000000000 ) ) ;
#13124 = CARTESIAN_POINT ( 'NONE',  ( 81.36347513509556961, 62.06248151587793416, 2.615128354545396494 ) ) ;
#13125 = CARTESIAN_POINT ( 'NONE',  ( 84.96089493372460311, 1.928984934743871449, -4.835719925821683418 ) ) ;
#13126 = CARTESIAN_POINT ( 'NONE',  ( 25.01091293497539780, 3.329590547006094248, -1.936828119410943350 ) ) ;
#13127 = CARTESIAN_POINT ( 'NONE',  ( 2.928305877310407368, -32.84746552919321516, 7.720710062488892689 ) ) ;
#13128 = DIRECTION ( 'NONE',  ( 1.000000000000000000, 0.000000000000000000, 0.000000000000000000 ) ) ;
#13129 = TOROIDAL_SURFACE ( 'NONE', #11104, 5.329987104167480894, 1.000000000000000000 ) ;
#13130 = LINE ( 'NONE', #26105, #18429 ) ;
#13131 = CARTESIAN_POINT ( 'NONE',  ( -71.92837670882107659, -20.78299143688747819, 9.949874371066202983 ) ) ;
#13132 = DIRECTION ( 'NONE',  ( -0.3420201433256725987, 0.9396926207859068736, -0.000000000000000000 ) ) ;
#13133 = DIRECTION ( 'NONE',  ( -0.000000000000000000, -0.000000000000000000, 1.000000000000000000 ) ) ;
#13134 = EDGE_CURVE ( 'NONE', #36097, #26946, #32146, .T. ) ;
#13135 = CARTESIAN_POINT ( 'NONE',  ( 69.17602579976487220, 58.86946863987066791, 3.990151341881416514 ) ) ;
#13136 = CARTESIAN_POINT ( 'NONE',  ( 34.93030302952856658, -1.707825049874648560, 5.658116598965852617 ) ) ;
#13137 = ADVANCED_FACE ( 'NONE', ( #23063 ), #1445, .F. ) ;
#13138 = CARTESIAN_POINT ( 'NONE',  ( 72.80781396401921768, 61.43345056764702150, -3.736020861133335647 ) ) ;
#13139 = CARTESIAN_POINT ( 'NONE',  ( 88.07575545775937087, -0.5731442609823791390, 3.387043347726935050 ) ) ;
#13140 = CIRCLE ( 'NONE', #40078, 8.080217238368769372 ) ;
#13141 = ORIENTED_EDGE ( 'NONE', *, *, #6339, .F. ) ;
#13143 = LINE ( 'NONE', #16023, #13226 ) ;
#13142 = CARTESIAN_POINT ( 'NONE',  ( 80.21507364257669792, 64.59331366548809683, -3.526329879082137797 ) ) ;
#13144 = CARTESIAN_POINT ( 'NONE',  ( -70.26248529839136836, -48.46472069417173145, 9.978220256720669923 ) ) ;
#13145 = ORIENTED_EDGE ( 'NONE', *, *, #34676, .T. ) ;
#13146 = CARTESIAN_POINT ( 'NONE',  ( -1.624655799086301533, -28.85995144147929992, 7.754798119455333705 ) ) ;
#13147 = EDGE_CURVE ( 'NONE', #8480, #26273, #25743, .T. ) ;
#13148 = VERTEX_POINT ( 'NONE', #1251 ) ;
#13149 = CARTESIAN_POINT ( 'NONE',  ( -73.93807322288319028, -3.714211979007700393, 9.537397809311197960 ) ) ;
#13150 = VERTEX_POINT ( 'NONE', #19362 ) ;
#13151 = CARTESIAN_POINT ( 'NONE',  ( 80.96353394671048420, 62.18107606247197339, -2.978180346930979994 ) ) ;
#13152 = CARTESIAN_POINT ( 'NONE',  ( 3.300000000000000711, 0.000000000000000000, 0.000000000000000000 ) ) ;
#13153 = CARTESIAN_POINT ( 'NONE',  ( 23.39816613655191802, 1.771640793782062406, 4.881439243339824152 ) ) ;
#13155 = ORIENTED_EDGE ( 'NONE', *, *, #6289, .T. ) ;
#13154 = ORIENTED_EDGE ( 'NONE', *, *, #13641, .F. ) ;
#13156 = EDGE_CURVE ( 'NONE', #29262, #14158, #15273, .T. ) ;
#13157 = AXIS2_PLACEMENT_3D ( 'NONE', #26543, #20153, #11676 ) ;
#13158 = EDGE_CURVE ( 'NONE', #15576, #38704, #1335, .T. ) ;
#13159 = DIRECTION ( 'NONE',  ( 0.000000000000000000, 0.000000000000000000, 1.000000000000000000 ) ) ;
#13161 = CARTESIAN_POINT ( 'NONE',  ( 86.43327874156520352, 1.271763543294590848, 4.874929521669852051 ) ) ;
#13160 = CARTESIAN_POINT ( 'NONE',  ( 4.535927232918584018, -31.44602833479315862, 6.979335674598002193 ) ) ;
#13162 = CARTESIAN_POINT ( 'NONE',  ( -14.44874870218064089, -25.49307895267003587, 6.700000000000000178 ) ) ;
#13163 = CARTESIAN_POINT ( 'NONE',  ( -63.68223573671823345, 44.25617700581931047, -1.889122668681848527 ) ) ;
#13164 = CARTESIAN_POINT ( 'NONE',  ( 72.12755885004493450, 59.87634726091143023, 3.962431611477345239 ) ) ;
#13165 = ORIENTED_EDGE ( 'NONE', *, *, #21960, .T. ) ;
#13166 = CARTESIAN_POINT ( 'NONE',  ( 21.85074289711433337, 4.166209864296642529, -4.242968198356735776 ) ) ;
#13167 = EDGE_LOOP ( 'NONE', ( #40492, #28289, #6618, #672 ) ) ;
#13168 = ADVANCED_FACE ( 'NONE', ( #35233 ), #9886, .F. ) ;
#13169 = ORIENTED_EDGE ( 'NONE', *, *, #35846, .F. ) ;
#13170 = CARTESIAN_POINT ( 'NONE',  ( 21.85643539959774273, -6.858222381794880640, 10.60035608423801357 ) ) ;
#13171 = CARTESIAN_POINT ( 'NONE',  ( 21.85643539959777826, 3.765123657700753412, -3.918568846603332378 ) ) ;
#13172 = CARTESIAN_POINT ( 'NONE',  ( 1.700390093233090871, -29.56993018339339940, 6.800000000000000711 ) ) ;
#13173 = CARTESIAN_POINT ( 'NONE',  ( 81.59312859629706338, 63.05267747589692107, 3.015199126130972740 ) ) ;
#13174 = CARTESIAN_POINT ( 'NONE',  ( 85.38594790374143884, 2.393190016811436394, 3.957880923259903927 ) ) ;
#13175 = VERTEX_POINT ( 'NONE', #16856 ) ;
#13176 = CARTESIAN_POINT ( 'NONE',  ( 0.4715827230650022073, -32.74012475684295964, 7.784476445165072533 ) ) ;
#13177 = CARTESIAN_POINT ( 'NONE',  ( 16.21041041637272428, -3.304833269244274341, 2.736424614369139530 ) ) ;
#13178 = CARTESIAN_POINT ( 'NONE',  ( 5.076139281392760161, -29.16456933348392511, 7.013842709614101167 ) ) ;
#13179 = CARTESIAN_POINT ( 'NONE',  ( 34.92983894306404125, -1.709246109001034020, -5.658044167049093964 ) ) ;
#13180 = CARTESIAN_POINT ( 'NONE',  ( 5.158998514376012423, -29.06454096104016571, 7.771081512783696077 ) ) ;
#13181 = CARTESIAN_POINT ( 'NONE',  ( -1.766085975226569404, -30.05319374170961666, 7.750000000000000888 ) ) ;
#13182 = DIRECTION ( 'NONE',  ( 1.000000000000000000, 1.301859416973403519E-15, 0.000000000000000000 ) ) ;
#13183 = VECTOR ( 'NONE', #37616, 1000.000000000000000 ) ;
#13184 = DIRECTION ( 'NONE',  ( 1.000000000000000000, 0.000000000000000000, 0.000000000000000000 ) ) ;
#13185 = CARTESIAN_POINT ( 'NONE',  ( 28.20895372393743017, -3.294009627498124093, 4.609087483380881700 ) ) ;
#13186 = VERTEX_POINT ( 'NONE', #13788 ) ;
#13187 = ORIENTED_EDGE ( 'NONE', *, *, #29714, .T. ) ;
#13188 = CARTESIAN_POINT ( 'NONE',  ( 32.06717985418615768, 0.2495969218020720470, 4.732404502101774213 ) ) ;
#13189 = CARTESIAN_POINT ( 'NONE',  ( -1.477562859369297987, -28.36137111117319520, 6.894806418505348589 ) ) ;
#13190 = CARTESIAN_POINT ( 'NONE',  ( 66.42297474478729669, 57.78816748095987776, -4.000000000000015987 ) ) ;
#13191 = CARTESIAN_POINT ( 'NONE',  ( -0.4513664592218429861, -26.80950562565463358, 7.750000000000000888 ) ) ;
#13192 = ADVANCED_FACE ( 'NONE', ( #26355 ), #10680, .F. ) ;
#13193 = ORIENTED_EDGE ( 'NONE', *, *, #5823, .F. ) ;
#13194 = AXIS2_PLACEMENT_3D ( 'NONE', #26053, #10780, #38981 ) ;
#13195 = FACE_BOUND ( 'NONE', #19852, .T. ) ;
#13196 = ORIENTED_EDGE ( 'NONE', *, *, #6084, .F. ) ;
#13197 = FACE_BOUND ( 'NONE', #17887, .T. ) ;
#13198 = CARTESIAN_POINT ( 'NONE',  ( 3.812057553938478893, -32.36114986992183873, 6.903112506833892326 ) ) ;
#13199 = ORIENTED_EDGE ( 'NONE', *, *, #30745, .F. ) ;
#13200 = CARTESIAN_POINT ( 'NONE',  ( 82.44602376881505279, 63.15227202030949627, -1.728104186158371913 ) ) ;
#13201 = CARTESIAN_POINT ( 'NONE',  ( -64.15669616364041872, -60.53509472482660669, -1.328953532546369276 ) ) ;
#13202 = ORIENTED_EDGE ( 'NONE', *, *, #16229, .T. ) ;
#13203 = ORIENTED_EDGE ( 'NONE', *, *, #10230, .T. ) ;
#13204 = CARTESIAN_POINT ( 'NONE',  ( 75.00613679496295561, 61.08591394029932076, -3.912919437578906035 ) ) ;
#13206 = CARTESIAN_POINT ( 'NONE',  ( 4.373635312142695852, -27.31077402155920097, 7.756742906098587298 ) ) ;
#13205 = LINE ( 'NONE', #25773, #12773 ) ;
#13207 = CARTESIAN_POINT ( 'NONE',  ( 15.57425752064463076, 11.08950951739397262, -2.625789524671749753 ) ) ;
#13208 = CARTESIAN_POINT ( 'NONE',  ( 75.81058488580242738, 63.71552251304081693, 3.121245466998407103 ) ) ;
#13209 = ORIENTED_EDGE ( 'NONE', *, *, #25349, .F. ) ;
#13210 = CARTESIAN_POINT ( 'NONE',  ( -2.448748702180640446, -26.64985754041175525, 6.700000000000000178 ) ) ;
#13211 = AXIS2_PLACEMENT_3D ( 'NONE', #1495, #7858, #7254 ) ;
#13212 = EDGE_CURVE ( 'NONE', #1735, #11061, #33348, .T. ) ;
#13213 = CARTESIAN_POINT ( 'NONE',  ( 1.775729607206522065, -26.08305913168524626, 7.782861076432730840 ) ) ;
#13214 = ADVANCED_FACE ( 'NONE', ( #5327 ), #2470, .F. ) ;
#13215 = CARTESIAN_POINT ( 'NONE',  ( 22.81629046404031413, 3.691080719936705279, -3.767431959620346937 ) ) ;
#13216 = CARTESIAN_POINT ( 'NONE',  ( 82.12703758395463183, 64.04502942998723825, 2.474249079298665333 ) ) ;
#13217 =( BOUNDED_CURVE ( )  B_SPLINE_CURVE ( 3, ( #22043, #18945, #16052, #34621 ),
 .UNSPECIFIED., .F., .F. ) 
 B_SPLINE_CURVE_WITH_KNOTS ( ( 4, 4 ),
 ( 4.748221474220559735, 4.941946782021394924 ),
 .UNSPECIFIED. ) 
 CURVE ( )  GEOMETRIC_REPRESENTATION_ITEM ( )  RATIONAL_B_SPLINE_CURVE ( ( 1.000000000000000000, 0.9968749865767494445, 0.9968749865767494445, 1.000000000000000000 ) ) 
 REPRESENTATION_ITEM ( '' )  );
#13219 = CARTESIAN_POINT ( 'NONE',  ( 14.51114108199450925, 10.82491523625665053, 2.499999999996797229 ) ) ;
#13218 = CARTESIAN_POINT ( 'NONE',  ( -0.1573688963480438519, -32.53621386746299038, 6.867199677474203234 ) ) ;
#13220 = CARTESIAN_POINT ( 'NONE',  ( 28.43092716748534343, -1.248584762127236569, 6.041969456467763955 ) ) ;
#13221 = CARTESIAN_POINT ( 'NONE',  ( 2.272301947206582184, -26.21837579307170785, 7.748216051605119503 ) ) ;
#13222 = CARTESIAN_POINT ( 'NONE',  ( -70.79780587197991792, -21.78299143688773043, 10.00000000000003020 ) ) ;
#13223 = CARTESIAN_POINT ( 'NONE',  ( 3.204051609024970659, -33.64229020702606476, 7.013842709614101167 ) ) ;
#13224 = DIRECTION ( 'NONE',  ( 0.000000000000000000, 1.000000000000000000, 0.000000000000000000 ) ) ;
#13225 = DIRECTION ( 'NONE',  ( 1.000000000000000000, 0.000000000000000000, 0.000000000000000000 ) ) ;
#13226 = VECTOR ( 'NONE', #37229, 1000.000000000000000 ) ;
#13227 = CARTESIAN_POINT ( 'NONE',  ( 36.66469078098081980, -3.237339655608454603, -5.925250000093051028 ) ) ;
#13228 = CARTESIAN_POINT ( 'NONE',  ( -22.44874870218064089, -26.64985754041175525, 6.700000000000000178 ) ) ;
#13229 = DIRECTION ( 'NONE',  ( -0.000000000000000000, -0.000000000000000000, -1.000000000000000000 ) ) ;
#13230 = DIRECTION ( 'NONE',  ( 0.000000000000000000, 0.000000000000000000, 1.000000000000000000 ) ) ;
#13231 = CARTESIAN_POINT ( 'NONE',  ( -81.32912492467333720, 10.50070982703512712, 3.457416654607596840 ) ) ;
#13232 = CARTESIAN_POINT ( 'NONE',  ( 22.07803051241986836, -11.23212333282388009, -2.500000000000000444 ) ) ;
#13233 = CARTESIAN_POINT ( 'NONE',  ( -1.498939527478906575, -28.41913694277257108, 7.756377446753163873 ) ) ;
#13234 = CARTESIAN_POINT ( 'NONE',  ( 31.76537530306199741, -2.962049296186602731, 5.164153083184395143 ) ) ;
#13235 = ORIENTED_EDGE ( 'NONE', *, *, #18894, .T. ) ;
#13236 = FACE_OUTER_BOUND ( 'NONE', #20851, .T. ) ;
#13237 = CARTESIAN_POINT ( 'NONE',  ( 67.91151009994659660, 58.69545974841741298, -3.974537232972598755 ) ) ;
#13238 = ORIENTED_EDGE ( 'NONE', *, *, #4021, .F. ) ;
#13239 = FACE_OUTER_BOUND ( 'NONE', #5462, .T. ) ;
#13240 = CARTESIAN_POINT ( 'NONE',  ( -62.92837670882106238, -23.80776546975053520, 6.000000000000000000 ) ) ;
#13241 = CARTESIAN_POINT ( 'NONE',  ( 22.20338448559262901, 4.015215451811328329, 3.998823550933331195 ) ) ;
#13242 = CARTESIAN_POINT ( 'NONE',  ( 0.9485833586031139353, -32.88577924541437625, 6.876076431790004051 ) ) ;
#13243 = CARTESIAN_POINT ( 'NONE',  ( 1.112807738419320458, -26.22108755103345246, 7.769368695748488207 ) ) ;
#13244 = LINE ( 'NONE', #1122, #12002 ) ;
#13245 = VERTEX_POINT ( 'NONE', #7993 ) ;
#13246 = CARTESIAN_POINT ( 'NONE',  ( 1.300000000000000044, 0.000000000000000000, 0.000000000000000000 ) ) ;
#13247 = CARTESIAN_POINT ( 'NONE',  ( 21.29078198983360792, -3.051855081372369938, 3.444149166357055591 ) ) ;
#13248 = CARTESIAN_POINT ( 'NONE',  ( 81.13780861853922488, 61.29235415973830925, 1.171933751919296274 ) ) ;
#13249 = VECTOR ( 'NONE', #18336, 1000.000000000000000 ) ;
#13250 = CARTESIAN_POINT ( 'NONE',  ( -28.97867591359219475, -26.64985754041175525, 6.700000000000000178 ) ) ;
#13251 = ORIENTED_EDGE ( 'NONE', *, *, #32159, .T. ) ;
#13252 = CARTESIAN_POINT ( 'NONE',  ( 78.19518920554678232, 64.50268734400745529, -3.317372267376125450 ) ) ;
#13254 = DIRECTION ( 'NONE',  ( -0.000000000000000000, -0.000000000000000000, 1.000000000000000000 ) ) ;
#13253 = CARTESIAN_POINT ( 'NONE',  ( 23.60046373739841030, 0.4362303430042576147, 5.514821429153919041 ) ) ;
#13255 = CARTESIAN_POINT ( 'NONE',  ( 79.35885969106151094, 66.15515411851717431, -1.832274617051104393 ) ) ;
#13256 = CARTESIAN_POINT ( 'NONE',  ( 80.71621671784500052, 61.21110637000719379, 1.935054690158737323 ) ) ;
#13257 = ORIENTED_EDGE ( 'NONE', *, *, #22577, .T. ) ;
#13258 = EDGE_CURVE ( 'NONE', #7577, #13694, #2054, .T. ) ;
#13259 = LINE ( 'NONE', #13868, #40495 ) ;
#13260 = ADVANCED_FACE ( 'NONE', ( #5124 ), #24256, .F. ) ;
#13261 = CARTESIAN_POINT ( 'NONE',  ( 79.67387220895498956, 66.32735109421597031, 1.189854999565118199 ) ) ;
#13262 = CARTESIAN_POINT ( 'NONE',  ( -64.08758708074307719, 42.81481910881112896, 3.292730723027928796 ) ) ;
#13263 = CARTESIAN_POINT ( 'NONE',  ( 25.28494853283190125, -3.333630280469910723, 5.108382079771137008 ) ) ;
#13264 = CYLINDRICAL_SURFACE ( 'NONE', #9495, 0.1000000000000028644 ) ;
#13265 = ORIENTED_EDGE ( 'NONE', *, *, #27974, .T. ) ;
#13266 = CARTESIAN_POINT ( 'NONE',  ( -77.73005492033482255, -4.997448663934537905, 8.952513429815514456 ) ) ;
#13267 = CARTESIAN_POINT ( 'NONE',  ( -1.543826794133986269, -28.25651525684694576, 7.751599049952173637 ) ) ;
#13268 = CARTESIAN_POINT ( 'NONE',  ( 21.66003001261448802, 6.756596355199507187, 2.827218952364252580 ) ) ;
#13269 = CARTESIAN_POINT ( 'NONE',  ( 35.36801745506461003, -3.791884530138194265, -5.511195673735667988 ) ) ;
#13270 = CARTESIAN_POINT ( 'NONE',  ( 3.367954892094448205, -32.64715822689380786, 6.863805608295729499 ) ) ;
#13271 = CARTESIAN_POINT ( 'NONE',  ( 21.38350792168483139, 5.477734254629577748, 3.543811591909045156 ) ) ;
#13272 = LINE ( 'NONE', #19666, #36389 ) ;
#13273 = DIRECTION ( 'NONE',  ( -0.000000000000000000, -0.000000000000000000, -1.000000000000000000 ) ) ;
#13274 = DIRECTION ( 'NONE',  ( 0.000000000000000000, 0.000000000000000000, 1.000000000000000000 ) ) ;
#13275 = CARTESIAN_POINT ( 'NONE',  ( -40.87867591359218977, -24.55319635012989110, 6.800000000000000711 ) ) ;
#13276 = CARTESIAN_POINT ( 'NONE',  ( 26.33495388482178257, 1.786803017097982504, -4.277245124679304844 ) ) ;
#13277 = CIRCLE ( 'NONE', #38893, 3.499999999999999556 ) ;
#13278 = CARTESIAN_POINT ( 'NONE',  ( 33.68488252487933465, -0.3869890349111386740, -5.069973516189887341 ) ) ;
#13279 = LINE ( 'NONE', #6912, #11718 ) ;
#13280 = ORIENTED_EDGE ( 'NONE', *, *, #9514, .F. ) ;
#13281 = CARTESIAN_POINT ( 'NONE',  ( 66.82203765260634043, 58.05418649187924274, 3.997265020314329842 ) ) ;
#13282 = AXIS2_PLACEMENT_3D ( 'NONE', #9944, #896, #35687 ) ;
#13283 = CARTESIAN_POINT ( 'NONE',  ( 86.57035376367728929, -0.007661497531101129840, -5.962853773335548446 ) ) ;
#13284 = VERTEX_POINT ( 'NONE', #1640 ) ;
#13285 = CARTESIAN_POINT ( 'NONE',  ( -73.12373367897625087, 4.565503759671822870, -10.93214365780120545 ) ) ;
#13286 = DIRECTION ( 'NONE',  ( 1.000000000000000000, 0.000000000000000000, 0.000000000000000000 ) ) ;
#13287 = CARTESIAN_POINT ( 'NONE',  ( 2.956026735610348233, -26.31784691181716340, 7.784725160561909441 ) ) ;
#13288 = DIRECTION ( 'NONE',  ( -5.570824187210003553E-14, 1.000000000000000000, -6.938893903907129770E-15 ) ) ;
#13289 = ORIENTED_EDGE ( 'NONE', *, *, #6520, .T. ) ;
#13290 = CARTESIAN_POINT ( 'NONE',  ( 3.948490735960236364, -26.89162167269672921, 7.767720160662274331 ) ) ;
#13291 = ORIENTED_EDGE ( 'NONE', *, *, #11319, .T. ) ;
#13292 = CARTESIAN_POINT ( 'NONE',  ( 80.75052706852349615, 61.66721672131044585, -2.660933152496147258 ) ) ;
#13293 = CARTESIAN_POINT ( 'NONE',  ( -1.720551146415195021, -28.88027794134619697, 7.780491323090172884 ) ) ;
#13294 = CARTESIAN_POINT ( 'NONE',  ( 79.52504771873113043, 64.52527500529804172, 3.543129918318852045 ) ) ;
#13296 = ORIENTED_EDGE ( 'NONE', *, *, #20671, .T. ) ;
#13295 = CARTESIAN_POINT ( 'NONE',  ( -1.699609906766908374, -29.55367944812416070, 6.931117832418181912 ) ) ;
#13297 = CARTESIAN_POINT ( 'NONE',  ( -88.78960668556791802, 4.298224710795182091, 12.50000000000000000 ) ) ;
#13298 = CARTESIAN_POINT ( 'NONE',  ( -1.797340250851707344, -29.44390463015740522, 7.750000000000000888 ) ) ;
#13299 = ADVANCED_FACE ( 'NONE', ( #39905 ), #39693, .F. ) ;
#13300 = CARTESIAN_POINT ( 'NONE',  ( 0.9127401033365564187, -32.98015121632014512, 6.916197352289366940 ) ) ;
#13301 = CARTESIAN_POINT ( 'NONE',  ( -63.96695182803195934, 19.27020452292900288, 9.800414904976365804 ) ) ;
#13302 = CARTESIAN_POINT ( 'NONE',  ( 21.85643539959776049, -14.86125632165375343, -4.251346793879176467 ) ) ;
#13303 = CARTESIAN_POINT ( 'NONE',  ( 22.00415366418653562, 5.540035186195420458, -3.131174203737818296 ) ) ;
#13304 = VERTEX_POINT ( 'NONE', #20972 ) ;
#13305 = CARTESIAN_POINT ( 'NONE',  ( 5.200304181073969190, -29.54472379604562704, 7.651421919295144036 ) ) ;
#13306 = ORIENTED_EDGE ( 'NONE', *, *, #22760, .F. ) ;
#13307 = CARTESIAN_POINT ( 'NONE',  ( -1.238405014327524922, -31.48339769696754331, 7.139344958878411695 ) ) ;
#13308 = DIRECTION ( 'NONE',  ( 0.7660444431189770143, 0.6427876096865404731, -0.000000000000000000 ) ) ;
#13309 = CARTESIAN_POINT ( 'NONE',  ( -74.10404772851687483, -1.915033150869918099, -10.75253851325693688 ) ) ;
#13310 = CARTESIAN_POINT ( 'NONE',  ( 5.144846875551112753, -28.94886861257825572, 7.635761828346576685 ) ) ;
#13311 = DIRECTION ( 'NONE',  ( 0.000000000000000000, 0.000000000000000000, 1.000000000000000000 ) ) ;
#13312 = CARTESIAN_POINT ( 'NONE',  ( 78.67710717883703353, 66.04916176178687692, 1.122020883098625355 ) ) ;
#13313 = CARTESIAN_POINT ( 'NONE',  ( 87.52985346608603834, -1.683278932971326691, -4.201117388013917875 ) ) ;
#13314 = CARTESIAN_POINT ( 'NONE',  ( -0.01902423455012235490, -32.61847323140942478, 7.710604733652635545 ) ) ;
#13315 = CARTESIAN_POINT ( 'NONE',  ( -1.270178459801816206, -27.72063930510053709, 7.761113333117549473 ) ) ;
#13316 = CARTESIAN_POINT ( 'NONE',  ( 21.55641518153495184, 7.313212361982168730, -1.964796485855104358 ) ) ;
#13317 = CARTESIAN_POINT ( 'NONE',  ( 1.664433243520564876, -26.17012032033359148, 7.703977250142848732 ) ) ;
#13318 = CARTESIAN_POINT ( 'NONE',  ( -0.3285218188496327740, -26.84164346155765557, 6.911401339314955372 ) ) ;
#13319 = CARTESIAN_POINT ( 'NONE',  ( 4.646307801825953376, -27.87241174337603766, 7.769368695748489095 ) ) ;
#13320 = CARTESIAN_POINT ( 'NONE',  ( 4.812521983982041895, -27.96848237138598137, 7.013842709614101167 ) ) ;
#13321 = CARTESIAN_POINT ( 'NONE',  ( 69.31827979293011310, 58.50063561948233115, 3.969490915146638876 ) ) ;
#13322 = CARTESIAN_POINT ( 'NONE',  ( 36.97985918926679005, -2.956901537102269106, 5.977999406396011572 ) ) ;
#13323 = EDGE_CURVE ( 'NONE', #34397, #24284, #39084, .T. ) ;
#13324 = CARTESIAN_POINT ( 'NONE',  ( -64.08758708074093136, 43.28737448368270435, -1.986914326131290931 ) ) ;
#13325 = B_SPLINE_CURVE_WITH_KNOTS ( 'NONE', 3,
 ( #35223, #39071, #16640, #20146, #29817, #32920, #10473, #1241, #1628, #35619, #6995, #13777, #19753, #10669, #19945, #7391, #19560, #16453, #29225, #26345, #23250, #29027, #830, #35816, #13361, #10274, #4522, #17042, #25936, #29621, #32331 ),
 .UNSPECIFIED., .F., .F.,
 ( 4, 3, 3, 3, 3, 3, 3, 3, 3, 3, 4 ),
 ( 0.000000000000000000, 2.999644130997832929E-05, 6.002588995695094977E-05, 8.960886084588270950E-05, 0.0001190604700446527250, 0.0001489538463052755965, 0.0001796139255493990746, 0.0002109707048517114154, 0.0002426195318110371997, 0.0002740640997890095992, 0.0002849778069099847449 ),
 .UNSPECIFIED. ) ;
#13326 = CARTESIAN_POINT ( 'NONE',  ( 87.26180097699096905, 0.3411280444268214862, 4.951700522085849876 ) ) ;
#13327 = EDGE_LOOP ( 'NONE', ( #12180, #13386, #11308, #27989 ) ) ;
#13329 = LINE ( 'NONE', #23218, #9270 ) ;
#13328 = CARTESIAN_POINT ( 'NONE',  ( 78.67160034737365493, 66.04525015085646089, -1.145133111591881026 ) ) ;
#13330 = CARTESIAN_POINT ( 'NONE',  ( -1.356998574253440948, -31.24811977623772918, 7.782861076432731728 ) ) ;
#13331 = EDGE_CURVE ( 'NONE', #36906, #5482, #10202, .T. ) ;
#13332 = DIRECTION ( 'NONE',  ( -0.3103887796125159859, -0.9506097019758703581, 0.000000000000000000 ) ) ;
#13333 = CIRCLE ( 'NONE', #29762, 3.499999999999999556 ) ;
#13334 = ORIENTED_EDGE ( 'NONE', *, *, #9670, .T. ) ;
#13335 = EDGE_CURVE ( 'NONE', #31580, #28300, #11480, .T. ) ;
#13336 = DIRECTION ( 'NONE',  ( -0.000000000000000000, -0.000000000000000000, 1.000000000000000000 ) ) ;
#13337 = ORIENTED_EDGE ( 'NONE', *, *, #33534, .F. ) ;
#13338 = LINE ( 'NONE', #10251, #34700 ) ;
#13339 = EDGE_CURVE ( 'NONE', #32211, #15032, #32932, .T. ) ;
#13341 = ORIENTED_EDGE ( 'NONE', *, *, #4988, .F. ) ;
#13340 = EDGE_LOOP ( 'NONE', ( #67, #9718, #5935, #8061, #40267 ) ) ;
#13342 = CARTESIAN_POINT ( 'NONE',  ( 80.88543547514458965, 62.41573260227067976, -3.197674131580382717 ) ) ;
#13343 = CARTESIAN_POINT ( 'NONE',  ( -70.92837670882107659, -27.85319909218681644, -6.138794830819693793 ) ) ;
#13344 = CARTESIAN_POINT ( 'NONE',  ( 25.13028398501089455, 2.418633085955766759, 4.024527564920112432 ) ) ;
#13346 = VERTEX_POINT ( 'NONE', #11679 ) ;
#13345 = VERTEX_POINT ( 'NONE', #36614 ) ;
#13347 = CARTESIAN_POINT ( 'NONE',  ( 80.51660522894103167, 65.82269567859330550, -2.502189764415934548 ) ) ;
#13348 = CARTESIAN_POINT ( 'NONE',  ( 5.076139281392760161, -29.16456933348392511, 7.013842709614101167 ) ) ;
#13349 = EDGE_CURVE ( 'NONE', #25264, #15683, #23348, .T. ) ;
#13351 = CARTESIAN_POINT ( 'NONE',  ( 85.36365109362724013, 2.473220085049208983, 2.424004168925880442 ) ) ;
#13350 = CARTESIAN_POINT ( 'NONE',  ( 4.540072660877648048, -31.43975234032491528, 6.911401339314955372 ) ) ;
#13352 = DIRECTION ( 'NONE',  ( -0.000000000000000000, -0.000000000000000000, 1.000000000000000000 ) ) ;
#13353 = CARTESIAN_POINT ( 'NONE',  ( -64.08758708073987975, 43.72986257717802516, -2.307254338139467897 ) ) ;
#13354 = CARTESIAN_POINT ( 'NONE',  ( 70.80012018114213390, 59.83342440824694819, 3.954977122261609690 ) ) ;
#13355 = CARTESIAN_POINT ( 'NONE',  ( 24.36792415750019458, 2.936288794802523139, -3.728798694104302758 ) ) ;
#13356 = VERTEX_POINT ( 'NONE', #14179 ) ;
#13357 = CARTESIAN_POINT ( 'NONE',  ( 5.025435985552490159, -30.27990892530747047, 7.754798119455333705 ) ) ;
#13358 = ORIENTED_EDGE ( 'NONE', *, *, #30, .T. ) ;
#13359 = CARTESIAN_POINT ( 'NONE',  ( 21.85643539959774273, 10.54266624894746229, 1.842303177338921572 ) ) ;
#13360 = CARTESIAN_POINT ( 'NONE',  ( 21.87484035784453695, 3.535422555123523658, 3.391095861108603504 ) ) ;
#13361 = CARTESIAN_POINT ( 'NONE',  ( 0.4594594901768997985, -32.73538295328250314, 6.870716933885664623 ) ) ;
#13362 = CARTESIAN_POINT ( 'NONE',  ( 81.04289631908092417, 64.65011820513348084, 3.243459512806144307 ) ) ;
#13363 = CARTESIAN_POINT ( 'NONE',  ( 87.94592890065770519, -0.6044765299818539717, 4.822713664802365408 ) ) ;
#13364 = VERTEX_POINT ( 'NONE', #20353 ) ;
#13365 = COLOUR_RGB ( '',0.7921568627450980005, 0.8196078431372548767, 0.9333333333333333481 ) ;
#13366 = DIRECTION ( 'NONE',  ( 0.000000000000000000, 1.000000000000000000, 0.000000000000000000 ) ) ;
#13367 = ADVANCED_FACE ( 'NONE', ( #30443 ), #2253, .F. ) ;
#13368 = CARTESIAN_POINT ( 'NONE',  ( 15.06368528933364281, -4.031268556551167670, 2.557450424642690567 ) ) ;
#13369 = CARTESIAN_POINT ( 'NONE',  ( 35.92872908462157966, -2.111607858196849818, 5.813945131888477391 ) ) ;
#13370 = CARTESIAN_POINT ( 'NONE',  ( 5.070928005489710344, -29.12330485715137840, 6.868387053540519815 ) ) ;
#13371 = CARTESIAN_POINT ( 'NONE',  ( 34.13611374073711602, -3.134507220645912806, -5.534164152908742196 ) ) ;
#13372 = DIRECTION ( 'NONE',  ( -0.3420201433256663259, -0.9396926207859092051, 0.000000000000000000 ) ) ;
#13373 = CARTESIAN_POINT ( 'NONE',  ( 84.50896143996750709, 2.514019815156651294, -3.493124578469008146 ) ) ;
#13374 = CARTESIAN_POINT ( 'NONE',  ( 2.895822981304927879, -32.85599670560755925, 7.767720160662274331 ) ) ;
#13375 = CARTESIAN_POINT ( 'NONE',  ( 5.651251297819362307, -26.64985754041175525, 6.700000000000000178 ) ) ;
#13376 = VECTOR ( 'NONE', #28065, 1000.000000000000000 ) ;
#13377 = VECTOR ( 'NONE', #8065, 1000.000000000000000 ) ;
#13378 = CARTESIAN_POINT ( 'NONE',  ( 32.89828394892415275, -3.753738769583905288, 5.047802179214622598 ) ) ;
#13379 = EDGE_LOOP ( 'NONE', ( #11149, #13464 ) ) ;
#13380 = ORIENTED_EDGE ( 'NONE', *, *, #16507, .T. ) ;
#13381 = CARTESIAN_POINT ( 'NONE',  ( 37.18642854612528481, -2.963312751682652735, 6.000018072115591572 ) ) ;
#13382 = CARTESIAN_POINT ( 'NONE',  ( 1.699828613893618945, -33.06668477344420154, 7.767720160662275219 ) ) ;
#13383 = EDGE_CURVE ( 'NONE', #12703, #3524, #29922, .T. ) ;
#13384 = CARTESIAN_POINT ( 'NONE',  ( 3.594851464545667952, -26.62696974998548782, 7.013842709614101167 ) ) ;
#13385 = CARTESIAN_POINT ( 'NONE',  ( 86.66947201173555015, -0.8835633689198520990, 5.500948792305413448 ) ) ;
#13386 = ORIENTED_EDGE ( 'NONE', *, *, #20725, .F. ) ;
#13387 = EDGE_CURVE ( 'NONE', #31945, #3169, #13500, .T. ) ;
#13388 = ORIENTED_EDGE ( 'NONE', *, *, #22748, .F. ) ;
#13389 = DIRECTION ( 'NONE',  ( -1.000000000000000000, -0.000000000000000000, -0.000000000000000000 ) ) ;
#13390 = CYLINDRICAL_SURFACE ( 'NONE', #32702, 0.1000000000000028644 ) ;
#13391 = CARTESIAN_POINT ( 'NONE',  ( 14.77315594796471743, 13.19392823276620419, 2.499999999999996891 ) ) ;
#13392 = ORIENTED_EDGE ( 'NONE', *, *, #40273, .F. ) ;
#13393 = FACE_BOUND ( 'NONE', #27930, .T. ) ;
#13394 = ADVANCED_FACE ( 'NONE', ( #4915 ), #17446, .T. ) ;
#13395 = CARTESIAN_POINT ( 'NONE',  ( 3.814825531500412481, -32.35904579807917258, 7.009310105710486738 ) ) ;
#13396 = VERTEX_POINT ( 'NONE', #39485 ) ;
#13397 = CARTESIAN_POINT ( 'NONE',  ( 24.27615491347996723, 3.119136480584640658, 3.486480195292287032 ) ) ;
#13398 = CARTESIAN_POINT ( 'NONE',  ( 82.29876416100408676, 62.79692783100093578, -1.831286414254867934 ) ) ;
#13399 = CARTESIAN_POINT ( 'NONE',  ( -1.312560436656867724, -31.35097737660188244, 7.697032948437508182 ) ) ;
#13400 = EDGE_LOOP ( 'NONE', ( #40708, #6282, #22830 ) ) ;
#13401 = CARTESIAN_POINT ( 'NONE',  ( 75.43741953989466253, 63.08613174173243010, -3.462570962765005866 ) ) ;
#13402 = EDGE_CURVE ( 'NONE', #15998, #5350, #16120, .T. ) ;
#13404 = CARTESIAN_POINT ( 'NONE',  ( -28.87867591359218977, -26.64985754041175525, 6.800000000000000711 ) ) ;
#13403 = FACE_BOUND ( 'NONE', #20034, .T. ) ;
#13405 = FACE_OUTER_BOUND ( 'NONE', #36198, .T. ) ;
#13406 = CARTESIAN_POINT ( 'NONE',  ( 76.63461511614542587, 62.03359853006617186, 3.872369636031695705 ) ) ;
#13407 = FACE_BOUND ( 'NONE', #1109, .T. ) ;
#13408 = CYLINDRICAL_SURFACE ( 'NONE', #39203, 0.09010775117052842453 ) ;
#13409 = CIRCLE ( 'NONE', #39047, 3.000000000000002665 ) ;
#13410 = CARTESIAN_POINT ( 'NONE',  ( 25.33160239074249986, 2.112310346557956908, -4.160007218831053954 ) ) ;
#13411 = CARTESIAN_POINT ( 'NONE',  ( 80.07729437284027085, 66.15382583937156369, 2.040045296073325520 ) ) ;
#13412 = DIRECTION ( 'NONE',  ( 1.000000000000000000, 0.000000000000000000, 0.000000000000000000 ) ) ;
#13413 = CARTESIAN_POINT ( 'NONE',  ( 27.88065694771982450, 2.580388505813413502, -1.055963728923108524 ) ) ;
#13414 = CARTESIAN_POINT ( 'NONE',  ( 3.559755418260376114, -26.72339534466646427, 7.013842709614101167 ) ) ;
#13415 = DIRECTION ( 'NONE',  ( -0.000000000000000000, -0.000000000000000000, -1.000000000000000000 ) ) ;
#13416 = VECTOR ( 'NONE', #31182, 1000.000000000000000 ) ;
#13417 = CARTESIAN_POINT ( 'NONE',  ( 1.700390093233090871, -29.56993018339339940, 7.800000000000000711 ) ) ;
#13418 = CARTESIAN_POINT ( 'NONE',  ( 0.7149948906900660539, -26.31585638355339185, 7.013842709614101167 ) ) ;
#13419 = CARTESIAN_POINT ( 'NONE',  ( 71.53106143128088945, 58.56707856135989942, 3.757617741137792677 ) ) ;
#13420 = CARTESIAN_POINT ( 'NONE',  ( 36.98988159880491366, -2.542881062934562841, -5.977438618132547177 ) ) ;
#13421 = AXIS2_PLACEMENT_3D ( 'NONE', #205, #18933, #18717 ) ;
#13422 = DIRECTION ( 'NONE',  ( 1.000000000000000000, 0.000000000000000000, 0.000000000000000000 ) ) ;
#13423 = LINE ( 'NONE', #4769, #14082 ) ;
#13424 = CARTESIAN_POINT ( 'NONE',  ( 3.322058374886247556, -32.55827286526241693, 7.778050822775631090 ) ) ;
#13425 = DIRECTION ( 'NONE',  ( 1.000000000000000000, 0.000000000000000000, 0.000000000000000000 ) ) ;
#13426 = EDGE_CURVE ( 'NONE', #1269, #10273, #14994, .T. ) ;
#13427 = CARTESIAN_POINT ( 'NONE',  ( 21.88286327911765028, -13.27756337371481798, -2.499999999999999556 ) ) ;
#13428 = CARTESIAN_POINT ( 'NONE',  ( 21.87963034546448071, -13.35931693332254788, 2.500000000000000444 ) ) ;
#13429 = EDGE_CURVE ( 'NONE', #30233, #31898, #5000, .T. ) ;
#13430 = ORIENTED_EDGE ( 'NONE', *, *, #12687, .T. ) ;
#13431 = CARTESIAN_POINT ( 'NONE',  ( 33.75536587385149545, -0.8752969169947810713, 5.454565398524055198 ) ) ;
#13432 = LINE ( 'NONE', #9747, #33698 ) ;
#13433 = CARTESIAN_POINT ( 'NONE',  ( 67.81915466200213416, 58.05084569011909679, -3.988165415173097195 ) ) ;
#13434 = ADVANCED_FACE ( 'NONE', ( #28161 ), #18905, .F. ) ;
#13435 = CARTESIAN_POINT ( 'NONE',  ( 11.65737507970504616, -30.94667987854474234, 6.000000000000000000 ) ) ;
#13436 = ORIENTED_EDGE ( 'NONE', *, *, #26415, .T. ) ;
#13437 = VECTOR ( 'NONE', #5624, 1000.000000000000000 ) ;
#13438 = CARTESIAN_POINT ( 'NONE',  ( -36.34874870218064302, -25.49307895267003587, 6.700000000000000178 ) ) ;
#13439 = ADVANCED_FACE ( 'NONE', ( #37019 ), #6147, .T. ) ;
#13440 = CARTESIAN_POINT ( 'NONE',  ( -64.08758708074093136, 37.43074634367857101, 3.182173495014448239 ) ) ;
#13441 = CARTESIAN_POINT ( 'NONE',  ( 24.35459986608915628, 2.895258409799770227, 3.776052705250971364 ) ) ;
#13442 = CARTESIAN_POINT ( 'NONE',  ( -70.92837670882107659, 28.72470171467712063, -4.357836081054403010 ) ) ;
#13443 = DIRECTION ( 'NONE',  ( -0.000000000000000000, -0.000000000000000000, -1.000000000000000000 ) ) ;
#13444 = CARTESIAN_POINT ( 'NONE',  ( 1.236065439282523437, -26.10086653224289321, 6.875780273367531947 ) ) ;
#13445 = ORIENTED_EDGE ( 'NONE', *, *, #16462, .T. ) ;
#13446 = CARTESIAN_POINT ( 'NONE',  ( 21.82997413388621410, 5.965416049814977306, 3.134756262805778793 ) ) ;
#13447 = PRESENTATION_STYLE_ASSIGNMENT (( #912 ) ) ;
#13448 = VECTOR ( 'NONE', #18531, 1000.000000000000000 ) ;
#13449 = CARTESIAN_POINT ( 'NONE',  ( 79.44789965344523353, 65.49939714349790165, 2.911438267503724475 ) ) ;
#13450 = DIRECTION ( 'NONE',  ( 0.000000000000000000, 0.000000000000000000, -1.000000000000000000 ) ) ;
#13451 = ORIENTED_EDGE ( 'NONE', *, *, #35088, .F. ) ;
#13452 = CARTESIAN_POINT ( 'NONE',  ( 78.28284693538141426, 65.31437991193503478, -2.608847861177645111 ) ) ;
#13453 =( BOUNDED_CURVE ( )  B_SPLINE_CURVE ( 3, ( #23367, #39199, #7117, #32850 ),
 .UNSPECIFIED., .F., .F. ) 
 B_SPLINE_CURVE_WITH_KNOTS ( ( 4, 4 ),
 ( 1.381924640371168467, 1.574767692156078258 ),
 .UNSPECIFIED. ) 
 CURVE ( )  GEOMETRIC_REPRESENTATION_ITEM ( )  RATIONAL_B_SPLINE_CURVE ( ( 1.000000000000000000, 0.9969033633783032089, 0.9969033633783032089, 1.000000000000000000 ) ) 
 REPRESENTATION_ITEM ( '' )  );
#13455 = CARTESIAN_POINT ( 'NONE',  ( -1.712075311290714108, -28.79206138794767611, 6.899963164400790383 ) ) ;
#13454 = CARTESIAN_POINT ( 'NONE',  ( 26.05429450752729892, 0.7955742409443752328, 4.421904258172623337 ) ) ;
#13456 = CARTESIAN_POINT ( 'NONE',  ( 79.08571093829934284, 66.16712123189802242, -1.622497907168747089 ) ) ;
#13457 = CARTESIAN_POINT ( 'NONE',  ( 79.08256350411643609, 63.89089281391859032, 3.718817779187653549 ) ) ;
#13458 = FACE_OUTER_BOUND ( 'NONE', #37891, .T. ) ;
#13459 = CARTESIAN_POINT ( 'NONE',  ( 80.02802368947529033, 66.35789156557528656, 1.168532795813725045 ) ) ;
#13460 = CARTESIAN_POINT ( 'NONE',  ( -64.08758708074093136, 41.64119180492454575, 2.960472591334007753 ) ) ;
#13461 = B_SPLINE_CURVE_WITH_KNOTS ( 'NONE', 3,
 ( #2196, #37167, #36760, #8546, #36557, #33498, #21738, #8745, #14714, #8336 ),
 .UNSPECIFIED., .F., .F.,
 ( 4, 3, 3, 4 ),
 ( 8.673617379884035472E-19, 3.025570593003197716E-05, 6.051145698344131290E-05, 6.468151674593491419E-05 ),
 .UNSPECIFIED. ) ;
#13462 = CARTESIAN_POINT ( 'NONE',  ( 25.43482567069144906, -3.911874351919522041, 4.043259094187231284 ) ) ;
#13463 = CARTESIAN_POINT ( 'NONE',  ( -64.17943696418035415, 35.01970154838168980, -4.761094547372056063 ) ) ;
#13464 = ORIENTED_EDGE ( 'NONE', *, *, #21751, .T. ) ;
#13465 = CARTESIAN_POINT ( 'NONE',  ( -79.86026552043743720, -5.632672876117126748, 4.514648094728398675 ) ) ;
#13466 = CARTESIAN_POINT ( 'NONE',  ( 23.58040427942380290, 0.3886573651980784194, -5.537642973953215808 ) ) ;
#13467 = CARTESIAN_POINT ( 'NONE',  ( -2.878675913592191993, -26.64985754041175525, 6.700000000000000178 ) ) ;
#13468 = AXIS2_PLACEMENT_3D ( 'NONE', #38579, #35331, #10385 ) ;
#13469 = VECTOR ( 'NONE', #1198, 1000.000000000000227 ) ;
#13470 = CARTESIAN_POINT ( 'NONE',  ( 1.700390093233090871, -29.56993018339339940, 7.800000000000000711 ) ) ;
#13471 = ORIENTED_EDGE ( 'NONE', *, *, #5354, .T. ) ;
#13472 = CARTESIAN_POINT ( 'NONE',  ( 36.13290868086723862, -1.530173128070416055, -5.643002085621601438 ) ) ;
#13473 = DIRECTION ( 'NONE',  ( 1.000000000000000000, 1.273455763949465563E-16, 0.000000000000000000 ) ) ;
#13474 = AXIS2_PLACEMENT_3D ( 'NONE', #37371, #5681, #34731 ) ;
#13475 = DIRECTION ( 'NONE',  ( 0.000000000000000000, -0.000000000000000000, -1.000000000000000000 ) ) ;
#13476 = CARTESIAN_POINT ( 'NONE',  ( 5.110926626256952154, -30.35622219256811150, 6.912143950357345190 ) ) ;
#13477 = FACE_OUTER_BOUND ( 'NONE', #33098, .T. ) ;
#13478 = CARTESIAN_POINT ( 'NONE',  ( 30.43224445366828235, -3.649418619126846508, 4.685639825479781528 ) ) ;
#13479 = CARTESIAN_POINT ( 'NONE',  ( 5.094086365274872463, -29.77691027265591828, 6.979335674598010186 ) ) ;
#13480 = CIRCLE ( 'NONE', #1012, 3.778021175560965172 ) ;
#13481 = DIRECTION ( 'NONE',  ( -0.000000000000000000, -0.000000000000000000, 1.000000000000000000 ) ) ;
#13482 = CARTESIAN_POINT ( 'NONE',  ( 21.94609799796423744, 0.7904948903713955310, -7.266583015939693801 ) ) ;
#13483 = CARTESIAN_POINT ( 'NONE',  ( 34.16050310316816052, -0.5835275994841344627, -5.173420616574753161 ) ) ;
#13484 = CARTESIAN_POINT ( 'NONE',  ( 20.40287464304303100, 10.75613383955523616, -2.500000000000000000 ) ) ;
#13485 = VERTEX_POINT ( 'NONE', #22007 ) ;
#13486 = CARTESIAN_POINT ( 'NONE',  ( 66.85348068378573316, 57.96691244536589238, 3.999524142431096330 ) ) ;
#13487 = ADVANCED_FACE ( 'NONE', ( #40500 ), #25295, .F. ) ;
#13488 = EDGE_CURVE ( 'NONE', #39731, #10043, #12721, .T. ) ;
#13489 = CARTESIAN_POINT ( 'NONE',  ( 84.34456690318765482, 2.887654542466673746, -2.101772343363317752 ) ) ;
#13490 = ADVANCED_FACE ( 'NONE', ( #31474 ), #31677, .T. ) ;
#13491 = DIRECTION ( 'NONE',  ( 0.000000000000000000, 0.000000000000000000, 1.000000000000000000 ) ) ;
#13492 = ORIENTED_EDGE ( 'NONE', *, *, #19769, .F. ) ;
#13493 = CARTESIAN_POINT ( 'NONE',  ( -81.51664041560071894, 10.48936286263200834, -2.744537766835254189 ) ) ;
#13494 = CARTESIAN_POINT ( 'NONE',  ( -0.4881783139857213683, -26.85647531738399252, 7.784725160561908552 ) ) ;
#13495 = APPLICATION_PROTOCOL_DEFINITION ( 'draft international standard', 'automotive_design', 1998, #8952 ) ;
#13496 = CARTESIAN_POINT ( 'NONE',  ( 2.326171464738295835, -32.91184545387483951, 7.703977250142848732 ) ) ;
#13497 = CARTESIAN_POINT ( 'NONE',  ( -0.4487487021806388365, -25.49307895267003587, 6.800000000000000711 ) ) ;
#13498 = VERTEX_POINT ( 'NONE', #15819 ) ;
#13499 = CARTESIAN_POINT ( 'NONE',  ( 5.054793046568992310, -30.12489038615697012, 7.693875151218752428 ) ) ;
#13500 = CIRCLE ( 'NONE', #36512, 0.1000000000000028644 ) ;
#13501 = CIRCLE ( 'NONE', #39835, 0.1000000000000028644 ) ;
#13502 = ORIENTED_EDGE ( 'NONE', *, *, #5841, .T. ) ;
#13503 = CARTESIAN_POINT ( 'NONE',  ( 78.57218090866955151, 65.76747258267620566, -2.123311106147462546 ) ) ;
#13504 = CARTESIAN_POINT ( 'NONE',  ( 37.13477802123105675, -2.471947244483942097, 5.963681894023967089 ) ) ;
#13505 = CARTESIAN_POINT ( 'NONE',  ( 79.79878548311236841, 63.97024398824610358, 3.714073935154437844 ) ) ;
#13507 = ORIENTED_EDGE ( 'NONE', *, *, #21772, .T. ) ;
#13506 = CARTESIAN_POINT ( 'NONE',  ( -0.6393902300633312885, -25.40346598495485253, 7.013842709614101167 ) ) ;
#13508 = VECTOR ( 'NONE', #4094, 1000.000000000000000 ) ;
#13509 = CARTESIAN_POINT ( 'NONE',  ( -80.92837670882107659, 2.429809908903242555, 12.50000000000000000 ) ) ;
#13510 = CARTESIAN_POINT ( 'NONE',  ( 0.9376568889370265891, -32.98581865358281107, 6.883550009118462931 ) ) ;
#13511 = DIRECTION ( 'NONE',  ( 0.000000000000000000, -0.7126435865141276249, 0.7015262779114413982 ) ) ;
#13512 = CARTESIAN_POINT ( 'NONE',  ( 21.85643539959774273, 11.61750052538138256, -3.706567411524428479 ) ) ;
#13513 = DIRECTION ( 'NONE',  ( 0.000000000000000000, 0.000000000000000000, -1.000000000000000000 ) ) ;
#13514 = CARTESIAN_POINT ( 'NONE',  ( 24.40656851573213260, 3.164061221018514836, -3.268877201782123709 ) ) ;
#13515 = ORIENTED_EDGE ( 'NONE', *, *, #18923, .F. ) ;
#13516 = CARTESIAN_POINT ( 'NONE',  ( 71.72449567874917875, 61.26021252176497001, -3.629688915602770294 ) ) ;
#13517 = ORIENTED_EDGE ( 'NONE', *, *, #26203, .T. ) ;
#13518 = CARTESIAN_POINT ( 'NONE',  ( -0.9367813558391736573, -31.71593409404636787, 6.892063359921931642 ) ) ;
#13519 = CARTESIAN_POINT ( 'NONE',  ( 4.282054009272330930, -27.35746286227295343, 7.680992449362119778 ) ) ;
#13520 = CARTESIAN_POINT ( 'NONE',  ( -71.87663712502020985, 3.986363140443492270, -9.955339895040744125 ) ) ;
#13521 = CARTESIAN_POINT ( 'NONE',  ( 1.700390093233090871, -29.56993018339339940, 27.90461065042423527 ) ) ;
#13522 = CARTESIAN_POINT ( 'NONE',  ( -0.8786759135921904385, -26.64985754041175525, 6.800000000000000711 ) ) ;
#13523 = CARTESIAN_POINT ( 'NONE',  ( 78.78605531729427014, 66.08782950793387556, 1.450104216466330920 ) ) ;
#13524 = CARTESIAN_POINT ( 'NONE',  ( 84.33668400229728945, 2.728897857615574019, 2.746074863882507877 ) ) ;
#13525 = B_SPLINE_CURVE_WITH_KNOTS ( 'NONE', 3,
 ( #26270, #13496, #38995, #26069, #22581, #20270, #10405, #32853, #1557, #4642, #35548, #17176, #32056, #7317, #3862, #25859, #38398, #40030, #8313, #30156, #11800, #39831, #8724, #11602, #21304 ),
 .UNSPECIFIED., .F., .F.,
 ( 4, 3, 3, 3, 3, 3, 3, 3, 4 ),
 ( 6.468151674593655405E-05, 9.076621574722012922E-05, 0.0001210204262067964080, 0.0001512763324577413155, 0.0001815301820994202919, 0.0002117781465860697028, 0.0002420274594459747739, 0.0002722905548971149212, 0.0002816827545175575411 ),
 .UNSPECIFIED. ) ;
#13526 = FACE_OUTER_BOUND ( 'NONE', #19578, .T. ) ;
#13527 = CARTESIAN_POINT ( 'NONE',  ( -0.8851723638970985242, -31.77784023144311476, 7.661510568013098599 ) ) ;
#13528 = CARTESIAN_POINT ( 'NONE',  ( 3.930147992295620174, -26.87211838299319311, 7.737115613922535218 ) ) ;
#13529 = VECTOR ( 'NONE', #15187, 1000.000000000000000 ) ;
#13530 = VECTOR ( 'NONE', #33423, 1000.000000000000000 ) ;
#13531 = DIRECTION ( 'NONE',  ( 1.000000000000000000, 0.000000000000000000, 0.000000000000000000 ) ) ;
#13532 = CARTESIAN_POINT ( 'NONE',  ( -0.3879985392179198245, -26.88688304283302344, 6.863904403958575706 ) ) ;
#13533 = DIRECTION ( 'NONE',  ( 1.000000000000000000, -0.000000000000000000, -0.000000000000000000 ) ) ;
#13534 = CARTESIAN_POINT ( 'NONE',  ( 69.11491457486368972, 59.02763561571557460, 3.981537309218734055 ) ) ;
#13535 = CARTESIAN_POINT ( 'NONE',  ( 33.62865206644069360, -1.228866384903354092, 5.454962485628514379 ) ) ;
#13536 = VECTOR ( 'NONE', #3782, 1000.000000000000000 ) ;
#13537 = LINE ( 'NONE', #28992, #22727 ) ;
#13538 = CARTESIAN_POINT ( 'NONE',  ( 86.67773139875836819, 0.9971827163122055637, 5.329716871657868005 ) ) ;
#13539 = ADVANCED_FACE ( 'NONE', ( #34175 ), #9219, .F. ) ;
#13541 = CARTESIAN_POINT ( 'NONE',  ( 4.818790771865216982, -30.92476493623475164, 6.929923840112062194 ) ) ;
#13540 = CARTESIAN_POINT ( 'NONE',  ( 79.58225024864499630, 65.28851876552752742, -3.146509185145911935 ) ) ;
#13542 = CARTESIAN_POINT ( 'NONE',  ( -1.229875790497353405, -27.65589205167745490, 6.961115707816238007 ) ) ;
#13543 = CARTESIAN_POINT ( 'NONE',  ( -56.50908310466263629, 29.95896301100009040, 1.719924897558617438 ) ) ;
#13544 = ORIENTED_EDGE ( 'NONE', *, *, #31523, .F. ) ;
#13545 = CARTESIAN_POINT ( 'NONE',  ( -60.14275962559869981, 24.84364830758654108, -9.154021781743367114 ) ) ;
#13546 = VERTEX_POINT ( 'NONE', #28373 ) ;
#13547 = CARTESIAN_POINT ( 'NONE',  ( -72.55849701049024247, 6.338670283186906396, 9.867990834847722326 ) ) ;
#13548 = ORIENTED_EDGE ( 'NONE', *, *, #30724, .F. ) ;
#13549 = CARTESIAN_POINT ( 'NONE',  ( 80.00358288781660576, 64.08847832824481827, -3.683925914261568124 ) ) ;
#13550 = DIRECTION ( 'NONE',  ( -0.000000000000000000, -1.000000000000000000, -0.000000000000000000 ) ) ;
#13551 = CARTESIAN_POINT ( 'NONE',  ( 22.01028799361013455, 1.448149096448989148, 6.405474035339984162 ) ) ;
#13553 = VERTEX_POINT ( 'NONE', #11888 ) ;
#13552 = ORIENTED_EDGE ( 'NONE', *, *, #20624, .T. ) ;
#13554 = CARTESIAN_POINT ( 'NONE',  ( 81.37441939350041764, 61.42019823254031508, -1.301239782962684499 ) ) ;
#13555 = CARTESIAN_POINT ( 'NONE',  ( 5.033237860645672690, -30.24233315725131277, 6.870716933885662847 ) ) ;
#13557 = DIRECTION ( 'NONE',  ( 0.000000000000000000, 0.000000000000000000, 1.000000000000000000 ) ) ;
#13556 = CARTESIAN_POINT ( 'NONE',  ( 4.616164590409697510, -31.31871807265113006, 6.887041543973317914 ) ) ;
#13558 = CARTESIAN_POINT ( 'NONE',  ( -4.248748702180636272, -26.64985754041175525, 6.700000000000000178 ) ) ;
#13559 = CIRCLE ( 'NONE', #6352, 0.1000000000000028644 ) ;
#13560 = CARTESIAN_POINT ( 'NONE',  ( -64.08758708074093136, 43.44355869127355163, -1.729337824599811668 ) ) ;
#13561 = CARTESIAN_POINT ( 'NONE',  ( 72.50225525176000474, 58.97572275893025306, 3.745173303611597948 ) ) ;
#13562 = EDGE_CURVE ( 'NONE', #12553, #9974, #21386, .T. ) ;
#13563 = CARTESIAN_POINT ( 'NONE',  ( 21.85277127755108850, 4.059747631923805500, -4.311690313514618289 ) ) ;
#13564 = ORIENTED_EDGE ( 'NONE', *, *, #5052, .F. ) ;
#13565 = FACE_OUTER_BOUND ( 'NONE', #31051, .T. ) ;
#13566 = VECTOR ( 'NONE', #34006, 1000.000000000000000 ) ;
#13567 = VERTEX_POINT ( 'NONE', #40305 ) ;
#13568 = CARTESIAN_POINT ( 'NONE',  ( 21.85643539959774984, 7.798985686765059100, -6.733359799098007414 ) ) ;
#13569 = CARTESIAN_POINT ( 'NONE',  ( 17.10505430642727021, 14.50076029600939620, -3.172244300427717878 ) ) ;
#13570 = CARTESIAN_POINT ( 'NONE',  ( -36.34874870218064302, -25.49307895267003587, 6.800000000000000711 ) ) ;
#13571 = CARTESIAN_POINT ( 'NONE',  ( 81.64588081866192226, 62.19174680641864228, 2.443770662203105459 ) ) ;
#13572 = CARTESIAN_POINT ( 'NONE',  ( 87.33013056844055200, 0.1115698105147486796, -5.569409363020906056 ) ) ;
#13573 = CARTESIAN_POINT ( 'NONE',  ( 26.00676459590870948, -2.423824083598640655, 4.803740791041811953 ) ) ;
#13574 = ORIENTED_EDGE ( 'NONE', *, *, #9324, .F. ) ;
#13575 = CARTESIAN_POINT ( 'NONE',  ( 26.28262498061524255, -2.815787221564533649, 4.308437294549054997 ) ) ;
#13576 = EDGE_CURVE ( 'NONE', #25891, #3311, #12162, .T. ) ;
#13577 = CARTESIAN_POINT ( 'NONE',  ( 5.078024580013459577, -29.18059064813925829, 6.988553391373222290 ) ) ;
#13578 = CARTESIAN_POINT ( 'NONE',  ( 26.27644361979791299, -2.815469118397957438, -4.307472543696508005 ) ) ;
#13579 = CARTESIAN_POINT ( 'NONE',  ( 36.14145924306839675, -3.142491748452399758, -5.847146818012371128 ) ) ;
#13580 = CARTESIAN_POINT ( 'NONE',  ( -34.44874870218064444, -26.64985754041175525, 6.700000000000000178 ) ) ;
#13581 = LINE ( 'NONE', #23262, #29875 ) ;
#13582 = DIRECTION ( 'NONE',  ( 0.000000000000000000, 0.000000000000000000, 1.000000000000000000 ) ) ;
#13583 = ORIENTED_EDGE ( 'NONE', *, *, #23579, .T. ) ;
#13584 = CARTESIAN_POINT ( 'NONE',  ( 1.887380280259158383, -26.17507603778478753, 7.013842709614101167 ) ) ;
#13585 = CARTESIAN_POINT ( 'NONE',  ( -28.97867591359219475, -24.55319635012989110, 6.700000000000000178 ) ) ;
#13586 = CARTESIAN_POINT ( 'NONE',  ( 32.88573892376593477, -3.567000722825174996, 5.242007489099518303 ) ) ;
#13587 = EDGE_CURVE ( 'NONE', #15847, #24744, #21594, .T. ) ;
#13588 = ORIENTED_EDGE ( 'NONE', *, *, #754, .T. ) ;
#13589 = ORIENTED_EDGE ( 'NONE', *, *, #793, .F. ) ;
#13590 = CARTESIAN_POINT ( 'NONE',  ( 37.21201414827569209, -2.743731264475244735, 6.000895904599971686 ) ) ;
#13591 = LINE ( 'NONE', #23272, #15926 ) ;
#13592 = AXIS2_PLACEMENT_3D ( 'NONE', #13046, #22539, #34495 ) ;
#13593 = CARTESIAN_POINT ( 'NONE',  ( 66.27376694609004915, 57.73522568913436004, -4.000000000000000000 ) ) ;
#13594 = AXIS2_PLACEMENT_3D ( 'NONE', #4567, #16687, #35666 ) ;
#13595 = CARTESIAN_POINT ( 'NONE',  ( 87.74957675019172143, -2.299229798971626160, -2.336605637469935548 ) ) ;
#13596 = CIRCLE ( 'NONE', #29383, 0.1000000000000028644 ) ;
#13597 = VERTEX_POINT ( 'NONE', #2877 ) ;
#13598 = CARTESIAN_POINT ( 'NONE',  ( -64.08758708074093136, 36.76569972833215161, -3.434863364314911571 ) ) ;
#13599 = EDGE_LOOP ( 'NONE', ( #12382, #19797, #6000, #37955 ) ) ;
#13600 = CARTESIAN_POINT ( 'NONE',  ( -56.05592576813389627, 30.85738657449433120, -3.898523360614985833 ) ) ;
#13601 = CARTESIAN_POINT ( 'NONE',  ( 3.813414093473169064, -32.36011468883553732, 7.006908160621414972 ) ) ;
#13602 = ORIENTED_EDGE ( 'NONE', *, *, #4786, .T. ) ;
#13603 = CARTESIAN_POINT ( 'NONE',  ( 23.14817712711864672, 3.972822056005928193, 3.193607562712095227 ) ) ;
#13604 = CARTESIAN_POINT ( 'NONE',  ( 81.49402754981267094, 65.64225023272284432, -1.838010297257802517 ) ) ;
#13605 = EDGE_CURVE ( 'NONE', #11880, #22985, #18753, .T. ) ;
#13606 = CARTESIAN_POINT ( 'NONE',  ( -42.44874870218064444, -25.49307895267003587, 6.700000000000000178 ) ) ;
#13607 = ORIENTED_EDGE ( 'NONE', *, *, #26602, .F. ) ;
#13608 = CARTESIAN_POINT ( 'NONE',  ( 76.31287196683634022, 61.24236878174163934, -3.825872951957620671 ) ) ;
#13610 = CARTESIAN_POINT ( 'NONE',  ( 0.1825688514504736626, 0.5999999999999995337, -3.931742364880508767 ) ) ;
#13609 = CARTESIAN_POINT ( 'NONE',  ( -1.599498859172472809, -28.40342561769650231, 7.670465701733752972 ) ) ;
#13611 = CARTESIAN_POINT ( 'NONE',  ( -70.66586135525236045, 0.1905911290138092018, 5.995467141624639673 ) ) ;
#13612 = CARTESIAN_POINT ( 'NONE',  ( 77.29397510068359622, 60.62518447217941997, 3.385286751607368139 ) ) ;
#13613 = DIRECTION ( 'NONE',  ( 0.000000000000000000, 0.000000000000000000, 1.000000000000000000 ) ) ;
#13614 = AXIS2_PLACEMENT_3D ( 'NONE', #3528, #16254, #28825 ) ;
#13615 = FACE_OUTER_BOUND ( 'NONE', #16576, .T. ) ;
#13616 = CARTESIAN_POINT ( 'NONE',  ( 25.78025694704896509, 1.897212611309158747, -4.230030613094124092 ) ) ;
#13617 = DIRECTION ( 'NONE',  ( 0.000000000000000000, 0.000000000000000000, 1.000000000000000000 ) ) ;
#13618 = CARTESIAN_POINT ( 'NONE',  ( 81.41940809751211816, 61.44195378529070695, 1.227604746834739080 ) ) ;
#13619 = CARTESIAN_POINT ( 'NONE',  ( 86.66388813748453401, 1.012732124415782531, -5.000054679117940104 ) ) ;
#13620 = B_SPLINE_CURVE_WITH_KNOTS ( 'NONE', 3,
 ( #23028, #35595, #7365, #32495, #8928, #24382, #15317, #18194, #30988, #33671, #31386, #37539, #21915, #8723, #25002, #14138, #26714, #5863, #9138, #15522, #5656, #27474, #9335, #15113, #24801 ),
 .UNSPECIFIED., .F., .F.,
 ( 4, 3, 3, 3, 3, 3, 3, 3, 4 ),
 ( 6.468151674593491419E-05, 9.076621574722202658E-05, 0.0001210204262067985493, 0.0001512763324577458149, 0.0001815301820994193703, 0.0002117781465860703533, 0.0002420274594459763189, 0.0002722905548971134033, 0.0002816827545175533670 ),
 .UNSPECIFIED. ) ;
#13621 = CARTESIAN_POINT ( 'NONE',  ( 28.77170544830297416, -1.679059579700503901, 5.945470488877720783 ) ) ;
#13622 = EDGE_CURVE ( 'NONE', #38197, #19595, #31874, .T. ) ;
#13623 = EDGE_CURVE ( 'NONE', #11094, #26805, #22817, .T. ) ;
#13624 = CARTESIAN_POINT ( 'NONE',  ( 2.369913428640782804, -26.23648987328603610, 7.782034975670476307 ) ) ;
#13625 = CIRCLE ( 'NONE', #11627, 0.1000000000000028644 ) ;
#13626 = CARTESIAN_POINT ( 'NONE',  ( 3.573240303917499361, -26.73224942468579357, 6.988553391373220514 ) ) ;
#13627 = VECTOR ( 'NONE', #29403, 1000.000000000000000 ) ;
#13628 = EDGE_CURVE ( 'NONE', #463, #8120, #11829, .T. ) ;
#13629 = CARTESIAN_POINT ( 'NONE',  ( -81.73797001107014637, -5.609980832826766850, -1.463193866445242186 ) ) ;
#13630 = CARTESIAN_POINT ( 'NONE',  ( -2.689021718275399042, -31.29716697405881476, 7.754798119455333705 ) ) ;
#13631 = CARTESIAN_POINT ( 'NONE',  ( 3.938183569304232634, -26.87878085491623636, 7.638132480492516585 ) ) ;
#13632 = CARTESIAN_POINT ( 'NONE',  ( 37.02894987274358130, -3.025198956107289394, -5.984733352030005449 ) ) ;
#13633 = CARTESIAN_POINT ( 'NONE',  ( -8.248748702180632719, -26.64985754041175525, 6.700000000000000178 ) ) ;
#13634 = CARTESIAN_POINT ( 'NONE',  ( -39.07867591359219261, -24.55319635012989110, 6.800000000000000711 ) ) ;
#13635 = CARTESIAN_POINT ( 'NONE',  ( -1.699609906766908818, -29.56993018339339940, 7.222147233343546802 ) ) ;
#13636 = CARTESIAN_POINT ( 'NONE',  ( 2.234964567898549692, -32.92764222152831621, 6.887041543973314361 ) ) ;
#13637 = CARTESIAN_POINT ( 'NONE',  ( 21.89416422391149553, -13.03218691091165482, -2.499999999999999556 ) ) ;
#13638 = FACE_OUTER_BOUND ( 'NONE', #16839, .T. ) ;
#13639 = EDGE_LOOP ( 'NONE', ( #12016, #10803, #441, #5796, #19222, #5412 ) ) ;
#13640 = CARTESIAN_POINT ( 'NONE',  ( 30.66838910461938283, 0.2949634357040269994, 4.962894452049861904 ) ) ;
#13641 = EDGE_CURVE ( 'NONE', #7892, #12826, #8868, .T. ) ;
#13642 = DIRECTION ( 'NONE',  ( -1.000000000000000000, 0.000000000000000000, 0.000000000000000000 ) ) ;
#13643 = CARTESIAN_POINT ( 'NONE',  ( 67.67991563464998706, 58.42724437289452055, -3.992148460412344502 ) ) ;
#13644 = PLANE ( 'NONE',  #32498 ) ;
#13645 = VECTOR ( 'NONE', #14363, 1000.000000000000000 ) ;
#13646 = ORIENTED_EDGE ( 'NONE', *, *, #35490, .F. ) ;
#13647 = DIRECTION ( 'NONE',  ( -0.9616058754224561245, 0.2744342186262705430, 0.000000000000000000 ) ) ;
#13648 = CARTESIAN_POINT ( 'NONE',  ( 30.88504653261737687, -3.473826543452005922, 4.907706032697572773 ) ) ;
#13649 = CARTESIAN_POINT ( 'NONE',  ( -60.14275962559869981, 24.84364830758654108, 9.154021781743367114 ) ) ;
#13650 = CARTESIAN_POINT ( 'NONE',  ( 5.049345966743696401, -28.55282231546490479, 6.931070083220556732 ) ) ;
#13651 = CARTESIAN_POINT ( 'NONE',  ( 21.71182896267971074, 6.328908860361642574, -3.192117583127509928 ) ) ;
#13652 = CARTESIAN_POINT ( 'NONE',  ( 0.3491796791923181265, -32.79858786375961444, 6.890920332093119605 ) ) ;
#13653 = VECTOR ( 'NONE', #37224, 1000.000000000000000 ) ;
#13654 = VECTOR ( 'NONE', #28752, 1000.000000000000000 ) ;
#13655 = CARTESIAN_POINT ( 'NONE',  ( -1.696743409393115520, -30.44007608545301125, 7.501983001166816933 ) ) ;
#13656 = ORIENTED_EDGE ( 'NONE', *, *, #39133, .T. ) ;
#13657 = CARTESIAN_POINT ( 'NONE',  ( 22.38195073352680353, 4.938598426050218038, 3.049351103695999932 ) ) ;
#13658 = DIRECTION ( 'NONE',  ( -1.000000000000000000, 0.000000000000000000, 0.000000000000000000 ) ) ;
#13659 = CARTESIAN_POINT ( 'NONE',  ( 80.79424907316142423, 63.37012793878832184, 3.540619799101252685 ) ) ;
#13660 = CARTESIAN_POINT ( 'NONE',  ( -30.97867591359219119, -24.55319635012989110, 6.800000000000000711 ) ) ;
#13661 = ORIENTED_EDGE ( 'NONE', *, *, #7555, .T. ) ;
#13662 = CARTESIAN_POINT ( 'NONE',  ( 79.66869450427640231, 60.77384974161335407, -2.178915381671177265 ) ) ;
#13664 = CARTESIAN_POINT ( 'NONE',  ( -1.735425026873168575, -28.90271622936575113, 6.872994525451590953 ) ) ;
#13663 = CARTESIAN_POINT ( 'NONE',  ( 23.06111833571992165, 0.3526964807778580901, 5.951137662820944918 ) ) ;
#13665 = CARTESIAN_POINT ( 'NONE',  ( 81.48104477345277985, 62.99720032632139066, -3.089171411835851089 ) ) ;
#13666 = CARTESIAN_POINT ( 'NONE',  ( 80.45616750117871163, 61.42990784962029949, 2.551437666014049199 ) ) ;
#13667 = EDGE_CURVE ( 'NONE', #1735, #20773, #12852, .T. ) ;
#13668 = LINE ( 'NONE', #7282, #28019 ) ;
#13669 = ADVANCED_FACE ( 'NONE', ( #4281 ), #7353, .T. ) ;
#13670 = CARTESIAN_POINT ( 'NONE',  ( 81.74784679736075077, 61.69507302169112251, 1.045691535380373960 ) ) ;
#13672 = ORIENTED_EDGE ( 'NONE', *, *, #7014, .F. ) ;
#13671 = DIRECTION ( 'NONE',  ( 0.000000000000000000, 0.000000000000000000, 1.000000000000000000 ) ) ;
#13673 = AXIS2_PLACEMENT_3D ( 'NONE', #9199, #21576, #6542 ) ;
#13674 = CARTESIAN_POINT ( 'NONE',  ( 25.45397947482645762, -4.047761836529544688, -3.708248611797466232 ) ) ;
#13675 = CARTESIAN_POINT ( 'NONE',  ( -64.44214806826670383, 36.58397470404546681, -5.707342493246947868 ) ) ;
#13676 = VERTEX_POINT ( 'NONE', #22416 ) ;
#13677 = CARTESIAN_POINT ( 'NONE',  ( -74.01735817102475323, -1.775513542402386014, 9.566008380307465586 ) ) ;
#13678 = CARTESIAN_POINT ( 'NONE',  ( 26.06763238852761333, 0.7305626207722594190, -4.422385087239707246 ) ) ;
#13679 = ADVANCED_FACE ( 'NONE', ( #12930 ), #38038, .T. ) ;
#13680 = CARTESIAN_POINT ( 'NONE',  ( -2.735299443412492426, -31.17001996922091678, 7.635761828346577573 ) ) ;
#13681 = CIRCLE ( 'NONE', #4489, 3.449999999999999734 ) ;
#13682 = CARTESIAN_POINT ( 'NONE',  ( -0.9856834644577864291, -31.80018438340522025, 7.778495531946295394 ) ) ;
#13683 = ADVANCED_FACE ( 'NONE', ( #29187 ), #16218, .F. ) ;
#13684 = CARTESIAN_POINT ( 'NONE',  ( 34.63719001687865529, -0.7818850938027223085, -5.275113761647806321 ) ) ;
#13685 = CARTESIAN_POINT ( 'NONE',  ( 30.77571102275213732, -3.326538504857021294, -4.963279402896310089 ) ) ;
#13686 = CARTESIAN_POINT ( 'NONE',  ( 3.301837905240542881, -32.68206207414233688, 7.013842709614101167 ) ) ;
#13687 = CARTESIAN_POINT ( 'NONE',  ( 5.128444259610362543, -30.27593629695848421, 6.864216812847430127 ) ) ;
#13688 = CARTESIAN_POINT ( 'NONE',  ( 5.199619722107929221, -29.64405277551909279, 6.867280401193710304 ) ) ;
#13689 = CYLINDRICAL_SURFACE ( 'NONE', #29927, 3.873277249845555215 ) ;
#13690 = CARTESIAN_POINT ( 'NONE',  ( 5.095244238841699413, -29.75692037041947913, 7.013842709614101167 ) ) ;
#13691 = VECTOR ( 'NONE', #38410, 1000.000000000000000 ) ;
#13692 = CARTESIAN_POINT ( 'NONE',  ( 30.19238557334687911, -2.952639005720375742, -4.918649992961978690 ) ) ;
#13693 = DIRECTION ( 'NONE',  ( -0.000000000000000000, -0.000000000000000000, 1.000000000000000000 ) ) ;
#13694 = VERTEX_POINT ( 'NONE', #35185 ) ;
#13695 = CARTESIAN_POINT ( 'NONE',  ( 66.90457105084450973, 57.82508126828634687, 3.996770903026528821 ) ) ;
#13696 = CARTESIAN_POINT ( 'NONE',  ( -64.08758708074093136, 38.27681294190825412, 4.090925416972679862 ) ) ;
#13697 = B_SPLINE_CURVE_WITH_KNOTS ( 'NONE', 3,
 ( #36651, #24499, #21010, #12132, #36855, #30696, #27590, #37052, #18310, #6182 ),
 .UNSPECIFIED., .F., .F.,
 ( 4, 3, 3, 4 ),
 ( 1.022834283856302764E-18, 3.025570593003066596E-05, 6.051145698344103507E-05, 6.468151674593461604E-05 ),
 .UNSPECIFIED. ) ;
#13698 = CARTESIAN_POINT ( 'NONE',  ( 85.61743365444765175, 1.218782235343771836, 5.694237175320765232 ) ) ;
#13699 = DIRECTION ( 'NONE',  ( 0.000000000000000000, 0.000000000000000000, 1.000000000000000000 ) ) ;
#13700 =( BOUNDED_CURVE ( )  B_SPLINE_CURVE ( 3, ( #6510, #9168, #2620, #18427 ),
 .UNSPECIFIED., .F., .T. ) 
 B_SPLINE_CURVE_WITH_KNOTS ( ( 4, 4 ),
 ( 0.6656944266037794211, 1.570796326794896558 ),
 .UNSPECIFIED. ) 
 CURVE ( )  GEOMETRIC_REPRESENTATION_ITEM ( )  RATIONAL_B_SPLINE_CURVE ( ( 1.000000000000000000, 0.9328897322841716022, 0.9328897322841716022, 1.000000000000000000 ) ) 
 REPRESENTATION_ITEM ( '' )  );
#13701 = ORIENTED_EDGE ( 'NONE', *, *, #14864, .F. ) ;
#13702 = CARTESIAN_POINT ( 'NONE',  ( 2.881058359821971226, -26.27508231979332010, 7.750000000000000000 ) ) ;
#13703 = DIRECTION ( 'NONE',  ( 1.000000000000000000, 0.000000000000000000, 0.000000000000000000 ) ) ;
#13704 = DIRECTION ( 'NONE',  ( 0.9848077530122103518, -0.1736481776669172583, -0.000000000000000000 ) ) ;
#13705 = B_SPLINE_CURVE_WITH_KNOTS ( 'NONE', 3,
 ( #39858, #21131, #37375, #36972, #9171, #37172, #40254, #21336, #15347, #18632, #21743, #34325, #33908, #5685, #18228, #6096, #12040, #28113, #30817, #31218, #27700, #2623, #38381 ),
 .UNSPECIFIED., .F., .F.,
 ( 4, 1, 1, 1, 1, 1, 1, 2, 2, 1, 1, 1, 1, 1, 2, 2, 4 ),
 ( 0.000000000000000000, 0.1250000000000023870, 0.1875000000000044964, 0.2187500000000058842, 0.2343750000000065503, 0.2421875000000077993, 0.2460937500000071054, 0.2480468750000068001, 0.2500000000000064393, 0.3750000000000008882, 0.4374999999999990008, 0.4687499999999974465, 0.4843749999999963918, 0.4921874999999948375, 0.4960937499999947820, 0.4999999999999946709, 1.000000000000000000 ),
 .UNSPECIFIED. ) ;
#13706 = CARTESIAN_POINT ( 'NONE',  ( 1.122058404042096447, -26.12935236771179603, 7.781480525794718162 ) ) ;
#13707 = ORIENTED_EDGE ( 'NONE', *, *, #20042, .F. ) ;
#13708 = CARTESIAN_POINT ( 'NONE',  ( -70.92837670882107659, 26.72470171467712063, 6.406751979251626317 ) ) ;
#13709 = EDGE_CURVE ( 'NONE', #13567, #23822, #27981, .T. ) ;
#13710 = ORIENTED_EDGE ( 'NONE', *, *, #38903, .T. ) ;
#13711 = CARTESIAN_POINT ( 'NONE',  ( 78.47952394835841972, 65.90892955575903045, -1.487544896896269897 ) ) ;
#13712 = CARTESIAN_POINT ( 'NONE',  ( 13.68084587807537211, 8.951768997783636550, -3.481680170128817586 ) ) ;
#13713 = B_SPLINE_CURVE_WITH_KNOTS ( 'NONE', 3,
 ( #9783, #34930, #29334, #19859, #10584, #29537, #23749, #36320, #14277, #14072, #26255, #1350, #10387, #26846, #13884, #7299, #23156, #32431, #20657, #35528, #17156, #4434, #1539, #39387, #1153, #17556, #35926, #26050, #38978, #36123, #11178 ),
 .UNSPECIFIED., .F., .F.,
 ( 4, 3, 3, 3, 3, 3, 3, 3, 3, 3, 4 ),
 ( 1.084202172485504434E-18, 3.077658087705642108E-05, 6.152638666998993839E-05, 9.267501192706701653E-05, 0.0001241882240135197676, 0.0001556618703051697815, 0.0001866161554452206231, 0.0002167966385861002613, 0.0002463805737537787905, 0.0002758761370306537911, 0.0002847094172290030433 ),
 .UNSPECIFIED. ) ;
#13714 = CARTESIAN_POINT ( 'NONE',  ( 80.68879072954337062, 62.10584950744630106, 3.070011659370367241 ) ) ;
#13715 = DIRECTION ( 'NONE',  ( -1.000000000000000000, 0.000000000000000000, 0.000000000000000000 ) ) ;
#13716 = CIRCLE ( 'NONE', #1245, 2.681419499219045655 ) ;
#13717 = LINE ( 'NONE', #4257, #25833 ) ;
#13718 = CARTESIAN_POINT ( 'NONE',  ( 0.9066789574456146639, -32.97874561297109608, 6.974994249511788702 ) ) ;
#13719 = CARTESIAN_POINT ( 'NONE',  ( -36.87867591359218977, -26.64985754041175525, 6.700000000000000178 ) ) ;
#13720 = CARTESIAN_POINT ( 'NONE',  ( 21.85643539959780313, 0.8081825263151607430, -15.79083533483346535 ) ) ;
#13721 = CARTESIAN_POINT ( 'NONE',  ( 3.443786484529058889, -26.65091147862827370, 7.785868773668302545 ) ) ;
#13722 = ORIENTED_EDGE ( 'NONE', *, *, #20587, .F. ) ;
#13723 = CARTESIAN_POINT ( 'NONE',  ( 78.67055650824026714, 66.04450565822685348, -1.166185623126624993 ) ) ;
#13724 = EDGE_CURVE ( 'NONE', #23016, #26349, #6958, .T. ) ;
#13725 = ORIENTED_EDGE ( 'NONE', *, *, #27696, .F. ) ;
#13726 = ADVANCED_FACE ( 'NONE', ( #32293 ), #19910, .F. ) ;
#13727 = DIRECTION ( 'NONE',  ( -0.000000000000000000, -0.000000000000000000, 1.000000000000000000 ) ) ;
#13728 = CARTESIAN_POINT ( 'NONE',  ( -0.6306894173035869633, -32.17721693801968996, 7.766640943994337576 ) ) ;
#13729 = EDGE_CURVE ( 'NONE', #36180, #29149, #32097, .T. ) ;
#13730 = CARTESIAN_POINT ( 'NONE',  ( -75.21192073048329974, -3.284165063629141290, -10.40382875421505204 ) ) ;
#13731 = CYLINDRICAL_SURFACE ( 'NONE', #6401, 0.1000000000000028644 ) ;
#13732 = DIRECTION ( 'NONE',  ( 1.000000000000000000, 0.000000000000000000, 0.000000000000000000 ) ) ;
#13733 = CARTESIAN_POINT ( 'NONE',  ( 79.17166177841365027, 65.86836750419900000, 2.393593008231245545 ) ) ;
#13734 = CARTESIAN_POINT ( 'NONE',  ( 3.300000000000000711, 0.000000000000000000, 2.500000000000000000 ) ) ;
#13735 = CARTESIAN_POINT ( 'NONE',  ( 6.074096823854431726, -32.03256286660679564, 7.695279973900954751 ) ) ;
#13736 = CARTESIAN_POINT ( 'NONE',  ( -1.296339748590412677, -27.78971074760038462, 7.785096263473211486 ) ) ;
#13737 = DIRECTION ( 'NONE',  ( 0.000000000000000000, 0.000000000000000000, 1.000000000000000000 ) ) ;
#13738 = CARTESIAN_POINT ( 'NONE',  ( 1.665718984681162418, -26.17010605203765650, 7.712764235869103757 ) ) ;
#13739 = DIRECTION ( 'NONE',  ( 1.000000000000000000, 0.000000000000000000, 0.000000000000000000 ) ) ;
#13740 = LINE ( 'NONE', #29582, #34675 ) ;
#13741 = CARTESIAN_POINT ( 'NONE',  ( 3.855327937537480487, -32.32757912347058493, 7.754798119455333705 ) ) ;
#13742 = CARTESIAN_POINT ( 'NONE',  ( -63.96695182803194513, 19.27020452292901709, -8.800414904976364028 ) ) ;
#13743 = CARTESIAN_POINT ( 'NONE',  ( 69.39861229970156842, 58.29198505329483027, 3.933428174212719952 ) ) ;
#13744 = CARTESIAN_POINT ( 'NONE',  ( 27.40774226395753388, 0.9655407106828844954, 4.484039057678827156 ) ) ;
#13745 = AXIS2_PLACEMENT_3D ( 'NONE', #8242, #14832, #21232 ) ;
#13746 = CARTESIAN_POINT ( 'NONE',  ( -22.34874870218063947, -25.49307895267003587, 6.700000000000000178 ) ) ;
#13747 = CARTESIAN_POINT ( 'NONE',  ( 84.92887162652053235, 2.911150016110632510, -2.020846097872043501 ) ) ;
#13749 = CARTESIAN_POINT ( 'NONE',  ( -0.4068137048510813703, -26.77534493328523979, 6.912143950357340749 ) ) ;
#13748 = CARTESIAN_POINT ( 'NONE',  ( 81.15585419290073332, 61.98190721255070201, -2.710038060602454113 ) ) ;
#13750 = CARTESIAN_POINT ( 'NONE',  ( -1.230256760684643291, -27.65647541743870974, 6.941203072598475465 ) ) ;
#13751 = CARTESIAN_POINT ( 'NONE',  ( 2.324462049692062937, -26.13488154514125128, 7.778495531946297170 ) ) ;
#13752 = ORIENTED_EDGE ( 'NONE', *, *, #3898, .T. ) ;
#13753 = CARTESIAN_POINT ( 'NONE',  ( -10.34874870218063769, -26.64985754041175525, 6.700000000000000178 ) ) ;
#13754 = CARTESIAN_POINT ( 'NONE',  ( 23.36034022128349363, -7.521608558640657805, -2.500000000000000444 ) ) ;
#13755 = ORIENTED_EDGE ( 'NONE', *, *, #26456, .T. ) ;
#13756 = VERTEX_POINT ( 'NONE', #13741 ) ;
#13757 = AXIS2_PLACEMENT_3D ( 'NONE', #4312, #13557, #10463 ) ;
#13758 = CARTESIAN_POINT ( 'NONE',  ( 80.84665409946079251, 62.14681778383292254, -3.018898740118487911 ) ) ;
#13759 = CARTESIAN_POINT ( 'NONE',  ( -64.08758708074091714, 24.84364830758654108, -8.800414904976364028 ) ) ;
#13760 = CARTESIAN_POINT ( 'NONE',  ( 81.10356443252399572, 61.32192396066507456, 1.621665796799052206 ) ) ;
#13761 = CARTESIAN_POINT ( 'NONE',  ( 25.02156159189623352, 1.129856609166535186, 4.599960578933319333 ) ) ;
#13762 = VERTEX_POINT ( 'NONE', #791 ) ;
#13763 = CARTESIAN_POINT ( 'NONE',  ( 0.03162470699431464694, -32.53223031769636009, 7.695279973900954751 ) ) ;
#13765 = CARTESIAN_POINT ( 'NONE',  ( 3.963564119169153077, -32.23977037706391258, 7.640616322432101981 ) ) ;
#13764 = CARTESIAN_POINT ( 'NONE',  ( -58.38231031521774383, 29.55838692813951951, -4.971618182862113322 ) ) ;
#13766 = DIRECTION ( 'NONE',  ( 0.000000000000000000, -0.6834397476448824671, 0.7300069255418740743 ) ) ;
#13767 = DIRECTION ( 'NONE',  ( 1.000000000000000000, 0.000000000000000000, 0.000000000000000000 ) ) ;
#13768 = CARTESIAN_POINT ( 'NONE',  ( 21.99199484643884617, 4.642299483723236087, -3.779662632850636861 ) ) ;
#13769 = VERTEX_POINT ( 'NONE', #4091 ) ;
#13770 = DIRECTION ( 'NONE',  ( 1.000000000000000000, 0.000000000000000000, 0.000000000000000000 ) ) ;
#13771 = VERTEX_POINT ( 'NONE', #13320 ) ;
#13772 = VECTOR ( 'NONE', #84, 1000.000000000000114 ) ;
#13773 = EDGE_CURVE ( 'NONE', #21380, #36954, #3046, .T. ) ;
#13774 = CARTESIAN_POINT ( 'NONE',  ( 23.93232801731964443, 3.995115622954060530, -2.300403959411237320 ) ) ;
#13776 = EDGE_CURVE ( 'NONE', #12843, #3833, #11632, .T. ) ;
#13775 = CARTESIAN_POINT ( 'NONE',  ( 21.80570325383041208, 6.356989464231460829, -3.898355529981889500 ) ) ;
#13777 = CARTESIAN_POINT ( 'NONE',  ( 0.3520804393569469948, -32.69116280221577853, 6.911401339314952708 ) ) ;
#13778 = CARTESIAN_POINT ( 'NONE',  ( 81.12957769509937123, 64.69578868775874980, 3.179853676208927560 ) ) ;
#13779 = CARTESIAN_POINT ( 'NONE',  ( 84.97295377430323526, 2.662001904288300302, 3.416982328422734305 ) ) ;
#13780 = CARTESIAN_POINT ( 'NONE',  ( -1.303108374136985104, -31.16335321463953534, 7.754798119455333705 ) ) ;
#13781 = EDGE_LOOP ( 'NONE', ( #14585, #21204, #9710, #17041, #17951 ) ) ;
#13782 = ORIENTED_EDGE ( 'NONE', *, *, #916, .F. ) ;
#13783 = CARTESIAN_POINT ( 'NONE',  ( 14.72357206727486556, -4.485203473217731052, 2.504367530671055331 ) ) ;
#13784 = CARTESIAN_POINT ( 'NONE',  ( 1.754540994691119460, -33.27093018339341768, 7.695279973900954751 ) ) ;
#13785 = CIRCLE ( 'NONE', #23643, 3.499999999999999556 ) ;
#13786 = CARTESIAN_POINT ( 'NONE',  ( -63.06901714727342068, 38.60153782280264778, 3.999999999999999112 ) ) ;
#13787 = CARTESIAN_POINT ( 'NONE',  ( 34.92879589194200918, -1.712044492387412742, -5.657881373695215821 ) ) ;
#13788 = CARTESIAN_POINT ( 'NONE',  ( -70.92837670882107659, -27.85319909218681644, -4.357836081054403010 ) ) ;
#13789 = CARTESIAN_POINT ( 'NONE',  ( 84.67345804563912282, 2.302372249231917412, 4.084305866287619047 ) ) ;
#13790 = CARTESIAN_POINT ( 'NONE',  ( 3.558396595903837056, -26.60381962644626697, 7.750000000000000888 ) ) ;
#13791 = CARTESIAN_POINT ( 'NONE',  ( -8.248748702180632719, -26.64985754041175525, 6.700000000000000178 ) ) ;
#13792 = CARTESIAN_POINT ( 'NONE',  ( -1.645707253693945438, -30.17297881286834027, 7.756377446753163873 ) ) ;
#13793 = CARTESIAN_POINT ( 'NONE',  ( -15.07867591359219439, -24.55319635012989110, 6.800000000000000711 ) ) ;
#13794 = VERTEX_POINT ( 'NONE', #20707 ) ;
#13795 = ORIENTED_EDGE ( 'NONE', *, *, #17922, .T. ) ;
#13796 = CARTESIAN_POINT ( 'NONE',  ( 35.73027522876729023, -1.304475999450107615, 5.538144598496089088 ) ) ;
#13797 = CARTESIAN_POINT ( 'NONE',  ( 16.44412387426018185, -3.224078058481200770, 2.772901251853813420 ) ) ;
#13798 = EDGE_CURVE ( 'NONE', #31681, #12012, #8139, .T. ) ;
#13799 = CARTESIAN_POINT ( 'NONE',  ( 14.77315594796849574, 13.19392823276453441, -2.500000000000005773 ) ) ;
#13800 = CARTESIAN_POINT ( 'NONE',  ( 86.28440875934980170, -0.2633909481622456195, 5.902347234764444117 ) ) ;
#13801 = VECTOR ( 'NONE', #11450, 1000.000000000000000 ) ;
#13802 = EDGE_LOOP ( 'NONE', ( #29447, #20921, #28650, #13875, #7157, #40338 ) ) ;
#13803 = CARTESIAN_POINT ( 'NONE',  ( 5.142603739873976565, -28.93654719523409824, 7.737115613922530777 ) ) ;
#13804 =( NAMED_UNIT ( * ) PLANE_ANGLE_UNIT ( ) SI_UNIT ( $, .RADIAN. ) );
#13805 = ORIENTED_EDGE ( 'NONE', *, *, #4934, .F. ) ;
#13806 = CARTESIAN_POINT ( 'NONE',  ( -7.078675913592194391, -24.55319635012989110, 6.700000000000000178 ) ) ;
#13807 = CARTESIAN_POINT ( 'NONE',  ( 3.868607535801338315, -32.31746327423868337, 6.863784140767623221 ) ) ;
#13808 = ORIENTED_EDGE ( 'NONE', *, *, #12467, .T. ) ;
#13809 = CARTESIAN_POINT ( 'NONE',  ( 21.93898495623947298, 5.250604734135974283, 3.452261465700366738 ) ) ;
#13810 = CARTESIAN_POINT ( 'NONE',  ( 78.69020857030078275, 66.05846869611056604, -1.014334479594670713 ) ) ;
#13811 = VECTOR ( 'NONE', #39839, 1000.000000000000000 ) ;
#13812 = DIRECTION ( 'NONE',  ( -0.000000000000000000, -1.000000000000000000, -0.000000000000000000 ) ) ;
#13813 = VERTEX_POINT ( 'NONE', #17605 ) ;
#13815 = DIRECTION ( 'NONE',  ( -1.000000000000000000, 0.000000000000000000, 0.000000000000000000 ) ) ;
#13814 = CARTESIAN_POINT ( 'NONE',  ( -0.8980191362577285563, -27.22509128144364610, 7.750000000000000888 ) ) ;
#13816 = CARTESIAN_POINT ( 'NONE',  ( 78.03839322897110264, 60.52053993360658524, 3.012346708730509803 ) ) ;
#13817 = CARTESIAN_POINT ( 'NONE',  ( 24.73513624196588268, 2.629268958504959564, -3.929116450179705122 ) ) ;
#13818 = ORIENTED_EDGE ( 'NONE', *, *, #26041, .T. ) ;
#13819 = CARTESIAN_POINT ( 'NONE',  ( -11.81496944966682960, -21.25669541281728669, 4.000000000000000000 ) ) ;
#13820 = DIRECTION ( 'NONE',  ( 1.000000000000000000, 0.000000000000000000, -0.000000000000000000 ) ) ;
#13822 = EDGE_CURVE ( 'NONE', #37478, #34807, #1062, .T. ) ;
#13821 = DIRECTION ( 'NONE',  ( -0.6502177225477864253, -0.3754033771448399559, 0.6605219282605377940 ) ) ;
#13823 = CARTESIAN_POINT ( 'NONE',  ( -62.84805993229080912, 35.59861336795816555, 5.826615769580637760 ) ) ;
#13824 = CYLINDRICAL_SURFACE ( 'NONE', #4418, 0.1000000000000028644 ) ;
#13825 = CARTESIAN_POINT ( 'NONE',  ( 81.24150567074694607, 65.50891479330012146, 2.400449347018090318 ) ) ;
#13826 = CARTESIAN_POINT ( 'NONE',  ( -64.08758708074094557, 43.59044912938107075, 1.299988725261512545 ) ) ;
#13827 = CARTESIAN_POINT ( 'NONE',  ( 27.87470673840761037, 2.608020033772324275, -0.5247038454205935620 ) ) ;
#13828 = CARTESIAN_POINT ( 'NONE',  ( -23.07867591359219617, -26.64985754041175525, 6.800000000000000711 ) ) ;
#13829 = CARTESIAN_POINT ( 'NONE',  ( -70.42535609528330554, -21.65703093012598401, 9.988066921647984486 ) ) ;
#13830 = AXIS2_PLACEMENT_3D ( 'NONE', #19907, #16413, #16601 ) ;
#13831 = CYLINDRICAL_SURFACE ( 'NONE', #17589, 0.1000000000000028644 ) ;
#13832 = DIRECTION ( 'NONE',  ( 0.000000000000000000, 1.000000000000000000, 0.000000000000000000 ) ) ;
#13833 = CARTESIAN_POINT ( 'NONE',  ( 3.923398576026549289, -26.86655477908580281, 7.678495282201406980 ) ) ;
#13834 = CARTESIAN_POINT ( 'NONE',  ( 37.06194287117967434, -2.795410267932249671, -5.990810550159801906 ) ) ;
#13835 = DIRECTION ( 'NONE',  ( 1.000000000000000000, 0.000000000000000000, 0.000000000000000000 ) ) ;
#13836 = PLANE ( 'NONE',  #22019 ) ;
#13837 = CARTESIAN_POINT ( 'NONE',  ( -1.799514919472523955, -29.59631703906507738, 7.736930692279464949 ) ) ;
#13838 = CARTESIAN_POINT ( 'NONE',  ( -1.589323393843971477, -28.37905787987142148, 7.762796336881261361 ) ) ;
#13839 = CARTESIAN_POINT ( 'NONE',  ( -0.4574210171174863948, -32.19744825413003753, 7.693875151218751540 ) ) ;
#13840 = AXIS2_PLACEMENT_3D ( 'NONE', #7206, #19765, #13182 ) ;
#13841 = ORIENTED_EDGE ( 'NONE', *, *, #13339, .T. ) ;
#13842 = CARTESIAN_POINT ( 'NONE',  ( 35.80552223569445403, -3.523224689456814662, 5.749495820074442598 ) ) ;
#13843 = FACE_OUTER_BOUND ( 'NONE', #38550, .T. ) ;
#13844 = CARTESIAN_POINT ( 'NONE',  ( 67.16623404331231484, 58.01883467879599721, -3.998868826385353348 ) ) ;
#13845 = CARTESIAN_POINT ( 'NONE',  ( -1.348517286369409263, -27.85116208076715694, 7.695279973900954751 ) ) ;
#13846 = ORIENTED_EDGE ( 'NONE', *, *, #9414, .F. ) ;
#13847 = DIRECTION ( 'NONE',  ( 0.1736481776669404897, -0.9848077530122062440, -0.000000000000000000 ) ) ;
#13848 = CARTESIAN_POINT ( 'NONE',  ( -4.978675913592189417, -26.64985754041175525, 6.700000000000000178 ) ) ;
#13849 = CARTESIAN_POINT ( 'NONE',  ( 84.98208903537448577, 1.898203206837230983, -4.865140515105523811 ) ) ;
#13850 = CARTESIAN_POINT ( 'NONE',  ( 0.4695943777967604427, -26.29347754267606874, 7.686927408461904143 ) ) ;
#13851 = CARTESIAN_POINT ( 'NONE',  ( -1.445707822656724373, -28.28067938226085332, 6.865312560952602894 ) ) ;
#13852 = EDGE_CURVE ( 'NONE', #27757, #30983, #11533, .T. ) ;
#13853 = PLANE ( 'NONE',  #25387 ) ;
#13854 = CARTESIAN_POINT ( 'NONE',  ( 4.391539421710277225, -31.80772365946451430, 7.638132480492513032 ) ) ;
#13855 = ORIENTED_EDGE ( 'NONE', *, *, #10457, .T. ) ;
#13856 = ADVANCED_FACE ( 'NONE', ( #1797 ), #17008, .F. ) ;
#13857 = CARTESIAN_POINT ( 'NONE',  ( 21.83475994719001534, 5.936717745254647127, 3.147461123595437726 ) ) ;
#13858 = VECTOR ( 'NONE', #3995, 1000.000000000000000 ) ;
#13859 = DIRECTION ( 'NONE',  ( -6.367278819747329048E-17, -1.000000000000000000, 0.000000000000000000 ) ) ;
#13860 = CARTESIAN_POINT ( 'NONE',  ( 81.20569604368299110, 61.99964894245921698, 2.688322534164198085 ) ) ;
#13861 = CARTESIAN_POINT ( 'NONE',  ( -63.70319261593226656, 44.37193174353182457, 1.420345578797184150 ) ) ;
#13862 = ORIENTED_EDGE ( 'NONE', *, *, #23971, .T. ) ;
#13863 = CARTESIAN_POINT ( 'NONE',  ( 78.69960226590261243, 64.59913094042720161, -3.401284978681007320 ) ) ;
#13865 = CARTESIAN_POINT ( 'NONE',  ( -1.727598588168507421, -28.86353026780088982, 6.863641214238739074 ) ) ;
#13864 = CARTESIAN_POINT ( 'NONE',  ( 23.06597301177588477, 0.3557582928994350580, 5.946024084739200077 ) ) ;
#13866 = CARTESIAN_POINT ( 'NONE',  ( 81.30751890105065627, 61.38951540425596676, -1.382728580142338570 ) ) ;
#13867 = CARTESIAN_POINT ( 'NONE',  ( 78.36941018910007983, 65.17477963226572513, 2.845586111146954700 ) ) ;
#13868 = CARTESIAN_POINT ( 'NONE',  ( -70.92837670882107659, -23.80776546975053520, 10.00000000000000888 ) ) ;
#13869 = AXIS2_PLACEMENT_3D ( 'NONE', #30404, #24218, #26709 ) ;
#13870 = EDGE_CURVE ( 'NONE', #16321, #5140, #8324, .T. ) ;
#13871 = CARTESIAN_POINT ( 'NONE',  ( 80.01568814228021154, 66.35127795588812205, 1.246975333546937126 ) ) ;
#13872 = DIRECTION ( 'NONE',  ( -0.000000000000000000, -1.000000000000000000, -0.000000000000000000 ) ) ;
#13873 = CARTESIAN_POINT ( 'NONE',  ( 29.92651255597534288, -3.613225851372795727, -4.302012675596341928 ) ) ;
#13874 = CARTESIAN_POINT ( 'NONE',  ( -64.08758708074093136, 36.14363715547680300, -3.800414904976362696 ) ) ;
#13875 = ORIENTED_EDGE ( 'NONE', *, *, #9334, .F. ) ;
#13876 = CARTESIAN_POINT ( 'NONE',  ( -75.57379153473316080, -3.643616896758648860, 8.892515182195944945 ) ) ;
#13877 = CARTESIAN_POINT ( 'NONE',  ( 25.39897559319004827, 0.6933974945119176780, -4.599801555308138390 ) ) ;
#13878 = CARTESIAN_POINT ( 'NONE',  ( 1.751251297819361730, -25.49307895267003587, 6.700000000000000178 ) ) ;
#13879 = LINE ( 'NONE', #26044, #3293 ) ;
#13880 = EDGE_LOOP ( 'NONE', ( #7764, #33676, #927, #7793 ) ) ;
#13881 = CARTESIAN_POINT ( 'NONE',  ( 37.10418691205928354, -3.126297194733565821, -5.976226130023548855 ) ) ;
#13882 = B_SPLINE_CURVE_WITH_KNOTS ( 'NONE', 3,
 ( #32741, #39086, #32539, #4338, #23457, #20551, #4918, #17448, #30038, #36616, #18277, #5329, #21181, #9015, #2056, #36820, #40306, #2254, #17864, #34176, #27753, #9220, #8400, #2676, #14779 ),
 .UNSPECIFIED., .F., .F.,
 ( 4, 3, 3, 3, 3, 3, 3, 3, 4 ),
 ( 6.468151674593884443E-05, 9.076621574721885528E-05, 0.0001210204262067969636, 0.0001512763324577432399, 0.0001815301820994194787, 0.0002117781465860675073, 0.0002420274594459734729, 0.0002722905548971120480, 0.0002816827545175622032 ),
 .UNSPECIFIED. ) ;
#13883 = CARTESIAN_POINT ( 'NONE',  ( 3.290306094747008636, -32.68797150366361137, 6.912143950357342526 ) ) ;
#13884 = CARTESIAN_POINT ( 'NONE',  ( -1.082483681122714980, -31.69258464036479239, 6.887547729233692628 ) ) ;
#13885 = CARTESIAN_POINT ( 'NONE',  ( -72.42837670882107659, -47.11702805680359063, 5.809475019311127753 ) ) ;
#13886 = CARTESIAN_POINT ( 'NONE',  ( 2.673814629606090065, -32.82760982625630675, 6.911401339314953596 ) ) ;
#13887 = PLANE ( 'NONE',  #21077 ) ;
#13888 = AXIS2_PLACEMENT_3D ( 'NONE', #10886, #4141, #38689 ) ;
#13889 = ADVANCED_FACE ( 'NONE', ( #5274 ), #17815, .T. ) ;
#13890 = DIRECTION ( 'NONE',  ( 0.9848077530122080203, 0.1736481776669307198, -0.000000000000000000 ) ) ;
#13891 = CARTESIAN_POINT ( 'NONE',  ( 2.164714747183682952, -33.03899383454390204, 6.875780273367530171 ) ) ;
#13892 = ORIENTED_EDGE ( 'NONE', *, *, #6816, .F. ) ;
#13893 = ORIENTED_EDGE ( 'NONE', *, *, #31027, .F. ) ;
#13894 = CARTESIAN_POINT ( 'NONE',  ( 66.43187891275407253, 57.76301247919355575, 4.000000000000005329 ) ) ;
#13895 = CARTESIAN_POINT ( 'NONE',  ( 71.16717283274410022, 58.92450812456241493, -3.908768822720080305 ) ) ;
#13896 = CARTESIAN_POINT ( 'NONE',  ( 2.272716057154847924, -26.11704110451741556, 7.695279973900954751 ) ) ;
#13897 = CARTESIAN_POINT ( 'NONE',  ( 84.20866968570335587, 3.050835305001676101, 0.3231758755354003920 ) ) ;
#13898 = CARTESIAN_POINT ( 'NONE',  ( 26.60317387207919637, 1.634061885071666387, 4.331281458463850598 ) ) ;
#13899 = APPLICATION_PROTOCOL_DEFINITION ( 'draft international standard', 'automotive_design', 1998, #39741 ) ;
#13900 = CARTESIAN_POINT ( 'NONE',  ( 2.885910282437001761, -26.27682094667402879, 7.756742906098588186 ) ) ;
#13901 = EDGE_CURVE ( 'NONE', #15938, #10309, #17208, .T. ) ;
#13902 = DIRECTION ( 'NONE',  ( 0.000000000000000000, 0.000000000000000000, 1.000000000000000000 ) ) ;
#13903 = CARTESIAN_POINT ( 'NONE',  ( 5.107338069706632844, -29.53735381186853814, 7.257242401810562349 ) ) ;
#13904 = ORIENTED_EDGE ( 'NONE', *, *, #18077, .F. ) ;
#13905 = CARTESIAN_POINT ( 'NONE',  ( 78.99843287308405593, 65.13824187233505825, -3.101774481621350610 ) ) ;
#13906 = DIRECTION ( 'NONE',  ( 1.000000000000000000, 0.000000000000000000, 0.000000000000000000 ) ) ;
#13907 = CARTESIAN_POINT ( 'NONE',  ( 79.97265554093038986, 63.70311272660544688, 3.710743084827281546 ) ) ;
#13908 = DIRECTION ( 'NONE',  ( 0.8831583674551010121, -0.4690749385695646700, 0.000000000000000000 ) ) ;
#13909 = CARTESIAN_POINT ( 'NONE',  ( 24.21182342437587565, 2.662150305148283547, 3.985238629172898950 ) ) ;
#13910 = CARTESIAN_POINT ( 'NONE',  ( 17.34275990732152195, 9.186172967928778021, -2.849824708884751256 ) ) ;
#13911 = DIRECTION ( 'NONE',  ( 1.000000000000000000, 0.000000000000000000, 0.000000000000000000 ) ) ;
#13912 = DIRECTION ( 'NONE',  ( 0.000000000000000000, 0.000000000000000000, -1.000000000000000000 ) ) ;
#13913 = CARTESIAN_POINT ( 'NONE',  ( 22.87846855920513178, 4.336014621590010165, -3.060014917398448553 ) ) ;
#13914 = ORIENTED_EDGE ( 'NONE', *, *, #39934, .F. ) ;
#13915 = FACE_OUTER_BOUND ( 'NONE', #27861, .T. ) ;
#13916 = LINE ( 'NONE', #36157, #26763 ) ;
#13917 = AXIS2_PLACEMENT_3D ( 'NONE', #16246, #18511, #9662 ) ;
#13918 = CARTESIAN_POINT ( 'NONE',  ( -71.75727376073825781, 2.199410611364987389, -9.965632999380227730 ) ) ;
#13919 = CARTESIAN_POINT ( 'NONE',  ( 4.718383115759797519, -27.79743845850708794, 7.737115613922531665 ) ) ;
#13920 = CARTESIAN_POINT ( 'NONE',  ( -1.699583094839331787, -29.58343279012807159, 7.635761828346577573 ) ) ;
#13921 = CARTESIAN_POINT ( 'NONE',  ( 81.28781607649123941, 61.48165154268892252, 1.786209778413323734 ) ) ;
#13922 = CARTESIAN_POINT ( 'NONE',  ( -1.495543489590137165, -30.73010626234981402, 7.769368695748488207 ) ) ;
#13923 = CARTESIAN_POINT ( 'NONE',  ( 3.901581986397568702, -26.97862765183199585, 7.779495906702011965 ) ) ;
#13924 = CARTESIAN_POINT ( 'NONE',  ( -1.276156623011316382, -27.74234360012602352, 7.776484688137388801 ) ) ;
#13925 = DIRECTION ( 'NONE',  ( 0.7660444431189771253, 0.6427876096865405842, -0.000000000000000000 ) ) ;
#13926 = CARTESIAN_POINT ( 'NONE',  ( 4.401417849205680355, -27.34407100962124559, 6.894806418505347700 ) ) ;
#13927 = PLANE ( 'NONE',  #30494 ) ;
#13928 = CARTESIAN_POINT ( 'NONE',  ( 4.176116573831426315, -31.90033323721567271, 6.903372536218459921 ) ) ;
#13929 =( BOUNDED_CURVE ( )  B_SPLINE_CURVE ( 3, ( #5215, #27842, #11980, #8489 ),
 .UNSPECIFIED., .F., .T. ) 
 B_SPLINE_CURVE_WITH_KNOTS ( ( 4, 4 ),
 ( 4.748221474220559735, 4.941946782021393147 ),
 .UNSPECIFIED. ) 
 CURVE ( )  GEOMETRIC_REPRESENTATION_ITEM ( )  RATIONAL_B_SPLINE_CURVE ( ( 1.000000000000000000, 0.9968749865767494445, 0.9968749865767494445, 1.000000000000000000 ) ) 
 REPRESENTATION_ITEM ( '' )  );
#13930 = CARTESIAN_POINT ( 'NONE',  ( 3.858201203583684791, -26.94241211265677194, 7.695279973900954751 ) ) ;
#13931 = CARTESIAN_POINT ( 'NONE',  ( 68.53436546801150087, 58.80600050245282517, 3.985059344218149668 ) ) ;
#13932 = CARTESIAN_POINT ( 'NONE',  ( 27.40694485339065523, 0.9632844686313415394, 4.483914602474418309 ) ) ;
#13933 = EDGE_CURVE ( 'NONE', #27494, #1015, #8387, .T. ) ;
#13934 = VERTEX_POINT ( 'NONE', #28529 ) ;
#13935 = LINE ( 'NONE', #1403, #1706 ) ;
#13937 = ADVANCED_FACE ( 'NONE', ( #31220 ), #9371, .F. ) ;
#13936 = CARTESIAN_POINT ( 'NONE',  ( 85.03556247682649882, 2.841744791465048880, -1.219259102000758821 ) ) ;
#13939 = CARTESIAN_POINT ( 'NONE',  ( -0.4998380263676178714, -26.84796820482366897, 6.870737987065016483 ) ) ;
#13938 = CARTESIAN_POINT ( 'NONE',  ( 78.65282594500106939, 66.03191569515874448, -1.205449537698850326 ) ) ;
#13940 = CARTESIAN_POINT ( 'NONE',  ( 3.791157483716739218, -32.25110375459131973, 7.754798119455333705 ) ) ;
#13941 = CARTESIAN_POINT ( 'NONE',  ( 2.356131281712445791, -26.14680573639735428, 7.785344483711591934 ) ) ;
#13942 = ORIENTED_EDGE ( 'NONE', *, *, #16233, .F. ) ;
#13943 = DIRECTION ( 'NONE',  ( 1.000000000000000000, 0.000000000000000000, -0.000000000000000000 ) ) ;
#13944 = LINE ( 'NONE', #26514, #18125 ) ;
#13945 = ADVANCED_FACE ( 'NONE', ( #28115 ), #18635, .T. ) ;
#13946 = VERTEX_POINT ( 'NONE', #40667 ) ;
#13947 = CARTESIAN_POINT ( 'NONE',  ( -12.44874870218064267, -25.49307895267003587, 6.800000000000000711 ) ) ;
#13948 = EDGE_CURVE ( 'NONE', #37746, #24175, #11747, .T. ) ;
#13949 = EDGE_LOOP ( 'NONE', ( #40654, #8608, #34150, #8824 ) ) ;
#13950 = APPLICATION_CONTEXT ( 'automotive_design' ) ;
#13951 = CARTESIAN_POINT ( 'NONE',  ( 79.49051211673854311, 64.87125159350625836, -3.403428918328330610 ) ) ;
#13952 = CARTESIAN_POINT ( 'NONE',  ( -10.44874870218064089, -26.64985754041175525, 6.800000000000000711 ) ) ;
#13953 = CARTESIAN_POINT ( 'NONE',  ( 80.20530801487242911, 63.82446735998111365, 3.674973878998263999 ) ) ;
#13954 = CARTESIAN_POINT ( 'NONE',  ( 22.13516576602885166, 0.4647494749783319112, 7.195819920971479711 ) ) ;
#13955 = CIRCLE ( 'NONE', #8006, 8.080217238368769372 ) ;
#13956 = AXIS2_PLACEMENT_3D ( 'NONE', #20334, #1238, #13770 ) ;
#13958 = DIRECTION ( 'NONE',  ( 0.000000000000000000, -0.7508067542896625923, -0.6605219282605402364 ) ) ;
#13957 = CARTESIAN_POINT ( 'NONE',  ( -56.74920310314012539, 30.60922821844966180, -3.177981099252243258 ) ) ;
#13959 = CARTESIAN_POINT ( 'NONE',  ( -1.261910041069867372, -27.90116479715461750, 7.703977250142847844 ) ) ;
#13960 = CARTESIAN_POINT ( 'NONE',  ( -64.08758708074093136, 43.62247136636499079, -2.470836091660580713 ) ) ;
#13961 = CARTESIAN_POINT ( 'NONE',  ( 4.250209030067871652, -31.97748039036408230, 7.387053503561884504 ) ) ;
#13962 = CARTESIAN_POINT ( 'NONE',  ( 22.06885602671490432, 5.236225869313073211, -3.280147744283338440 ) ) ;
#13963 = EDGE_LOOP ( 'NONE', ( #4746, #20130, #12294, #35654 ) ) ;
#13964 = CARTESIAN_POINT ( 'NONE',  ( 5.143923624032054498, -30.17768819491086063, 7.767720160662274331 ) ) ;
#13965 = CARTESIAN_POINT ( 'NONE',  ( 21.85643539959777470, 6.775053487808889940, 8.548204544396675431 ) ) ;
#13966 = CARTESIAN_POINT ( 'NONE',  ( 21.69289330443334407, 6.888012688853258680, -2.083760414291091490 ) ) ;
#13967 = CARTESIAN_POINT ( 'NONE',  ( 15.45142765023373421, 8.160991103234476185, 3.484307100729007622 ) ) ;
#13968 = CARTESIAN_POINT ( 'NONE',  ( 4.045228995182856835, -26.97152095390259063, 7.750000000000000888 ) ) ;
#13969 = CARTESIAN_POINT ( 'NONE',  ( 81.43955525001683782, 63.33353925139297047, 3.171364025132952680 ) ) ;
#13970 = CARTESIAN_POINT ( 'NONE',  ( 87.41819985312852737, -0.4314763451276128481, -5.556477619079806196 ) ) ;
#13971 = CARTESIAN_POINT ( 'NONE',  ( -0.5125101069461960313, -26.98863734761392053, 7.693875151218752428 ) ) ;
#13972 = ORIENTED_EDGE ( 'NONE', *, *, #35812, .T. ) ;
#13973 = CARTESIAN_POINT ( 'NONE',  ( 17.09951025371067246, -3.020100718152188612, 2.875190146946546843 ) ) ;
#13974 = DIRECTION ( 'NONE',  ( 0.000000000000000000, -1.000000000000000000, 0.000000000000000000 ) ) ;
#13975 = CARTESIAN_POINT ( 'NONE',  ( 31.37986798448046954, -3.012493565446135779, -5.103985342590017460 ) ) ;
#13976 = CARTESIAN_POINT ( 'NONE',  ( 33.68735618323012204, -3.098775115391426471, -5.464124682821736023 ) ) ;
#13977 = CARTESIAN_POINT ( 'NONE',  ( -36.97867591359219119, -24.55319635012989110, 6.700000000000000178 ) ) ;
#13978 = CARTESIAN_POINT ( 'NONE',  ( 84.10666795971768295, 3.009888640750769451, -0.3126704449478291403 ) ) ;
#13979 = ORIENTED_EDGE ( 'NONE', *, *, #31418, .T. ) ;
#13980 = AXIS2_PLACEMENT_3D ( 'NONE', #35940, #29152, #16978 ) ;
#13981 = CARTESIAN_POINT ( 'NONE',  ( -42.44874870218064444, -26.64985754041175525, 6.700000000000000178 ) ) ;
#13982 = CARTESIAN_POINT ( 'NONE',  ( -1.163435125605633225, -27.73728167763614039, 6.871394612369936539 ) ) ;
#13983 = EDGE_LOOP ( 'NONE', ( #38701, #2668, #35614, #32697 ) ) ;
#13984 = ORIENTED_EDGE ( 'NONE', *, *, #19443, .T. ) ;
#13985 = CARTESIAN_POINT ( 'NONE',  ( 36.13231797942587775, -1.531115809672503492, 5.643701445848282816 ) ) ;
#13986 = CARTESIAN_POINT ( 'NONE',  ( -1.649184783451180136, -30.58499090532986386, 6.941203072598473689 ) ) ;
#13987 = CARTESIAN_POINT ( 'NONE',  ( 33.44795012684379287, -3.712436240568119494, 5.220878576662950188 ) ) ;
#13988 = CARTESIAN_POINT ( 'NONE',  ( 86.83780739659150072, -1.126960070541983550, 5.236682382497662047 ) ) ;
#13989 = EDGE_LOOP ( 'NONE', ( #21002, #26661, #18107, #18404 ) ) ;
#13990 = EDGE_CURVE ( 'NONE', #615, #38890, #33909, .T. ) ;
#13991 = ORIENTED_EDGE ( 'NONE', *, *, #34802, .T. ) ;
#13992 = EDGE_CURVE ( 'NONE', #22597, #17373, #28481, .T. ) ;
#13993 = DIRECTION ( 'NONE',  ( -0.1736481776669340227, 0.9848077530122073542, -0.000000000000000000 ) ) ;
#13994 = CARTESIAN_POINT ( 'NONE',  ( -56.11355572853777574, 30.33753280151830367, -1.575778306538754725 ) ) ;
#13995 = AXIS2_PLACEMENT_3D ( 'NONE', #35950, #38210, #6932 ) ;
#13997 = CARTESIAN_POINT ( 'NONE',  ( 4.281682929012584182, -27.35702998321412593, 7.703977250142848732 ) ) ;
#13996 = CARTESIAN_POINT ( 'NONE',  ( 4.823128680976433103, -27.98926455409796432, 6.961115707816236231 ) ) ;
#13998 = ORIENTED_EDGE ( 'NONE', *, *, #23369, .T. ) ;
#13999 = CARTESIAN_POINT ( 'NONE',  ( 23.16222335850500613, 3.880895066624781009, 3.304975045450427196 ) ) ;
#14000 = CARTESIAN_POINT ( 'NONE',  ( 82.39441792515134466, 64.18328374515905921, -1.882325606869287515 ) ) ;
#14001 = CARTESIAN_POINT ( 'NONE',  ( -1.312586491988795956, -31.35093330168482595, 7.698786668945012401 ) ) ;
#14002 = VERTEX_POINT ( 'NONE', #33547 ) ;
#14004 = CARTESIAN_POINT ( 'NONE',  ( 4.403058967736086515, -27.36916703378302174, 7.785344483711591934 ) ) ;
#14003 = CARTESIAN_POINT ( 'NONE',  ( 0.01005603839840271338, -26.61987263535688797, 7.775108481317159814 ) ) ;
#14005 = CYLINDRICAL_SURFACE ( 'NONE', #24415, 0.1000000000000028644 ) ;
#14006 = CARTESIAN_POINT ( 'NONE',  ( 74.86608108239484238, 61.39286988729297434, 3.912919437578932236 ) ) ;
#14007 = CIRCLE ( 'NONE', #21249, 114.6618724293813898 ) ;
#14008 = CARTESIAN_POINT ( 'NONE',  ( 22.92160100993126548, 2.713958931179029754, -4.448556569055366339 ) ) ;
#14009 = CARTESIAN_POINT ( 'NONE',  ( -64.08758708074093136, 36.43951107221849384, 3.602717568031709394 ) ) ;
#14010 = FACE_OUTER_BOUND ( 'NONE', #31840, .T. ) ;
#14011 = DIRECTION ( 'NONE',  ( -0.6427876096865328126, -0.7660444431189835646, -0.000000000000000000 ) ) ;
#14012 = DIRECTION ( 'NONE',  ( 0.000000000000000000, 0.000000000000000000, 1.000000000000000000 ) ) ;
#14013 = CARTESIAN_POINT ( 'NONE',  ( -51.21549048184568420, -38.28842912540938670, 4.000000000000000000 ) ) ;
#14014 = CARTESIAN_POINT ( 'NONE',  ( 81.16729622508351838, 61.30314466175459387, 1.045986116561637314 ) ) ;
#14015 = CARTESIAN_POINT ( 'NONE',  ( 87.43837438447430088, 0.1427924124619655843, -4.444214939316114332 ) ) ;
#14016 = CARTESIAN_POINT ( 'NONE',  ( 33.14263624204154723, -3.231821542972313388, 5.586707398679605419 ) ) ;
#14017 = CARTESIAN_POINT ( 'NONE',  ( 1.700390093233090871, -29.56993018339339940, 7.800000000000000711 ) ) ;
#14018 = CARTESIAN_POINT ( 'NONE',  ( -71.12440821180588557, -45.61702805680360484, 10.00000000000001066 ) ) ;
#14019 = FACE_OUTER_BOUND ( 'NONE', #31935, .T. ) ;
#14020 = EDGE_LOOP ( 'NONE', ( #21649, #26957, #35140, #13145 ) ) ;
#14021 = AXIS2_PLACEMENT_3D ( 'NONE', #26300, #16800, #7747 ) ;
#14022 = CARTESIAN_POINT ( 'NONE',  ( 0.09322448663572599492, -26.46073943648378091, 6.887547729233691740 ) ) ;
#14023 = CARTESIAN_POINT ( 'NONE',  ( 32.81190345724319002, -0.8379345996357051574, -5.327489112023386930 ) ) ;
#14024 = CARTESIAN_POINT ( 'NONE',  ( 1.651251297819358754, -26.64985754041175525, 6.700000000000000178 ) ) ;
#14025 = DIRECTION ( 'NONE',  ( 0.000000000000000000, 0.000000000000000000, 1.000000000000000000 ) ) ;
#14026 = CARTESIAN_POINT ( 'NONE',  ( -63.70768058868311812, 44.39675795731059793, -1.000000000000000000 ) ) ;
#14027 = VECTOR ( 'NONE', #24023, 1000.000000000000000 ) ;
#14028 = DIRECTION ( 'NONE',  ( 1.000000000000000000, 0.000000000000000000, 0.000000000000000000 ) ) ;
#14029 = CARTESIAN_POINT ( 'NONE',  ( 4.316965410430217531, -31.74099757282072076, 7.748216051605115062 ) ) ;
#14030 = VERTEX_POINT ( 'NONE', #23640 ) ;
#14031 = CARTESIAN_POINT ( 'NONE',  ( 33.66564864975276095, -3.596117103781460766, 5.375233385895072935 ) ) ;
#14032 = DIRECTION ( 'NONE',  ( -1.000000000000000000, 0.000000000000000000, 0.000000000000000000 ) ) ;
#14033 = CARTESIAN_POINT ( 'NONE',  ( 67.70975997764571730, 58.34660981014267378, -3.996132678073276878 ) ) ;
#14034 = CARTESIAN_POINT ( 'NONE',  ( -1.345438465516780369, -27.84570974966549173, 7.660770905198783787 ) ) ;
#14035 = ORIENTED_EDGE ( 'NONE', *, *, #39786, .F. ) ;
#14036 = B_SPLINE_CURVE_WITH_KNOTS ( 'NONE', 3,
 ( #30705, #40149, #5370, #19300, #2511, #31871, #11523, #17908, #14822, #15035 ),
 .UNSPECIFIED., .F., .F.,
 ( 4, 3, 3, 4 ),
 ( 4.982613841084487634E-18, 3.077658087705387998E-05, 6.152638666998344673E-05, 7.730982992130896385E-05 ),
 .UNSPECIFIED. ) ;
#14037 = CARTESIAN_POINT ( 'NONE',  ( -22.44874870218064089, -25.49307895267003587, 6.700000000000000178 ) ) ;
#14039 = EDGE_CURVE ( 'NONE', #462, #5317, #15497, .T. ) ;
#14038 = CARTESIAN_POINT ( 'NONE',  ( 1.736346942945643512, -32.96974004645320377, 7.695279973900954751 ) ) ;
#14040 = CARTESIAN_POINT ( 'NONE',  ( 85.41573320709208872, 1.271949590728955970, -5.602497903006397273 ) ) ;
#14041 = CARTESIAN_POINT ( 'NONE',  ( 4.984671627384348547, -28.36018029005467866, 7.635761828346577573 ) ) ;
#14042 = CARTESIAN_POINT ( 'NONE',  ( 0.4741610271200560334, -32.84809465111302984, 6.894806418505347700 ) ) ;
#14043 = CARTESIAN_POINT ( 'NONE',  ( -1.699178655868960552, -29.51577928193538369, 7.785387725071490905 ) ) ;
#14044 = ORIENTED_EDGE ( 'NONE', *, *, #9204, .F. ) ;
#14045 = CARTESIAN_POINT ( 'NONE',  ( 23.74959400416620170, 3.568744068378384426, 3.161886204904667430 ) ) ;
#14046 = CARTESIAN_POINT ( 'NONE',  ( -70.92837670882107659, 28.72470171467712063, -2.000000000000000000 ) ) ;
#14048 = AXIS2_PLACEMENT_3D ( 'NONE', #7008, #29243, #26161 ) ;
#14047 = CARTESIAN_POINT ( 'NONE',  ( 78.64903117394807452, 66.02922079195218430, 1.215327096190495615 ) ) ;
#14049 = CARTESIAN_POINT ( 'NONE',  ( 30.76629399850509827, -3.583112896957922899, -4.803821987783259750 ) ) ;
#14050 = ORIENTED_EDGE ( 'NONE', *, *, #13426, .T. ) ;
#14051 = CARTESIAN_POINT ( 'NONE',  ( 78.82422632494606773, 64.37263203041347026, -3.536670452273165566 ) ) ;
#14053 = CARTESIAN_POINT ( 'NONE',  ( 5.116398603051176330, -28.77698600466689882, 7.139344958878411695 ) ) ;
#14052 = CARTESIAN_POINT ( 'NONE',  ( 21.99049160266946146, 0.2366918349952460976, 7.677809126247182370 ) ) ;
#14054 = CARTESIAN_POINT ( 'NONE',  ( 80.08603431819594221, 65.58772839307371783, -2.892908819258016795 ) ) ;
#14055 = CARTESIAN_POINT ( 'NONE',  ( 79.45360044721715553, 62.79974527947165797, 3.729426069516725395 ) ) ;
#14056 = VECTOR ( 'NONE', #6727, 1000.000000000000000 ) ;
#14057 = CARTESIAN_POINT ( 'NONE',  ( 35.49282083210901817, -3.770656079430354524, -5.543542841511455599 ) ) ;
#14058 = CARTESIAN_POINT ( 'NONE',  ( 78.69036185089561286, 66.05857758962513060, 1.005837412005772036 ) ) ;
#14059 = DIRECTION ( 'NONE',  ( 0.000000000000000000, 0.000000000000000000, -1.000000000000000000 ) ) ;
#14060 = CARTESIAN_POINT ( 'NONE',  ( 29.97903609306309747, -3.796949753938318128, 3.982659670407546759 ) ) ;
#14061 = EDGE_CURVE ( 'NONE', #15530, #38080, #19236, .T. ) ;
#14062 = CARTESIAN_POINT ( 'NONE',  ( -63.58520484588292732, 35.72026407271199133, -6.999999999999995559 ) ) ;
#14063 = ORIENTED_EDGE ( 'NONE', *, *, #21819, .F. ) ;
#14064 = CARTESIAN_POINT ( 'NONE',  ( -79.05190533785294349, -5.483372927171442868, 5.843910349080737809 ) ) ;
#14065 = CARTESIAN_POINT ( 'NONE',  ( 22.29617236214320641, 0.2616978831331430166, -7.104760123125566373 ) ) ;
#14066 = CARTESIAN_POINT ( 'NONE',  ( -30.97867591359219119, -26.64985754041175525, 6.800000000000000711 ) ) ;
#14067 = ORIENTED_EDGE ( 'NONE', *, *, #31485, .F. ) ;
#14068 = CARTESIAN_POINT ( 'NONE',  ( 5.162379329697287744, -29.05540582370486291, 6.863805608295729499 ) ) ;
#14069 = CARTESIAN_POINT ( 'NONE',  ( 37.18610711987288653, -2.963366855433791525, -5.999999389906995440 ) ) ;
#14070 = PRESENTATION_STYLE_ASSIGNMENT (( #1537 ) ) ;
#14071 = CARTESIAN_POINT ( 'NONE',  ( 3.281363509912449850, -32.69251293742141939, 6.951256099901584662 ) ) ;
#14072 = CARTESIAN_POINT ( 'NONE',  ( -1.053466190009290315, -31.73008655996581595, 6.865482280155370098 ) ) ;
#14073 = DIRECTION ( 'NONE',  ( 1.000000000000000000, -0.000000000000000000, 0.000000000000000000 ) ) ;
#14074 = DIRECTION ( 'NONE',  ( 1.000000000000000000, 0.000000000000000000, 0.000000000000000000 ) ) ;
#14075 = DIRECTION ( 'NONE',  ( 0.9396926207859126468, -0.3420201433256568335, -0.000000000000000000 ) ) ;
#14076 = ADVANCED_FACE ( 'NONE', ( #27137 ), #24040, .F. ) ;
#14077 = LINE ( 'NONE', #23754, #36864 ) ;
#14078 = VERTEX_POINT ( 'NONE', #24249 ) ;
#14079 = VERTEX_POINT ( 'NONE', #14173 ) ;
#14080 = CARTESIAN_POINT ( 'NONE',  ( 66.27376694608996388, 57.73522568913447373, 4.000000000000000000 ) ) ;
#14081 = CARTESIAN_POINT ( 'NONE',  ( 71.87019205445125181, 60.48965333507749165, -3.909340765870004564 ) ) ;
#14082 = VECTOR ( 'NONE', #1695, 1000.000000000000000 ) ;
#14083 = ORIENTED_EDGE ( 'NONE', *, *, #12229, .F. ) ;
#14084 = CARTESIAN_POINT ( 'NONE',  ( 84.47734884986269321, 2.726878650076010491, -2.900369371603537694 ) ) ;
#14086 = EDGE_CURVE ( 'NONE', #36353, #35702, #29318, .T. ) ;
#14085 = CARTESIAN_POINT ( 'NONE',  ( -1.797258899342013549, -29.44812577374269580, 7.754798119455333705 ) ) ;
#14087 = ADVANCED_FACE ( 'NONE', ( #39283 ), #20346, .T. ) ;
#14088 = CARTESIAN_POINT ( 'NONE',  ( 2.140846989427893643, -33.04210496623404225, 7.013842709614101167 ) ) ;
#14089 = APPLICATION_PROTOCOL_DEFINITION ( 'draft international standard', 'automotive_design', 1998, #16583 ) ;
#14090 = CARTESIAN_POINT ( 'NONE',  ( -29.07867591359219617, -24.55319635012989110, 6.800000000000000711 ) ) ;
#14091 = CARTESIAN_POINT ( 'NONE',  ( -38.34874870218063592, -26.64985754041175525, 6.800000000000000711 ) ) ;
#14092 = CARTESIAN_POINT ( 'NONE',  ( -70.92837670882107659, 10.37661300689600097, 0.000000000000000000 ) ) ;
#14093 = ORIENTED_EDGE ( 'NONE', *, *, #19990, .T. ) ;
#14094 = CARTESIAN_POINT ( 'NONE',  ( 79.03665253560640735, 65.17130141867492910, -3.087291694836853395 ) ) ;
#14095 = B_SPLINE_CURVE_WITH_KNOTS ( 'NONE', 3,
 ( #28037, #12394, #24962, #37496, #9293, #21871, #35459, #4161, #29265, #19984, #22890, #35059, #23091, #35656, #1077, #16678, #38715, #26382, #32568, #31963, #23284, #6833, #4557, #10705, #35853, #22695, #38913, #28659, #465, #4364, #16884 ),
 .UNSPECIFIED., .F., .F.,
 ( 4, 3, 3, 3, 3, 3, 3, 3, 3, 3, 4 ),
 ( 6.484403375994724850E-05, 8.983333709522357997E-05, 0.0001203539973219380516, 0.0001514144607149691020, 0.0001828916862241622594, 0.0002144221682127272230, 0.0002455195857862213201, 0.0002758614570916287823, 0.0003055381793602585799, 0.0003350143730643718900, 0.0003497271997307932457 ),
 .UNSPECIFIED. ) ;
#14096 = CARTESIAN_POINT ( 'NONE',  ( 14.51114109149617981, 10.82491507747520387, -2.499999999998495426 ) ) ;
#14097 = CARTESIAN_POINT ( 'NONE',  ( 79.37660656468254672, 64.78470313322952734, 3.432573985763631708 ) ) ;
#14098 = LINE ( 'NONE', #29557, #34877 ) ;
#14099 = EDGE_CURVE ( 'NONE', #14684, #20369, #6954, .T. ) ;
#14100 = AXIS2_PLACEMENT_3D ( 'NONE', #16598, #35380, #28575 ) ;
#14101 = DIRECTION ( 'NONE',  ( 0.000000000000000000, 0.000000000000000000, 1.000000000000000000 ) ) ;
#14102 = CARTESIAN_POINT ( 'NONE',  ( 4.040074159915059582, -27.10297285337844286, 6.929923840112066635 ) ) ;
#14103 = CARTESIAN_POINT ( 'NONE',  ( -17.69482985384421880, -42.37473357531882101, -2.500000000000000000 ) ) ;
#14104 = CARTESIAN_POINT ( 'NONE',  ( 21.85643539959774273, 10.54266624894746229, 1.842303177338921572 ) ) ;
#14105 = DIRECTION ( 'NONE',  ( -0.000000000000000000, -0.000000000000000000, -1.000000000000000000 ) ) ;
#14106 = EDGE_LOOP ( 'NONE', ( #25025, #24376, #4728, #32609 ) ) ;
#14107 = CARTESIAN_POINT ( 'NONE',  ( 77.73210138736416752, 65.38047884209385074, -2.040462881234939907 ) ) ;
#14108 = VECTOR ( 'NONE', #10742, 1000.000000000000000 ) ;
#14109 = CARTESIAN_POINT ( 'NONE',  ( 14.75671739045200326, -5.151268613661418527, 2.500000000000008438 ) ) ;
#14110 = CARTESIAN_POINT ( 'NONE',  ( -75.63216817879452947, -3.684923045591205870, -10.23342513283385635 ) ) ;
#14111 = CARTESIAN_POINT ( 'NONE',  ( -0.4747269484695719743, -32.18314005917732601, 7.635761828346577573 ) ) ;
#14112 = CARTESIAN_POINT ( 'NONE',  ( 34.14251866354382514, -3.850829291023918799, -5.232138609549901176 ) ) ;
#14113 = CARTESIAN_POINT ( 'NONE',  ( 80.70080623961233357, 63.70112813535636320, 3.588566286536278849 ) ) ;
#14114 = CARTESIAN_POINT ( 'NONE',  ( -83.92837670882109080, 2.429809908903242555, 15.50000000000000000 ) ) ;
#14115 = CARTESIAN_POINT ( 'NONE',  ( -75.45330471031414277, 33.71485196875532608, 21.52833696633422988 ) ) ;
#14116 = CARTESIAN_POINT ( 'NONE',  ( -0.08065709997538077214, -26.55697965350343281, 7.695279973900954751 ) ) ;
#14117 = CARTESIAN_POINT ( 'NONE',  ( 31.21728410049454183, -0.3790710272928793922, 5.078610195387921245 ) ) ;
#14118 = ADVANCED_FACE ( 'NONE', ( #4716 ), #33128, .T. ) ;
#14119 = EDGE_CURVE ( 'NONE', #109, #1708, #5276, .T. ) ;
#14120 = ADVANCED_FACE ( 'NONE', ( #33741 ), #32925, .F. ) ;
#14121 = CARTESIAN_POINT ( 'NONE',  ( 3.967042426631197216, -32.23682145114030817, 7.743886751744254227 ) ) ;
#14122 = CARTESIAN_POINT ( 'NONE',  ( 87.15742208552646275, 0.4583713694408729777, 4.797783382239512839 ) ) ;
#14123 = CARTESIAN_POINT ( 'NONE',  ( 4.256963712960452284, -31.81136415787042537, 6.874555630061438549 ) ) ;
#14124 = CARTESIAN_POINT ( 'NONE',  ( 2.277526804980155362, -33.02201842327861669, 6.894806418505347700 ) ) ;
#14125 = CARTESIAN_POINT ( 'NONE',  ( 68.11537257328342321, 58.15040817571434673, 3.985705108533863505 ) ) ;
#14126 = CARTESIAN_POINT ( 'NONE',  ( 34.33392167688137420, -1.483023185420157430, 5.565036865347550155 ) ) ;
#14127 = AXIS2_PLACEMENT_3D ( 'NONE', #23261, #10285, #3739 ) ;
#14128 = CARTESIAN_POINT ( 'NONE',  ( -64.08758708074093136, 42.48851732804387638, -2.660621167144407995 ) ) ;
#14129 = CIRCLE ( 'NONE', #1035, 31.65266504832700534 ) ;
#14130 = CARTESIAN_POINT ( 'NONE',  ( 85.64504565501374600, 2.098084819171330828, -4.577105872335450520 ) ) ;
#14132 = CARTESIAN_POINT ( 'NONE',  ( 1.669309969508061764, -33.06979218437418666, 6.894806418505347700 ) ) ;
#14131 = CARTESIAN_POINT ( 'NONE',  ( 78.73074668855629454, 66.04592173387707987, -1.531260274641971675 ) ) ;
#14133 = DIRECTION ( 'NONE',  ( 1.385724075720358314E-16, -1.000000000000000000, 0.000000000000000000 ) ) ;
#14134 = CARTESIAN_POINT ( 'NONE',  ( -1.236334162535101644, -27.66580709588378539, 6.998987538705434552 ) ) ;
#14135 = CARTESIAN_POINT ( 'NONE',  ( -59.46024017484869972, 26.94883531126005849, 5.502890977078418011 ) ) ;
#14136 = EDGE_LOOP ( 'NONE', ( #32276, #26455, #6793, #16626, #7293 ) ) ;
#14137 = DIRECTION ( 'NONE',  ( -0.000000000000000000, -0.000000000000000000, -1.000000000000000000 ) ) ;
#14138 = CARTESIAN_POINT ( 'NONE',  ( 4.874192403021982756, -30.78934762560861671, 7.785172627573962778 ) ) ;
#14139 = VECTOR ( 'NONE', #16379, 1000.000000000000000 ) ;
#14140 = ORIENTED_EDGE ( 'NONE', *, *, #5684, .F. ) ;
#14141 = CARTESIAN_POINT ( 'NONE',  ( -71.64402667994158946, -21.49031309831630665, 3.957576123060442708 ) ) ;
#14142 = VERTEX_POINT ( 'NONE', #5522 ) ;
#14143 = B_SPLINE_CURVE_WITH_KNOTS ( 'NONE', 3,
 ( #13799, #33145, #24470, #39917, #5135, #2686, #14789, #30250 ),
 .UNSPECIFIED., .F., .F.,
 ( 4, 2, 2, 4 ),
 ( -2.112996879340024923E-05, 0.0001977261364128406966, 0.0004165822416190816525, 0.0008542944520315643234 ),
 .UNSPECIFIED. ) ;
#14144 = ORIENTED_EDGE ( 'NONE', *, *, #24687, .F. ) ;
#14145 = CARTESIAN_POINT ( 'NONE',  ( 79.09343976728325742, 65.54176476638896531, -2.787474064117370975 ) ) ;
#14146 = LINE ( 'NONE', #16433, #22070 ) ;
#14147 = CARTESIAN_POINT ( 'NONE',  ( 79.73292928667240176, 64.66788176856890402, 3.497296750721718084 ) ) ;
#14148 = CARTESIAN_POINT ( 'NONE',  ( 23.14899473699292898, 0.4583984410259172027, 5.838797680875789098 ) ) ;
#14150 = ORIENTED_EDGE ( 'NONE', *, *, #36080, .T. ) ;
#14149 = CARTESIAN_POINT ( 'NONE',  ( 4.727238272722242840, -27.81534140858726900, 7.762796336881262249 ) ) ;
#14151 = ADVANCED_FACE ( 'NONE', ( #27547 ), #30654, .F. ) ;
#14152 = DIRECTION ( 'NONE',  ( 0.4826092789263659033, -0.5751513419797880111, -0.6605219282605402364 ) ) ;
#14154 = CARTESIAN_POINT ( 'NONE',  ( 1.062037487868057184, -33.01122440958558002, 6.894806418505347700 ) ) ;
#14153 = CARTESIAN_POINT ( 'NONE',  ( -51.01549048184568846, -30.38627270959228710, 6.800000000000000711 ) ) ;
#14155 = CARTESIAN_POINT ( 'NONE',  ( -0.7996099067669091287, -29.56993018339339940, -15.49999999999999822 ) ) ;
#14156 = LINE ( 'NONE', #26730, #12692 ) ;
#14157 = CARTESIAN_POINT ( 'NONE',  ( 22.47233723954558471, 4.599796910044377185, -3.286792849618373147 ) ) ;
#14158 = VERTEX_POINT ( 'NONE', #26744 ) ;
#14159 = CARTESIAN_POINT ( 'NONE',  ( 5.121105927283316817, -30.24177255004237352, 7.784725160561910329 ) ) ;
#14160 = EDGE_CURVE ( 'NONE', #23979, #13676, #27879, .T. ) ;
#14161 = CIRCLE ( 'NONE', #16803, 0.1000000000000028644 ) ;
#14162 = CARTESIAN_POINT ( 'NONE',  ( 22.34899403049013245, 4.475801132629629642, -6.347516269785208998 ) ) ;
#14163 = AXIS2_PLACEMENT_3D ( 'NONE', #16877, #20370, #30059 ) ;
#14164 = EDGE_CURVE ( 'NONE', #14484, #4585, #2389, .T. ) ;
#14165 = CARTESIAN_POINT ( 'NONE',  ( 17.60335251145751911, 11.93951241251601658, 2.500000000000000444 ) ) ;
#14166 = ORIENTED_EDGE ( 'NONE', *, *, #8349, .F. ) ;
#14167 = CARTESIAN_POINT ( 'NONE',  ( 1.113415308591769737, -33.02035961353927718, 7.744938106820260515 ) ) ;
#14168 = CARTESIAN_POINT ( 'NONE',  ( 80.08603431818187346, 65.58772839306588764, 2.892908819267548282 ) ) ;
#14169 = CARTESIAN_POINT ( 'NONE',  ( 88.07792789432249947, -1.225918755007668226, 4.438991276806098618 ) ) ;
#14170 =( BOUNDED_CURVE ( )  B_SPLINE_CURVE ( 3, ( #1381, #32271, #16585, #32462 ),
 .UNSPECIFIED., .F., .T. ) 
 B_SPLINE_CURVE_WITH_KNOTS ( ( 4, 4 ),
 ( 1.381924640371169133, 1.574767692156078036 ),
 .UNSPECIFIED. ) 
 CURVE ( )  GEOMETRIC_REPRESENTATION_ITEM ( )  RATIONAL_B_SPLINE_CURVE ( ( 1.000000000000000000, 0.9969033633783032089, 0.9969033633783032089, 1.000000000000000000 ) ) 
 REPRESENTATION_ITEM ( '' )  );
#14171 = DIRECTION ( 'NONE',  ( 1.000000000000000000, 0.000000000000000000, 0.000000000000000000 ) ) ;
#14172 = EDGE_LOOP ( 'NONE', ( #36010, #13193, #6978, #31277 ) ) ;
#14173 = CARTESIAN_POINT ( 'NONE',  ( -0.4487487021806388365, -26.64985754041175525, 6.700000000000000178 ) ) ;
#14174 = AXIS2_PLACEMENT_3D ( 'NONE', #8967, #21964, #5902 ) ;
#14175 = ADVANCED_FACE ( 'NONE', ( #17653 ), #2048, .F. ) ;
#14176 = CARTESIAN_POINT ( 'NONE',  ( 5.060761980011518446, -29.05224715530099999, 6.874555630061443878 ) ) ;
#14177 = CARTESIAN_POINT ( 'NONE',  ( 21.50439050508445149, -2.639863281018423269, -3.562678242604879753 ) ) ;
#14178 = CARTESIAN_POINT ( 'NONE',  ( 36.78868941511550616, -3.039652253131195803, -5.948162739681252198 ) ) ;
#14179 = CARTESIAN_POINT ( 'NONE',  ( 0.4741610271200560334, -32.84809465111302984, 6.894806418505347700 ) ) ;
#14180 = CARTESIAN_POINT ( 'NONE',  ( 25.79188176699440760, 1.042700297243206009, -4.433481499727591313 ) ) ;
#14181 = DIRECTION ( 'NONE',  ( -0.000000000000000000, 1.000000000000000000, -0.000000000000000000 ) ) ;
#14182 = EDGE_LOOP ( 'NONE', ( #39099, #27632, #15409, #30044, #18503, #7416 ) ) ;
#14183 = CARTESIAN_POINT ( 'NONE',  ( 37.04507163839541306, -2.801180510112711186, 5.988177386251506640 ) ) ;
#14184 = DIRECTION ( 'NONE',  ( 1.000000000000000000, 0.000000000000000000, 0.000000000000000000 ) ) ;
#14185 = CARTESIAN_POINT ( 'NONE',  ( -1.190803463164421094, -27.78076534723357582, 6.864651958020304257 ) ) ;
#14186 = VERTEX_POINT ( 'NONE', #16012 ) ;
#14187 = ORIENTED_EDGE ( 'NONE', *, *, #11318, .F. ) ;
#14188 = CARTESIAN_POINT ( 'NONE',  ( 37.01009445965782874, -2.248872324984072080, 5.912996221296350718 ) ) ;
#14189 = CARTESIAN_POINT ( 'NONE',  ( -0.5358931834503292135, -32.26233439484389010, 7.640616322432101093 ) ) ;
#14190 = CARTESIAN_POINT ( 'NONE',  ( 66.27376694609004915, 57.73522568913436004, -4.000000000000000000 ) ) ;
#14191 = CARTESIAN_POINT ( 'NONE',  ( 86.30432403813082942, -0.2980101775014994958, 5.888268584329271249 ) ) ;
#14192 = ORIENTED_EDGE ( 'NONE', *, *, #26657, .F. ) ;
#14193 = CIRCLE ( 'NONE', #12885, 0.9999999999999998890 ) ;
#14194 = ORIENTED_EDGE ( 'NONE', *, *, #26487, .F. ) ;
#14195 = AXIS2_PLACEMENT_3D ( 'NONE', #13152, #31491, #6581 ) ;
#14196 = CARTESIAN_POINT ( 'NONE',  ( 5.144146178010085890, -28.94499496390147186, 7.750000000000002665 ) ) ;
#14197 = ORIENTED_EDGE ( 'NONE', *, *, #854, .F. ) ;
#14198 = DIRECTION ( 'NONE',  ( 0.000000000000000000, 0.000000000000000000, -1.000000000000000000 ) ) ;
#14199 = EDGE_LOOP ( 'NONE', ( #6405, #24662, #11389, #2189 ) ) ;
#14200 = CARTESIAN_POINT ( 'NONE',  ( 24.12618649232457102, 3.044573673447521500, 3.674781211205538689 ) ) ;
#14201 = VECTOR ( 'NONE', #7690, 1000.000000000000000 ) ;
#14202 = CARTESIAN_POINT ( 'NONE',  ( 81.41940809751206132, 61.44195378529067852, -1.227604746834842553 ) ) ;
#14203 = CARTESIAN_POINT ( 'NONE',  ( -1.237321756456247979, -31.28161037787917209, 7.635761828346577573 ) ) ;
#14204 = VERTEX_POINT ( 'NONE', #6557 ) ;
#14206 = DIRECTION ( 'NONE',  ( 1.000000000000000000, 0.000000000000000000, 0.000000000000000000 ) ) ;
#14205 = CARTESIAN_POINT ( 'NONE',  ( 0.04414393643251195848, -26.60059526728241863, 7.785868773668302545 ) ) ;
#14207 = DIRECTION ( 'NONE',  ( 0.000000000000000000, 0.000000000000000000, 1.000000000000000000 ) ) ;
#14208 = CARTESIAN_POINT ( 'NONE',  ( 75.63732367802946044, 59.67466586216193036, 3.300071129360657718 ) ) ;
#14209 = VERTEX_POINT ( 'NONE', #25085 ) ;
#14210 = CARTESIAN_POINT ( 'NONE',  ( 23.09589271538837352, 2.967069001993269506, -4.168098669102857201 ) ) ;
#14211 = DIRECTION ( 'NONE',  ( 1.000000000000000000, -0.000000000000000000, 0.000000000000000000 ) ) ;
#14212 = DIRECTION ( 'NONE',  ( 1.000000000000000000, 0.000000000000000000, 0.000000000000000000 ) ) ;
#14213 = DIRECTION ( 'NONE',  ( -0.000000000000000000, -0.000000000000000000, -1.000000000000000000 ) ) ;
#14214 = DIRECTION ( 'NONE',  ( 0.000000000000000000, 0.000000000000000000, -1.000000000000000000 ) ) ;
#14215 = CYLINDRICAL_SURFACE ( 'NONE', #9652, 3.499999999999999556 ) ;
#14216 = CARTESIAN_POINT ( 'NONE',  ( 81.23963933823235095, 65.14454330635810209, 2.817575383041586168 ) ) ;
#14217 = CARTESIAN_POINT ( 'NONE',  ( 86.81546468666313388, 0.8424741501213859340, -5.177899619954967392 ) ) ;
#14218 = CARTESIAN_POINT ( 'NONE',  ( 33.69128717328723610, -4.440785898112559416, 4.348130384999381981 ) ) ;
#14219 = DIRECTION ( 'NONE',  ( -0.5000000000000039968, 0.8660254037844363761, -0.000000000000000000 ) ) ;
#14220 = CARTESIAN_POINT ( 'NONE',  ( 4.662059713662509708, -31.23981618828790374, 7.712764235869101981 ) ) ;
#14221 = EDGE_CURVE ( 'NONE', #36180, #29402, #22212, .T. ) ;
#14222 = EDGE_CURVE ( 'NONE', #38011, #18554, #29455, .T. ) ;
#14223 = CARTESIAN_POINT ( 'NONE',  ( -75.55143765322812044, -3.604765552797612571, -10.26479841964585127 ) ) ;
#14224 = CARTESIAN_POINT ( 'NONE',  ( 4.163022776446456241, -25.19622345277205966, 7.695279973900954751 ) ) ;
#14225 = CARTESIAN_POINT ( 'NONE',  ( -81.07947155388370675, 30.81399289130170871, -9.800414904976365804 ) ) ;
#14226 = ADVANCED_FACE ( 'NONE', ( #15812 ), #31671, .T. ) ;
#14227 = CARTESIAN_POINT ( 'NONE',  ( 36.91755608882559159, -3.049047347627591886, -5.968275500765976460 ) ) ;
#14228 =( NAMED_UNIT ( * ) PLANE_ANGLE_UNIT ( ) SI_UNIT ( $, .RADIAN. ) );
#14229 = FACE_OUTER_BOUND ( 'NONE', #1991, .T. ) ;
#14230 = CARTESIAN_POINT ( 'NONE',  ( -1.548822507116328184, -28.29671509637249827, 7.780491323090174660 ) ) ;
#14231 = AXIS2_PLACEMENT_3D ( 'NONE', #472, #35068, #13013 ) ;
#14232 = CARTESIAN_POINT ( 'NONE',  ( 5.252969295392960092, -25.75565214092510047, 6.894806418505347700 ) ) ;
#14233 = EDGE_LOOP ( 'NONE', ( #22355, #22166, #19322, #35538 ) ) ;
#14234 = CARTESIAN_POINT ( 'NONE',  ( 36.34368568239760577, -1.915824052793491328, 5.836657992818942375 ) ) ;
#14235 = CARTESIAN_POINT ( 'NONE',  ( -70.81198565705318515, 0.2164538760997103128, 6.011900603202949611 ) ) ;
#14236 = CARTESIAN_POINT ( 'NONE',  ( 67.44728384595320847, 58.15801736331750504, -3.998402061830689025 ) ) ;
#14237 = CARTESIAN_POINT ( 'NONE',  ( 5.039926880157825195, -30.20828278875847062, 6.894806418505346812 ) ) ;
#14238 = ORIENTED_EDGE ( 'NONE', *, *, #34163, .F. ) ;
#14239 = CARTESIAN_POINT ( 'NONE',  ( -0.5309917997555131386, -32.13526346537501865, 7.785172627573962778 ) ) ;
#14240 = CARTESIAN_POINT ( 'NONE',  ( 86.01948820964511810, 0.2178104211941651880, -5.999583529693873984 ) ) ;
#14241 = CARTESIAN_POINT ( 'NONE',  ( 78.42699581646675711, 65.87166649608005287, 1.555834701912668150 ) ) ;
#14242 = CARTESIAN_POINT ( 'NONE',  ( 1.059624283225857999, -32.90900568614345190, 6.892063359921933419 ) ) ;
#14243 = CARTESIAN_POINT ( 'NONE',  ( 0.3399341882483242760, -32.79470409825933785, 7.006248344249653925 ) ) ;
#14244 = CARTESIAN_POINT ( 'NONE',  ( 1.261915996905217163, -26.09750387580824693, 7.011627023500182965 ) ) ;
#14245 = ORIENTED_EDGE ( 'NONE', *, *, #22243, .T. ) ;
#14246 = CARTESIAN_POINT ( 'NONE',  ( 22.87844296631609353, 4.332290514531911718, 3.065998780651157052 ) ) ;
#14247 = CARTESIAN_POINT ( 'NONE',  ( -1.743365991543899485, -30.19486540288534826, 7.750000000000001776 ) ) ;
#14248 = CARTESIAN_POINT ( 'NONE',  ( 81.15585419290071911, 61.98190721255070201, 2.710038060602456778 ) ) ;
#14249 = VECTOR ( 'NONE', #3132, 1000.000000000000000 ) ;
#14250 = CARTESIAN_POINT ( 'NONE',  ( 11.65737507970504616, -30.94667987854474234, 6.800000000000000711 ) ) ;
#14251 = ORIENTED_EDGE ( 'NONE', *, *, #496, .F. ) ;
#14252 = CARTESIAN_POINT ( 'NONE',  ( 78.04063183619210520, 64.12728436294460721, -3.505091495581006189 ) ) ;
#14254 = CARTESIAN_POINT ( 'NONE',  ( 14.77475711260441393, -5.167191994590148774, -2.499999999999999556 ) ) ;
#14253 = CARTESIAN_POINT ( 'NONE',  ( 24.74313392016376412, 0.5480228596914666905, 4.780878997086071003 ) ) ;
#14255 = AXIS2_PLACEMENT_3D ( 'NONE', #6878, #28494, #15526 ) ;
#14256 = CARTESIAN_POINT ( 'NONE',  ( 81.40528610411905674, 61.52959015154601019, -1.692865493181702430 ) ) ;
#14257 = CARTESIAN_POINT ( 'NONE',  ( 79.57354641881573798, 61.78191946445392801, 3.317372267376139217 ) ) ;
#14258 = CIRCLE ( 'NONE', #24802, 2.500000000000000444 ) ;
#14259 = ORIENTED_EDGE ( 'NONE', *, *, #26429, .F. ) ;
#14260 = AXIS2_PLACEMENT_3D ( 'NONE', #3493, #16017, #17767 ) ;
#14261 = CARTESIAN_POINT ( 'NONE',  ( -0.9247287804614536810, -27.40920093173490102, 7.721096864323897080 ) ) ;
#14262 = CARTESIAN_POINT ( 'NONE',  ( 82.38651420471397557, 62.84168609110421500, 1.553473047276233476 ) ) ;
#14263 = CARTESIAN_POINT ( 'NONE',  ( 82.38753728249152175, 5.816132372599501110, -6.000000000000000888 ) ) ;
#14264 = CARTESIAN_POINT ( 'NONE',  ( 26.59415400691353071, 2.826550869980146707, -2.084159418869949043 ) ) ;
#14265 = CARTESIAN_POINT ( 'NONE',  ( -64.37872067649583130, 36.58503142451505141, -5.660009492437820811 ) ) ;
#14266 = ORIENTED_EDGE ( 'NONE', *, *, #11598, .T. ) ;
#14267 = DIRECTION ( 'NONE',  ( 0.6427876096865379196, 0.7660444431189793457, -0.000000000000000000 ) ) ;
#14268 = CARTESIAN_POINT ( 'NONE',  ( 21.73396179380037552, 0.2160579277391266595, -9.105503571107611549 ) ) ;
#14269 = VERTEX_POINT ( 'NONE', #384 ) ;
#14270 = B_SPLINE_CURVE_WITH_KNOTS ( 'NONE', 3,
 ( #20000, #3981, #35870, #23104, #32582, #16307, #13829, #38524, #13222, #16692 ),
 .UNSPECIFIED., .F., .F.,
 ( 4, 2, 2, 2, 4 ),
 ( 0.000000000000000000, 0.0003911417017416533534, 0.0007822834034833067067, 0.001173425105224960114, 0.001564566806966613413 ),
 .UNSPECIFIED. ) ;
#14271 = CARTESIAN_POINT ( 'NONE',  ( 5.163932268927621472, -29.06596534262345699, 6.863784140767622333 ) ) ;
#14272 = ADVANCED_FACE ( 'NONE', ( #2669 ), #15603, .T. ) ;
#14273 = EDGE_LOOP ( 'NONE', ( #15186, #5366, #11063, #14688 ) ) ;
#14274 = CARTESIAN_POINT ( 'NONE',  ( 36.44373137833709109, -1.735229189699011743, -5.732540015342363127 ) ) ;
#14275 = CARTESIAN_POINT ( 'NONE',  ( 3.398405180618411237, -32.61369795523508230, 7.785344483711591934 ) ) ;
#14276 = CARTESIAN_POINT ( 'NONE',  ( 3.307555699830478702, -32.67912093030300014, 6.887547729233684635 ) ) ;
#14277 = CARTESIAN_POINT ( 'NONE',  ( -1.047142997612213078, -31.73814762596163064, 6.863784140767623221 ) ) ;
#14278 = DIRECTION ( 'NONE',  ( 1.000000000000000000, 0.000000000000000000, 0.000000000000000000 ) ) ;
#14279 = CARTESIAN_POINT ( 'NONE',  ( 3.551251297819357777, -26.64985754041175525, 6.700000000000000178 ) ) ;
#14280 = CARTESIAN_POINT ( 'NONE',  ( 5.093905639142482400, -29.77981643751997964, 6.959317978105170610 ) ) ;
#14281 = CARTESIAN_POINT ( 'NONE',  ( 4.437609036105186533, -27.54124898828658630, 7.386948897581451234 ) ) ;
#14282 = VERTEX_POINT ( 'NONE', #25289 ) ;
#14283 =( BOUNDED_CURVE ( )  B_SPLINE_CURVE ( 3, ( #39818, #10437, #20107, #17973 ),
 .UNSPECIFIED., .F., .F. ) 
 B_SPLINE_CURVE_WITH_KNOTS ( ( 4, 4 ),
 ( 1.381924640371168467, 1.574767692156076260 ),
 .UNSPECIFIED. ) 
 CURVE ( )  GEOMETRIC_REPRESENTATION_ITEM ( )  RATIONAL_B_SPLINE_CURVE ( ( 1.000000000000000000, 0.9969033633783033199, 0.9969033633783033199, 1.000000000000000000 ) ) 
 REPRESENTATION_ITEM ( '' )  );
#14284 = CARTESIAN_POINT ( 'NONE',  ( 66.27376694608996388, 57.73522568913447373, 4.000000000000000000 ) ) ;
#14285 = B_SPLINE_CURVE_WITH_KNOTS ( 'NONE', 3,
 ( #10321, #4757, #38723, #16894, #17291, #36254, #29869, #7239, #39329, #4171 ),
 .UNSPECIFIED., .F., .F.,
 ( 4, 3, 3, 4 ),
 ( 0.000000000000000000, 3.025505781527817344E-05, 6.051003801291506945E-05, 6.468145402690557617E-05 ),
 .UNSPECIFIED. ) ;
#14286 = CARTESIAN_POINT ( 'NONE',  ( 71.91282362819097784, 60.38839763785598080, -3.929231508849751364 ) ) ;
#14287 = AXIS2_PLACEMENT_3D ( 'NONE', #956, #13491, #19872 ) ;
#14288 = EDGE_LOOP ( 'NONE', ( #33096, #12378, #37243, #28346 ) ) ;
#14289 = CARTESIAN_POINT ( 'NONE',  ( 87.90619863186083194, -2.144287391213948624, -2.780224877855328014 ) ) ;
#14290 = CARTESIAN_POINT ( 'NONE',  ( -60.36144324275490902, 24.84364830758653397, 8.926047827505314558 ) ) ;
#14291 = CARTESIAN_POINT ( 'NONE',  ( -0.8982326133871421092, -27.22530497104394343, 6.867199677474200570 ) ) ;
#14292 = ADVANCED_FACE ( 'NONE', ( #9212 ), #34576, .T. ) ;
#14293 = DIRECTION ( 'NONE',  ( 1.000000000000000000, 0.000000000000000000, 0.000000000000000000 ) ) ;
#14294 = FACE_OUTER_BOUND ( 'NONE', #14586, .T. ) ;
#14295 = FACE_OUTER_BOUND ( 'NONE', #2890, .T. ) ;
#14296 = CARTESIAN_POINT ( 'NONE',  ( -1.752498985642891860, -28.99760421947165057, 7.685194954629195330 ) ) ;
#14297 = EDGE_LOOP ( 'NONE', ( #16430, #6831, #22586, #18652 ) ) ;
#14298 = CARTESIAN_POINT ( 'NONE',  ( 79.98243830041433000, 63.02105934045280833, -3.686141857899485341 ) ) ;
#14299 = CARTESIAN_POINT ( 'NONE',  ( 16.08591502891163572, 7.879342335236748873, -3.484773916741195965 ) ) ;
#14300 = CARTESIAN_POINT ( 'NONE',  ( 79.93741260258519787, 63.33597468792986973, 3.730195463674649048 ) ) ;
#14301 = CARTESIAN_POINT ( 'NONE',  ( 0.6527267737179240914, -26.33536660093865578, 7.754798119455333705 ) ) ;
#14302 = EDGE_CURVE ( 'NONE', #27373, #24427, #179, .T. ) ;
#14303 = CARTESIAN_POINT ( 'NONE',  ( -4.444218661349752963, -35.94265729135299381, -6.000000000000000000 ) ) ;
#14304 = CARTESIAN_POINT ( 'NONE',  ( 4.030793147055388381, -27.09420370279508816, 6.903372536218459032 ) ) ;
#14305 = CARTESIAN_POINT ( 'NONE',  ( 20.16773313137984758, 11.18254505362385132, 2.500000000000000000 ) ) ;
#14306 = CARTESIAN_POINT ( 'NONE',  ( 21.85643539959777826, -3.868027658932458479, -14.06783426539529458 ) ) ;
#14307 = VECTOR ( 'NONE', #20991, 1000.000000000000000 ) ;
#14308 = CARTESIAN_POINT ( 'NONE',  ( 22.61512373101874118, 4.622147853589440913, -3.046406503706223567 ) ) ;
#14309 = ORIENTED_EDGE ( 'NONE', *, *, #36356, .T. ) ;
#14310 = CARTESIAN_POINT ( 'NONE',  ( -77.75226058499177384, 9.861553516275824549, 8.926870939310843411 ) ) ;
#14311 = CARTESIAN_POINT ( 'NONE',  ( 14.76739534775846074, -5.162396215499652996, 2.500000000000008438 ) ) ;
#14312 = CARTESIAN_POINT ( 'NONE',  ( -77.74832814377666068, 9.864871290048851549, -8.937781199387956121 ) ) ;
#14313 = ADVANCED_FACE ( 'NONE', ( #28155 ), #18270, .F. ) ;
#14314 = CARTESIAN_POINT ( 'NONE',  ( -0.3903772972505400451, -26.88875661219547553, 7.754798119455333705 ) ) ;
#14315 = CARTESIAN_POINT ( 'NONE',  ( 2.343738134713599486, -26.23135099740764531, 6.889465824494255486 ) ) ;
#14316 = CARTESIAN_POINT ( 'NONE',  ( 81.32346312764153140, 61.65804850752792987, 2.069468987430086226 ) ) ;
#14317 = DIRECTION ( 'NONE',  ( 0.9848077530122103518, -0.1736481776669172583, -0.000000000000000000 ) ) ;
#14318 = DIRECTION ( 'NONE',  ( 1.000000000000000000, -0.000000000000000000, 0.000000000000000000 ) ) ;
#14319 = CARTESIAN_POINT ( 'NONE',  ( -0.08065709997537935660, -26.55697965350343281, 7.686927408461904143 ) ) ;
#14320 = CARTESIAN_POINT ( 'NONE',  ( 0.6123814071172324347, -26.24333476180446567, 6.865482280155368322 ) ) ;
#14321 = DIRECTION ( 'NONE',  ( -0.000000000000000000, -0.000000000000000000, -1.000000000000000000 ) ) ;
#14322 = CARTESIAN_POINT ( 'NONE',  ( 1.106838199985236137, -33.01923402788369799, 7.636816916992232862 ) ) ;
#14323 = CARTESIAN_POINT ( 'NONE',  ( 4.222957656326197906, -31.84957092882903495, 6.863904403958576594 ) ) ;
#14324 = CARTESIAN_POINT ( 'NONE',  ( -51.01549048184568846, -38.28842912540938670, 6.000000000000000000 ) ) ;
#14325 = CARTESIAN_POINT ( 'NONE',  ( 68.01940210501214779, 58.40717514567135282, 3.996230182412886744 ) ) ;
#14326 = CARTESIAN_POINT ( 'NONE',  ( 36.81793901403195690, -2.525225168568379974, 5.952727846996393346 ) ) ;
#14327 = EDGE_CURVE ( 'NONE', #3514, #26672, #14743, .T. ) ;
#14328 = CARTESIAN_POINT ( 'NONE',  ( 2.239018498799941082, -33.01413523298945307, 7.784725160561910329 ) ) ;
#14329 = CARTESIAN_POINT ( 'NONE',  ( 85.56873805237422914, 2.242856678970356565, 3.827793690346343869 ) ) ;
#14331 = CARTESIAN_POINT ( 'NONE',  ( 31.16512824583443475, -0.3608391175596852296, -5.070470012874099375 ) ) ;
#14330 = CARTESIAN_POINT ( 'NONE',  ( 78.84693035237090442, 66.01116107573028557, -1.842213953838235163 ) ) ;
#14332 = CARTESIAN_POINT ( 'NONE',  ( -1.610170960295353781, -28.79519250847841150, 6.895222827070023541 ) ) ;
#14333 = EDGE_CURVE ( 'NONE', #12043, #32308, #21634, .T. ) ;
#14334 = CARTESIAN_POINT ( 'NONE',  ( -58.78362175692702607, 29.48419490076549465, 5.741263644839468938 ) ) ;
#14335 = ORIENTED_EDGE ( 'NONE', *, *, #12981, .F. ) ;
#14336 = CARTESIAN_POINT ( 'NONE',  ( -0.6858270280168272670, -32.13039545693963106, 6.912143950357345190 ) ) ;
#14337 = CIRCLE ( 'NONE', #20257, 0.1000000000000028644 ) ;
#14338 = ORIENTED_EDGE ( 'NONE', *, *, #9779, .F. ) ;
#14339 = CARTESIAN_POINT ( 'NONE',  ( 78.79145472225366120, 65.75511795602321286, -2.294512580621462572 ) ) ;
#14340 = EDGE_CURVE ( 'NONE', #33808, #14142, #33892, .T. ) ;
#14341 = LINE ( 'NONE', #11244, #29923 ) ;
#14342 = EDGE_CURVE ( 'NONE', #8717, #39757, #14161, .T. ) ;
#14343 = CARTESIAN_POINT ( 'NONE',  ( 78.58771539371637971, 65.98568759316006549, 1.340350474428749106 ) ) ;
#14344 = CARTESIAN_POINT ( 'NONE',  ( 22.53023701225289344, 0.9678367267434657695, 6.208473668897325659 ) ) ;
#14346 = VERTEX_POINT ( 'NONE', #6950 ) ;
#14345 = CARTESIAN_POINT ( 'NONE',  ( -0.7841952061120170958, -27.24896036044557945, 6.887945620086121323 ) ) ;
#14347 = EDGE_CURVE ( 'NONE', #28596, #19820, #30444, .T. ) ;
#14348 = CARTESIAN_POINT ( 'NONE',  ( 75.40715271138134312, 60.19559828969859439, -3.661998389317127511 ) ) ;
#14349 = CARTESIAN_POINT ( 'NONE',  ( 3.229767211660741655, -32.60654106225653948, 6.903372536218458144 ) ) ;
#14350 = AXIS2_PLACEMENT_3D ( 'NONE', #36654, #28920, #23293 ) ;
#14351 = CIRCLE ( 'NONE', #18296, 117.6618724293813898 ) ;
#14353 = CARTESIAN_POINT ( 'NONE',  ( -1.228758070621239762, -27.64172748556450543, 7.387053503561887169 ) ) ;
#14352 = DIRECTION ( 'NONE',  ( 1.000000000000000000, 0.000000000000000000, 0.000000000000000000 ) ) ;
#14354 = FACE_OUTER_BOUND ( 'NONE', #21118, .T. ) ;
#14355 = CARTESIAN_POINT ( 'NONE',  ( 4.662674093641094863, -31.23872421060049831, 7.692469944509195301 ) ) ;
#14356 = CARTESIAN_POINT ( 'NONE',  ( 24.39979727116465114, 2.957582978230396176, -3.694537854723473735 ) ) ;
#14357 = ORIENTED_EDGE ( 'NONE', *, *, #3948, .T. ) ;
#14358 = CARTESIAN_POINT ( 'NONE',  ( -1.749609906766908640, -29.56993018339339940, 6.850000000000000533 ) ) ;
#14359 = CARTESIAN_POINT ( 'NONE',  ( 22.82155563815204502, -7.011124981618892527, 0.5620805258418327677 ) ) ;
#14360 = CARTESIAN_POINT ( 'NONE',  ( 21.86624219161040372, 3.264102293340572558, -3.922476187580016038 ) ) ;
#14361 = CARTESIAN_POINT ( 'NONE',  ( 2.894372913787321089, -32.75339045652842884, 7.670860738520328681 ) ) ;
#14362 = EDGE_CURVE ( 'NONE', #38041, #2116, #34416, .T. ) ;
#14363 = DIRECTION ( 'NONE',  ( 0.000000000000000000, 0.000000000000000000, 1.000000000000000000 ) ) ;
#14364 = CARTESIAN_POINT ( 'NONE',  ( 81.34875679478896870, 63.64560584540186738, 3.283621700565935164 ) ) ;
#14365 = CARTESIAN_POINT ( 'NONE',  ( 84.31734228151684363, 3.084090681639994003, 0.3216814846013044127 ) ) ;
#14366 = DIRECTION ( 'NONE',  ( -0.000000000000000000, -1.000000000000000000, -0.000000000000000000 ) ) ;
#14367 = VERTEX_POINT ( 'NONE', #25686 ) ;
#14368 = CARTESIAN_POINT ( 'NONE',  ( 28.46177005721402153, 1.600858155335632027, -4.033575672602236928 ) ) ;
#14369 = AXIS2_PLACEMENT_3D ( 'NONE', #36666, #8448, #21646 ) ;
#14370 = DIRECTION ( 'NONE',  ( -1.000000000000000000, 0.000000000000000000, 0.000000000000000000 ) ) ;
#14371 = CARTESIAN_POINT ( 'NONE',  ( 28.89404039681430092, -3.378319669541595349, -4.594214991691023542 ) ) ;
#14372 = CARTESIAN_POINT ( 'NONE',  ( 36.42059806513616849, -3.113254328073003396, -5.890713182194031283 ) ) ;
#14373 = DIRECTION ( 'NONE',  ( -0.000000000000000000, 1.000000000000000000, -0.000000000000000000 ) ) ;
#14374 = CARTESIAN_POINT ( 'NONE',  ( 21.73603501643664160, 0.2904304739139229596, -8.914614138416270706 ) ) ;
#14375 = CARTESIAN_POINT ( 'NONE',  ( 29.69387923751475356, -3.790797245299356799, -4.444098776127088257 ) ) ;
#14376 = ORIENTED_EDGE ( 'NONE', *, *, #29231, .T. ) ;
#14377 = CARTESIAN_POINT ( 'NONE',  ( 27.40455262169001927, 0.9565157424767126715, 4.483541236861189105 ) ) ;
#14378 = CARTESIAN_POINT ( 'NONE',  ( 33.46397865298071395, -3.088978469517898340, -5.429261216816389179 ) ) ;
#14379 = CIRCLE ( 'NONE', #642, 0.1000000000000028644 ) ;
#14380 = VERTEX_POINT ( 'NONE', #19305 ) ;
#14381 = EDGE_LOOP ( 'NONE', ( #1310, #16726, #4803, #31475 ) ) ;
#14382 = CARTESIAN_POINT ( 'NONE',  ( 37.10502815858426118, -3.127196235056679541, 5.976114625744155084 ) ) ;
#14383 = CARTESIAN_POINT ( 'NONE',  ( -1.619657530256499056, -30.67780588394286667, 6.863805608295729499 ) ) ;
#14384 = CARTESIAN_POINT ( 'NONE',  ( -70.83040762834239956, -45.61702805680359063, 10.00000000000001066 ) ) ;
#14385 = EDGE_CURVE ( 'NONE', #18658, #9338, #19444, .T. ) ;
#14386 = DIRECTION ( 'NONE',  ( 1.000000000000000000, -0.000000000000000000, 0.000000000000000000 ) ) ;
#14387 = ORIENTED_EDGE ( 'NONE', *, *, #34625, .T. ) ;
#14388 = CARTESIAN_POINT ( 'NONE',  ( -0.9786759135921931918, -26.64985754041175525, 6.700000000000000178 ) ) ;
#14389 = EDGE_LOOP ( 'NONE', ( #12431, #33713, #38592 ) ) ;
#14390 = EDGE_CURVE ( 'NONE', #28218, #33723, #35576, .T. ) ;
#14391 = ORIENTED_EDGE ( 'NONE', *, *, #14719, .F. ) ;
#14392 = CARTESIAN_POINT ( 'NONE',  ( 5.021941733704682775, -28.81150442415370705, 7.139196562012270597 ) ) ;
#14393 = ORIENTED_EDGE ( 'NONE', *, *, #33110, .F. ) ;
#14394 = CARTESIAN_POINT ( 'NONE',  ( 1.700390093233090871, -29.56993018339339940, 2.499999999999998668 ) ) ;
#14395 = EDGE_LOOP ( 'NONE', ( #7168, #4884, #23078, #12190 ) ) ;
#14397 = CARTESIAN_POINT ( 'NONE',  ( 21.87278005295215166, 2.930088050433785174, -3.925081081564471663 ) ) ;
#14396 = CARTESIAN_POINT ( 'NONE',  ( 4.821848874205628022, -27.98673438488562581, 6.931070083220556732 ) ) ;
#14398 = ORIENTED_EDGE ( 'NONE', *, *, #26657, .T. ) ;
#14399 = CARTESIAN_POINT ( 'NONE',  ( 24.11465845078392789, 3.025944685091374708, 3.701068920836044995 ) ) ;
#14400 = EDGE_CURVE ( 'NONE', #16672, #3667, #8847, .T. ) ;
#14401 = CARTESIAN_POINT ( 'NONE',  ( 79.56604632444070546, 66.26916991809633828, -1.539394129974356096 ) ) ;
#14402 = VECTOR ( 'NONE', #27797, 1000.000000000000000 ) ;
#14403 = DIRECTION ( 'NONE',  ( -0.000000000000000000, -0.000000000000000000, -1.000000000000000000 ) ) ;
#14404 = ORIENTED_EDGE ( 'NONE', *, *, #1096, .T. ) ;
#14405 =( BOUNDED_SURFACE ( )  B_SPLINE_SURFACE ( 3, 2, ( 
 ( #37917, #23249, #28871 ),
 ( #32725, #13219, #25785 ),
 ( #7981, #31560, #25579 ),
 ( #267, #1434, #36009 ),
 ( #19198, #7788, #13967 ),
 ( #3578, #20339, #26535 ),
 ( #38876, #28671, #39070 ),
 ( #3383, #32918, #9926 ),
 ( #23635, #29816, #6844 ),
 ( #14165, #3779, #678 ),
 ( #12807, #17242, #26737 ),
 ( #38124, #15899, #39275 ),
 ( #11065, #10869, #10668 ),
 ( #22508, #35815, #1627 ),
 ( #7591, #35072, #28460 ),
 ( #20145, #9724, #22305 ),
 ( #19402, #20959, #12082 ),
 ( #5725, #8592, #30648 ) ),
 .UNSPECIFIED., .F., .F., .T. ) 
 B_SPLINE_SURFACE_WITH_KNOTS ( ( 4, 2, 2, 2, 2, 2, 2, 2, 4 ),
 ( 3, 3 ),
 ( 0.1120466800155300452, 0.1143735119802114647, 0.1149552199713818196, 0.1151006469691744083, 0.1151733604680706957, 0.1152460739669669970, 0.1155369279625521745, 0.1167003439448928842, 0.1213540078742557232 ),
 ( 0.000000000000000000, 0.5795136697007319260 ),
 .UNSPECIFIED. ) 
 GEOMETRIC_REPRESENTATION_ITEM ( )  RATIONAL_B_SPLINE_SURFACE ( (
 ( 1.000000000000000000, 0.9576553671123291256, 0.9643893214183871798),
 ( 1.000000000000000000, 0.9576100389905349841, 0.9643512017072020104),
 ( 1.000000000000000000, 0.9575646527973793454, 0.9643130331595894944),
 ( 1.000000000000000000, 0.9575078494902402593, 0.9642652631312538247),
 ( 1.000000000000000000, 0.9574964853007239540, 0.9642557061585608214),
 ( 1.000000000000000000, 0.9574822756861615103, 0.9642437562611960722),
 ( 1.000000000000000000, 0.9574794335443638227, 0.9642413660976467682),
 ( 1.000000000000000000, 0.9574751700039521030, 0.9642377805767230470),
 ( 1.000000000000000000, 0.9574763124065062136, 0.9642387413060384826),
 ( 1.000000000000000000, 0.9574763124065062136, 0.9642387413060384826),
 ( 1.000000000000000000, 0.9574763124065062136, 0.9642387413060387047),
 ( 1.000000000000000000, 0.9574763124065062136, 0.9642387413060387047),
 ( 1.000000000000000000, 0.9574763124065062136, 0.9642387413060384826),
 ( 1.000000000000000000, 0.9574763124065062136, 0.9642387413060384826),
 ( 1.000000000000000000, 0.9574763124065062136, 0.9642387413060384826),
 ( 1.000000000000000000, 0.9574763124065062136, 0.9642387413060384826),
 ( 1.000000000000000000, 0.9574763124065062136, 0.9642387413060384826),
 ( 1.000000000000000000, 0.9574763124065062136, 0.9642387413060384826) ) ) 
 REPRESENTATION_ITEM ( '' )  SURFACE ( )  );
#14407 = CARTESIAN_POINT ( 'NONE',  ( 16.12894463104543874, -3.340519685027638186, -2.723709908311349626 ) ) ;
#14406 = DIRECTION ( 'NONE',  ( 0.000000000000000000, 0.000000000000000000, -1.000000000000000000 ) ) ;
#14408 = CARTESIAN_POINT ( 'NONE',  ( -70.92837670882107659, -56.35932253828836025, 5.950000000000010836 ) ) ;
#14409 = CARTESIAN_POINT ( 'NONE',  ( 73.86803306573551708, 62.08347648694397947, 3.642458757454824614 ) ) ;
#14410 = CARTESIAN_POINT ( 'NONE',  ( 24.56503363824644026, 2.726745707801141894, -3.881485574194932120 ) ) ;
#14411 = EDGE_LOOP ( 'NONE', ( #9437, #20966, #37634, #28849, #33931 ) ) ;
#14412 = CARTESIAN_POINT ( 'NONE',  ( -2.239401636788067140, -26.21711406210128104, 7.695279973900954751 ) ) ;
#14413 = CARTESIAN_POINT ( 'NONE',  ( 7.021324086407807030, -24.55319635012989110, 6.700000000000000178 ) ) ;
#14414 = AXIS2_PLACEMENT_3D ( 'NONE', #11720, #2505, #26983 ) ;
#14415 = DIRECTION ( 'NONE',  ( 0.000000000000000000, 1.000000000000000000, 0.000000000000000000 ) ) ;
#14416 = CARTESIAN_POINT ( 'NONE',  ( -62.77989223203980629, 36.45919279222904663, 4.734733336003105642 ) ) ;
#14417 = CARTESIAN_POINT ( 'NONE',  ( -70.92837670882106238, -48.61702805680358352, 6.000000000000002665 ) ) ;
#14418 = CARTESIAN_POINT ( 'NONE',  ( 81.87949262442930376, 63.91736224575979008, 2.817575383041585724 ) ) ;
#14419 = CARTESIAN_POINT ( 'NONE',  ( 86.23508606437836477, 1.494382965102754923, 4.690504771849753674 ) ) ;
#14420 = CARTESIAN_POINT ( 'NONE',  ( 29.75157451403313758, 0.8046206704518127362, -4.785270562610461020 ) ) ;
#14421 = CARTESIAN_POINT ( 'NONE',  ( -81.61576440455658599, -5.621349923170992469, -2.262421638520457634 ) ) ;
#14422 = CARTESIAN_POINT ( 'NONE',  ( 33.11976541959475639, -3.702904870183194586, 5.168375141609065082 ) ) ;
#14423 = CARTESIAN_POINT ( 'NONE',  ( 0.1054938181805689934, -26.45442818934983009, 6.903112506833893214 ) ) ;
#14424 = CARTESIAN_POINT ( 'NONE',  ( 30.55152536728312285, -0.03400272534400829161, -4.974702443634486215 ) ) ;
#14425 = CARTESIAN_POINT ( 'NONE',  ( -42.83131703149249603, -32.06993018339340296, 6.000000000000000000 ) ) ;
#14426 = DIRECTION ( 'NONE',  ( 0.000000000000000000, 0.6834397476448849096, -0.7300069255418718539 ) ) ;
#14427 = CARTESIAN_POINT ( 'NONE',  ( -75.45330471031414277, 33.71485196875532608, -8.800414904976364028 ) ) ;
#14428 = DIRECTION ( 'NONE',  ( 1.000000000000000000, 0.000000000000000000, 0.000000000000000000 ) ) ;
#14429 = ADVANCED_FACE ( 'NONE', ( #10228, #35381, #19710 ), #4085, .F. ) ;
#14430 = CARTESIAN_POINT ( 'NONE',  ( 2.321451664048270302, -33.01438696571141662, 7.635761828346576685 ) ) ;
#14431 = ORIENTED_EDGE ( 'NONE', *, *, #15308, .F. ) ;
#14432 = CARTESIAN_POINT ( 'NONE',  ( 36.41835342286016441, -1.780275768523426283, 5.760862909898532891 ) ) ;
#14433 = CARTESIAN_POINT ( 'NONE',  ( -70.02024225408199243, -0.3498828673826461233, 3.930990725878107384 ) ) ;
#14434 = CARTESIAN_POINT ( 'NONE',  ( 67.18992292689074475, 57.95373832061253694, -3.997022163556062324 ) ) ;
#14435 = EDGE_CURVE ( 'NONE', #23121, #36016, #20913, .T. ) ;
#14436 = DIRECTION ( 'NONE',  ( 0.000000000000000000, -0.000000000000000000, -1.000000000000000000 ) ) ;
#14437 = VERTEX_POINT ( 'NONE', #8132 ) ;
#14438 = DIRECTION ( 'NONE',  ( -8.398074759113475787E-17, 1.000000000000000000, 0.000000000000000000 ) ) ;
#14439 = EDGE_CURVE ( 'NONE', #31083, #8831, #4861, .T. ) ;
#14440 = CONICAL_SURFACE ( 'NONE', #36174, 6.406751979251626317, 0.7853981633974482790 ) ;
#14441 = CYLINDRICAL_SURFACE ( 'NONE', #17996, 0.09010775117052929883 ) ;
#14442 = DIRECTION ( 'NONE',  ( 0.000000000000000000, 1.000000000000000000, 0.000000000000000000 ) ) ;
#14443 = CARTESIAN_POINT ( 'NONE',  ( 0.4206787789642892905, -32.82760425591565223, 6.864368109219935121 ) ) ;
#14444 = CARTESIAN_POINT ( 'NONE',  ( 3.180781611337405668, -26.50125022492531102, 7.505001789837628223 ) ) ;
#14445 = ORIENTED_EDGE ( 'NONE', *, *, #30465, .T. ) ;
#14446 = CARTESIAN_POINT ( 'NONE',  ( 24.74716371176318219, 3.014745549408870406, 3.371973451314655534 ) ) ;
#14447 = EDGE_CURVE ( 'NONE', #36291, #5244, #26695, .T. ) ;
#14448 = CARTESIAN_POINT ( 'NONE',  ( 82.43037228308448050, 64.59322875725442259, -1.165579324820864571 ) ) ;
#14449 = CARTESIAN_POINT ( 'NONE',  ( 80.83425215363003247, 63.04220640063321213, 3.443978770203983242 ) ) ;
#14450 = ADVANCED_FACE ( 'NONE', ( #30180 ), #36164, .F. ) ;
#14451 = CARTESIAN_POINT ( 'NONE',  ( -41.07867591359219972, -26.64985754041175525, 6.800000000000000711 ) ) ;
#14452 = VERTEX_POINT ( 'NONE', #2001 ) ;
#14453 = CARTESIAN_POINT ( 'NONE',  ( 77.50572060368776306, 65.09508644891813844, -2.418543376929283450 ) ) ;
#14455 = CARTESIAN_POINT ( 'NONE',  ( 14.63804428710352212, -4.770366908001074435, -2.500000000000007550 ) ) ;
#14454 = CARTESIAN_POINT ( 'NONE',  ( 23.58038339315848120, 0.3885796826799637893, 5.537669914968013529 ) ) ;
#14456 = CARTESIAN_POINT ( 'NONE',  ( 81.34308989086048314, 63.28542802927258748, -3.228380831070265078 ) ) ;
#14457 = CARTESIAN_POINT ( 'NONE',  ( 78.04063183619207678, 64.12728436294460721, 3.505091495581009298 ) ) ;
#14458 = ORIENTED_EDGE ( 'NONE', *, *, #6383, .F. ) ;
#14459 = CARTESIAN_POINT ( 'NONE',  ( 35.33400523470628940, -3.787639325471320539, -5.505966337058852744 ) ) ;
#14460 = CARTESIAN_POINT ( 'NONE',  ( 81.16936534046872964, 61.30390240240431865, 1.014334479594651173 ) ) ;
#14461 = CARTESIAN_POINT ( 'NONE',  ( 4.351629544212539003, -31.85488319143487601, 6.880608371227950215 ) ) ;
#14462 = CARTESIAN_POINT ( 'NONE',  ( 29.80812890880734756, -3.278499718192964263, -4.781105184254491824 ) ) ;
#14463 = CARTESIAN_POINT ( 'NONE',  ( -70.92837670882107659, 26.72470171467712063, 0.000000000000000000 ) ) ;
#14464 = DIRECTION ( 'NONE',  ( 1.000000000000000000, 0.000000000000000000, -0.000000000000000000 ) ) ;
#14465 = ORIENTED_EDGE ( 'NONE', *, *, #38947, .T. ) ;
#14466 = CARTESIAN_POINT ( 'NONE',  ( 1.700390093233090871, -29.56993018339339940, 7.800000000000000711 ) ) ;
#14467 = CARTESIAN_POINT ( 'NONE',  ( 26.05868958960777704, 0.7870788155237375960, -4.421617872047712616 ) ) ;
#14468 = EDGE_LOOP ( 'NONE', ( #39454, #30695, #12986, #29690 ) ) ;
#14469 = CARTESIAN_POINT ( 'NONE',  ( -2.297321782777200561, -26.28614060416741438, 7.695279973900954751 ) ) ;
#14470 = CARTESIAN_POINT ( 'NONE',  ( 8.290806648384990041, -35.94265729135299381, 6.000000000000000000 ) ) ;
#14471 = AXIS2_PLACEMENT_3D ( 'NONE', #9268, #22268, #647 ) ;
#14472 = CARTESIAN_POINT ( 'NONE',  ( 5.149995510507904939, -30.16172614916897743, 7.638991368224662182 ) ) ;
#14473 = CARTESIAN_POINT ( 'NONE',  ( 37.10863271423323795, -2.405271516614433835, -5.952050369318877543 ) ) ;
#14474 = CARTESIAN_POINT ( 'NONE',  ( 30.67406393699503298, -3.593393542108534344, -4.777508688867102116 ) ) ;
#14475 = DIRECTION ( 'NONE',  ( -0.8660254037844212771, -0.5000000000000298650, 0.000000000000000000 ) ) ;
#14476 = DIRECTION ( 'NONE',  ( -0.000000000000000000, -0.000000000000000000, 1.000000000000000000 ) ) ;
#14477 = CARTESIAN_POINT ( 'NONE',  ( -72.42837670882107659, -47.11702805680359063, 38.00000000000000711 ) ) ;
#14478 = CARTESIAN_POINT ( 'NONE',  ( 2.775199688670615839, -32.79558988863323066, 6.866852738645443210 ) ) ;
#14479 = LINE ( 'NONE', #30353, #7923 ) ;
#14480 = CARTESIAN_POINT ( 'NONE',  ( -2.348748702180637693, -26.64985754041175525, 6.700000000000000178 ) ) ;
#14481 = CARTESIAN_POINT ( 'NONE',  ( 2.127989488270969787, -33.04371390207043646, 6.912143950357346966 ) ) ;
#14482 = APPLICATION_CONTEXT ( 'automotive_design' ) ;
#14483 = ORIENTED_EDGE ( 'NONE', *, *, #17982, .F. ) ;
#14484 = VERTEX_POINT ( 'NONE', #8338 ) ;
#14485 = CARTESIAN_POINT ( 'NONE',  ( 66.41901733680195719, 57.79934748174507320, 4.000000000000016875 ) ) ;
#14486 = CARTESIAN_POINT ( 'NONE',  ( 72.57946960881442067, 58.78899945845352448, -3.647993048395011595 ) ) ;
#14487 = AXIS2_PLACEMENT_3D ( 'NONE', #12823, #25595, #25192 ) ;
#14488 = CARTESIAN_POINT ( 'NONE',  ( 4.421194222029321885, -27.53100279559231112, 7.013842709614101167 ) ) ;
#14489 = ORIENTED_EDGE ( 'NONE', *, *, #28081, .F. ) ;
#14490 = CARTESIAN_POINT ( 'NONE',  ( 84.89189963960113516, 2.021164017676272184, 4.676249375175704159 ) ) ;
#14491 = CARTESIAN_POINT ( 'NONE',  ( -54.79610818216033152, 31.51396769785350926, 4.000000000000000000 ) ) ;
#14492 = CARTESIAN_POINT ( 'NONE',  ( 2.998870170862291129, -26.42764606383958892, 6.868387053540520704 ) ) ;
#14493 = DIRECTION ( 'NONE',  ( -1.000000000000000000, 0.000000000000000000, -0.000000000000000000 ) ) ;
#14494 = LINE ( 'NONE', #24384, #38315 ) ;
#14495 = ORIENTED_EDGE ( 'NONE', *, *, #37520, .F. ) ;
#14496 = CARTESIAN_POINT ( 'NONE',  ( 23.14867680946094097, 4.061912727637136733, 3.041127315635880901 ) ) ;
#14497 = ADVANCED_FACE ( 'NONE', ( #33695 ), #11624, .F. ) ;
#14498 = CARTESIAN_POINT ( 'NONE',  ( -59.01947560891952804, 27.90920910948504385, -6.147301388271595890 ) ) ;
#14499 = AXIS2_PLACEMENT_3D ( 'NONE', #16111, #9932, #6454 ) ;
#14500 = ADVANCED_FACE ( 'NONE', ( #39021 ), #33286, .T. ) ;
#14501 = CARTESIAN_POINT ( 'NONE',  ( 78.72519613238203817, 65.48187369539458302, -2.679976076788564754 ) ) ;
#14502 = CARTESIAN_POINT ( 'NONE',  ( 15.21972607795940391, 10.50943668950837839, -2.499999999997734701 ) ) ;
#14503 = CARTESIAN_POINT ( 'NONE',  ( 80.62899510017081184, 61.84672251665477205, 2.918211652848217152 ) ) ;
#14504 = CARTESIAN_POINT ( 'NONE',  ( 0.6486176734534436772, -26.33669956561429260, 7.759451378593096749 ) ) ;
#14505 = CARTESIAN_POINT ( 'NONE',  ( -10.24874870218063450, -26.64985754041175525, 6.700000000000000178 ) ) ;
#14506 = CARTESIAN_POINT ( 'NONE',  ( 3.928928892870411360, -27.00212668263422700, 6.887041543973314361 ) ) ;
#14507 = ORIENTED_EDGE ( 'NONE', *, *, #28267, .T. ) ;
#14508 = CARTESIAN_POINT ( 'NONE',  ( 21.85643539959778181, 2.105182337828026995, -13.78739850581801996 ) ) ;
#14509 = ORIENTED_EDGE ( 'NONE', *, *, #2459, .F. ) ;
#14510 = CYLINDRICAL_SURFACE ( 'NONE', #9744, 8.080217238368769372 ) ;
#14511 = CIRCLE ( 'NONE', #9946, 0.1000000000000028644 ) ;
#14512 = CARTESIAN_POINT ( 'NONE',  ( 14.70276859592049057, -4.942772565485702430, 2.499999999999277911 ) ) ;
#14513 = CARTESIAN_POINT ( 'NONE',  ( -79.87450223356385948, 10.49415034902278698, -4.486381563923941052 ) ) ;
#14514 = CARTESIAN_POINT ( 'NONE',  ( -2.712160580843945734, -31.23359347163986399, 7.695279973900954751 ) ) ;
#14515 = DIRECTION ( 'NONE',  ( 1.000000000000000000, -7.930164461608261228E-15, 0.000000000000000000 ) ) ;
#14516 = CARTESIAN_POINT ( 'NONE',  ( 79.33528816075222778, 65.72664079943768911, 2.661900242191239219 ) ) ;
#14517 = DIRECTION ( 'NONE',  ( -0.000000000000000000, 1.000000000000000000, 0.000000000000000000 ) ) ;
#14518 =( BOUNDED_CURVE ( )  B_SPLINE_CURVE ( 3, ( #15282, #12189, #12400, #15483 ),
 .UNSPECIFIED., .F., .F. ) 
 B_SPLINE_CURVE_WITH_KNOTS ( ( 4, 4 ),
 ( 1.381924640371167801, 1.574767692156076482 ),
 .UNSPECIFIED. ) 
 CURVE ( )  GEOMETRIC_REPRESENTATION_ITEM ( )  RATIONAL_B_SPLINE_CURVE ( ( 1.000000000000000000, 0.9969033633783032089, 0.9969033633783032089, 1.000000000000000000 ) ) 
 REPRESENTATION_ITEM ( '' )  );
#14519 = CARTESIAN_POINT ( 'NONE',  ( 3.861119344891603244, -26.94481130969886706, 7.721096864323898856 ) ) ;
#14520 = FACE_OUTER_BOUND ( 'NONE', #18536, .T. ) ;
#14521 = CARTESIAN_POINT ( 'NONE',  ( 0.5325725529551263993, -26.27050565893173228, 6.894806418505347700 ) ) ;
#14522 = CARTESIAN_POINT ( 'NONE',  ( 4.405768222705582993, -27.34935008554416669, 6.887161170156904433 ) ) ;
#14523 = AXIS2_PLACEMENT_3D ( 'NONE', #18701, #37629, #31686 ) ;
#14524 = CARTESIAN_POINT ( 'NONE',  ( 88.04454721149249963, -0.5380896775427260748, 2.907127687869381916 ) ) ;
#14525 = DIRECTION ( 'NONE',  ( -0.000000000000000000, 1.000000000000000000, -0.000000000000000000 ) ) ;
#14526 = VERTEX_POINT ( 'NONE', #5474 ) ;
#14527 = CARTESIAN_POINT ( 'NONE',  ( 68.10340323693496600, 58.18244674706191688, 3.988335407916730802 ) ) ;
#14528 = CARTESIAN_POINT ( 'NONE',  ( 35.86997984655084792, -2.084313029741385659, 5.804775892431827344 ) ) ;
#14529 = CARTESIAN_POINT ( 'NONE',  ( 2.213664895657379006, -33.02484726641009871, 7.776484688137383472 ) ) ;
#14530 = CARTESIAN_POINT ( 'NONE',  ( 85.64278173364962754, 1.868356560669967470, -5.099220668941490509 ) ) ;
#14531 = CARTESIAN_POINT ( 'NONE',  ( 4.875541254183488604, -30.78583112718583692, 6.887041543973317026 ) ) ;
#14532 = CARTESIAN_POINT ( 'NONE',  ( -1.632457674179491391, -28.89752720953548604, 6.870716933885662847 ) ) ;
#14533 = CARTESIAN_POINT ( 'NONE',  ( -58.25352014915284826, 31.25337030895682133, 4.614317915849918350 ) ) ;
#14534 = CARTESIAN_POINT ( 'NONE',  ( -0.6056525554631260189, -32.20285051197402026, 6.867280401193708528 ) ) ;
#14535 = ORIENTED_EDGE ( 'NONE', *, *, #17686, .F. ) ;
#14536 = CARTESIAN_POINT ( 'NONE',  ( -71.92837670882107659, -20.78299143688747819, 3.916079783099609912 ) ) ;
#14537 = ADVANCED_FACE ( 'NONE', ( #14520 ), #24202, .F. ) ;
#14538 = CARTESIAN_POINT ( 'NONE',  ( 78.93661819519692813, 65.67810670493901171, -2.545842637937977937 ) ) ;
#14539 = DIRECTION ( 'NONE',  ( 0.7541618601367534591, 0.000000000000000000, 0.6566885781822856538 ) ) ;
#14540 = CARTESIAN_POINT ( 'NONE',  ( 80.84665409946110515, 62.14681778383299360, 3.018898740118469703 ) ) ;
#14541 = CARTESIAN_POINT ( 'NONE',  ( 26.54964660807501531, 1.667999962647538359, 4.320834639766450991 ) ) ;
#14543 = ORIENTED_EDGE ( 'NONE', *, *, #17741, .F. ) ;
#14542 = DIRECTION ( 'NONE',  ( 0.000000000000000000, 0.000000000000000000, 1.000000000000000000 ) ) ;
#14544 = B_SPLINE_CURVE_WITH_KNOTS ( 'NONE', 3,
 ( #10320, #39122, #16495, #28868, #29072, #13215, #878, #35466, #7238, #10518, #36061, #38721, #23098, #19801, #675, #38921, #10919, #20190, #26391, #13410, #10713, #13616, #32372, #25985, #29664, #23292, #38517 ),
 .UNSPECIFIED., .F., .F.,
 ( 4, 1, 2, 2, 1, 1, 1, 1, 2, 2, 1, 1, 1, 1, 1, 2, 2, 1, 4 ),
 ( 0.07055524994525608218, 0.1867358437020780471, 0.2448261405804889046, 0.2738712890196948191, 0.3029164374589006781, 0.4190970312157243916, 0.4771873280941357209, 0.4917099023137387892, 0.4989711894235402401, 0.5007865112009901587, 0.5026018329784399663, 0.5062324765333394705, 0.5352776249725555990, 0.6514582187294180038, 0.7095485156078492617, 0.7385936640470648351, 0.7531162382666727328, 0.7676388124862805196, 1.000000000000000000 ),
 .UNSPECIFIED. ) ;
#14545 = CARTESIAN_POINT ( 'NONE',  ( 73.97359482965943300, 60.32890003735500528, -3.899931323540655637 ) ) ;
#14546 = VECTOR ( 'NONE', #16476, 1000.000000000000000 ) ;
#14547 = FACE_OUTER_BOUND ( 'NONE', #36207, .T. ) ;
#14549 = CARTESIAN_POINT ( 'NONE',  ( -2.248748702180634940, -26.64985754041175525, 6.700000000000000178 ) ) ;
#14548 = CARTESIAN_POINT ( 'NONE',  ( 36.10284116201629701, 0.9159659085930716982, -6.000000000000000000 ) ) ;
#14550 = CARTESIAN_POINT ( 'NONE',  ( -1.795519090086910019, -29.40075872605237706, 7.013842709614101167 ) ) ;
#14551 = CARTESIAN_POINT ( 'NONE',  ( 5.165995621756787948, -25.65200095290807880, 7.013842709614101167 ) ) ;
#14552 = CARTESIAN_POINT ( 'NONE',  ( 22.17125346225300575, 4.446648860891334820, -3.726893279828063843 ) ) ;
#14553 = ORIENTED_EDGE ( 'NONE', *, *, #35846, .T. ) ;
#14554 = DIRECTION ( 'NONE',  ( 0.000000000000000000, -1.000000000000000000, 0.000000000000000000 ) ) ;
#14555 = CARTESIAN_POINT ( 'NONE',  ( 22.76577552469399990, -5.388071312449273620, 6.143773694815460651 ) ) ;
#14556 = FACE_BOUND ( 'NONE', #34340, .T. ) ;
#14557 = ORIENTED_EDGE ( 'NONE', *, *, #25668, .F. ) ;
#14558 = LINE ( 'NONE', #39476, #32733 ) ;
#14559 = CARTESIAN_POINT ( 'NONE',  ( 85.39132736373097998, 1.761725527925377399, -5.190388716534374502 ) ) ;
#14560 = CARTESIAN_POINT ( 'NONE',  ( 8.290806648384990041, -35.94265729135299381, 2.500000000000000000 ) ) ;
#14561 = ORIENTED_EDGE ( 'NONE', *, *, #23146, .T. ) ;
#14562 = CARTESIAN_POINT ( 'NONE',  ( 26.98979804764019264, 2.155375236454192933, -3.758468440649340714 ) ) ;
#14563 = EDGE_CURVE ( 'NONE', #10365, #32868, #1728, .T. ) ;
#14564 = CARTESIAN_POINT ( 'NONE',  ( 22.18104894856640996, 5.504333011849090518, -2.539813209877764155 ) ) ;
#14565 = CARTESIAN_POINT ( 'NONE',  ( 15.25857687985927136, -3.898425631526794000, -2.584722552834652465 ) ) ;
#14566 = CARTESIAN_POINT ( 'NONE',  ( 36.14130771815730725, -3.140490948321353670, -5.847123168885349997 ) ) ;
#14567 = CARTESIAN_POINT ( 'NONE',  ( 3.121324086407806231, -26.64985754041175525, 6.700000000000000178 ) ) ;
#14568 = CARTESIAN_POINT ( 'NONE',  ( 25.67091747518093570, 1.146822820001185184, -4.432699664903578807 ) ) ;
#14569 = EDGE_CURVE ( 'NONE', #29836, #24849, #21444, .T. ) ;
#14570 = CARTESIAN_POINT ( 'NONE',  ( -12.44874870218064267, -26.64985754041175525, 6.700000000000000178 ) ) ;
#14571 = VERTEX_POINT ( 'NONE', #23989 ) ;
#14572 = CARTESIAN_POINT ( 'NONE',  ( 2.782197798051136317, -32.89830469346890141, 7.754798119455333705 ) ) ;
#14573 = LINE ( 'NONE', #17675, #14307 ) ;
#14574 = EDGE_CURVE ( 'NONE', #16283, #17660, #20779, .T. ) ;
#14575 = CARTESIAN_POINT ( 'NONE',  ( 4.985095813259256659, -28.36132152183090582, 7.756742906098588186 ) ) ;
#14576 = VERTEX_POINT ( 'NONE', #2198 ) ;
#14577 = ORIENTED_EDGE ( 'NONE', *, *, #30439, .T. ) ;
#14578 = CARTESIAN_POINT ( 'NONE',  ( 33.45688159892293356, -3.834031077008411614, 5.088667958700237470 ) ) ;
#14579 = CARTESIAN_POINT ( 'NONE',  ( -80.92837670882107659, 2.429809908903242555, 15.50000000000000000 ) ) ;
#14580 = CARTESIAN_POINT ( 'NONE',  ( 22.10870846509921250, -3.077893895552592074, -3.560816367895537127 ) ) ;
#14581 = VECTOR ( 'NONE', #39300, 1000.000000000000000 ) ;
#14582 = DIRECTION ( 'NONE',  ( 0.000000000000000000, 1.000000000000000000, 0.000000000000000000 ) ) ;
#14583 = ORIENTED_EDGE ( 'NONE', *, *, #36526, .F. ) ;
#14584 = CARTESIAN_POINT ( 'NONE',  ( -1.020414035563122601, -31.60885757119451256, 7.013842709614101167 ) ) ;
#14585 = ORIENTED_EDGE ( 'NONE', *, *, #21170, .F. ) ;
#14586 = EDGE_LOOP ( 'NONE', ( #35372, #4933, #35427, #39316 ) ) ;
#14587 = CYLINDRICAL_SURFACE ( 'NONE', #10184, 0.09010775117053103356 ) ;
#14588 = EDGE_CURVE ( 'NONE', #5754, #393, #18017, .T. ) ;
#14589 = CARTESIAN_POINT ( 'NONE',  ( 79.70553327529583498, 65.02082924290299104, -3.340002271463676120 ) ) ;
#14590 = CARTESIAN_POINT ( 'NONE',  ( 14.75868448971168512, -5.144185890768196323, 2.500012889186591813 ) ) ;
#14591 = EDGE_LOOP ( 'NONE', ( #40298, #33978, #4143, #8890 ) ) ;
#14593 = CARTESIAN_POINT ( 'NONE',  ( 21.88711032996733863, 3.208699644456277866, -3.395463446387114725 ) ) ;
#14592 = CARTESIAN_POINT ( 'NONE',  ( -40.87867591359218977, -24.55319635012989110, 6.700000000000000178 ) ) ;
#14594 = ORIENTED_EDGE ( 'NONE', *, *, #1204, .T. ) ;
#14595 = CARTESIAN_POINT ( 'NONE',  ( 22.00057757746165166, 4.523971029709453973, 3.846587773178183678 ) ) ;
#14596 = CARTESIAN_POINT ( 'NONE',  ( 81.24150567074659079, 65.50891479329992251, -2.400449347018692059 ) ) ;
#14597 = CARTESIAN_POINT ( 'NONE',  ( -59.00782325774520132, 28.07066389825120822, 6.403654028263575881 ) ) ;
#14599 = CARTESIAN_POINT ( 'NONE',  ( 26.17280925958501214, -2.761831904353556411, -4.291297895378931138 ) ) ;
#14598 = CARTESIAN_POINT ( 'NONE',  ( 0.05294289315275076124, -26.59572142761524205, 7.785172627573962778 ) ) ;
#14600 = DIRECTION ( 'NONE',  ( 0.000000000000000000, 0.000000000000000000, 1.000000000000000000 ) ) ;
#14601 = CARTESIAN_POINT ( 'NONE',  ( 75.27660179239936156, 61.98686977074611804, 3.846775394605563836 ) ) ;
#14602 = ORIENTED_EDGE ( 'NONE', *, *, #36087, .T. ) ;
#14603 = CARTESIAN_POINT ( 'NONE',  ( 22.48581518839592874, 2.618461469189475199, -4.833321383114350667 ) ) ;
#14604 = ORIENTED_EDGE ( 'NONE', *, *, #24443, .F. ) ;
#14605 = EDGE_CURVE ( 'NONE', #6597, #13346, #10807, .T. ) ;
#14606 = DIRECTION ( 'NONE',  ( -0.8660254037844345998, -0.5000000000000071054, -0.000000000000000000 ) ) ;
#14607 = CARTESIAN_POINT ( 'NONE',  ( 1.294658908450306845, -26.08664770627206053, 7.387053503561885393 ) ) ;
#14608 = CARTESIAN_POINT ( 'NONE',  ( -62.88953457012820536, 35.56785342129472838, 5.946384872131353916 ) ) ;
#14609 = CARTESIAN_POINT ( 'NONE',  ( -70.92837670882107659, 28.72470171467712063, 6.000000000000005329 ) ) ;
#14610 = CARTESIAN_POINT ( 'NONE',  ( 81.51784234612475188, 64.89972252180031376, 2.776691787112188337 ) ) ;
#14611 = CARTESIAN_POINT ( 'NONE',  ( 86.07545474579461597, 1.673688438695506431, -4.651254279175787154 ) ) ;
#14612 = CARTESIAN_POINT ( 'NONE',  ( 29.24680661740138632, 2.095232292622827508, -1.948189103474716966 ) ) ;
#14613 = CARTESIAN_POINT ( 'NONE',  ( -2.639489883291917138, -27.04870784343005141, 7.635761828346577573 ) ) ;
#14614 = AXIS2_PLACEMENT_3D ( 'NONE', #19027, #18403, #9755 ) ;
#14615 = CARTESIAN_POINT ( 'NONE',  ( 19.72131146634190557, -3.044362691710549296, 3.219876361117069763 ) ) ;
#14616 = CARTESIAN_POINT ( 'NONE',  ( -4.224659823956008253, -51.67615071827237472, -6.000000000000000000 ) ) ;
#14617 = CARTESIAN_POINT ( 'NONE',  ( 29.17646580786398758, 0.5759241497138282151, -4.760091143445980499 ) ) ;
#14618 = CARTESIAN_POINT ( 'NONE',  ( 4.630655976963546472, -31.48396831510932969, 6.961115707816232678 ) ) ;
#14619 = EDGE_CURVE ( 'NONE', #15871, #37640, #1790, .T. ) ;
#14620 = EDGE_CURVE ( 'NONE', #17512, #7534, #15721, .T. ) ;
#14621 = DIRECTION ( 'NONE',  ( 1.000000000000000000, 0.000000000000000000, 0.000000000000000000 ) ) ;
#14622 = B_SPLINE_CURVE_WITH_KNOTS ( 'NONE', 3,
 ( #2567, #33853, #11987, #30138, #33235, #11174, #14472, #27241, #11377, #40204 ),
 .UNSPECIFIED., .F., .F.,
 ( 4, 3, 3, 4 ),
 ( 8.673617379884035472E-19, 3.025505781527810907E-05, 6.051003801291621463E-05, 6.468145402690745997E-05 ),
 .UNSPECIFIED. ) ;
#14623 = ADVANCED_FACE ( 'NONE', ( #24825 ), #15137, .T. ) ;
#14624 = CARTESIAN_POINT ( 'NONE',  ( -72.84815947045233031, 2.429809908903243443, -12.50000000000000000 ) ) ;
#14625 = DIRECTION ( 'NONE',  ( -0.000000000000000000, 1.000000000000000000, -0.000000000000000000 ) ) ;
#14626 = VERTEX_POINT ( 'NONE', #21740 ) ;
#14627 = CARTESIAN_POINT ( 'NONE',  ( 33.68482843757833223, -3.836899954132453772, 5.141354644792926365 ) ) ;
#14628 = CARTESIAN_POINT ( 'NONE',  ( -70.29787437547823004, 0.001187990818876110462, 5.979574859000733156 ) ) ;
#14629 = B_SPLINE_CURVE_WITH_KNOTS ( 'NONE', 3,
 ( #13687, #4227, #35723, #10777, #8090, #5024, #939, #26651, #38789, #23357, #22963, #13476, #7703, #16753, #7499, #32639, #38581, #16961, #29728, #20253, #32837, #4629, #39184, #10979, #7904 ),
 .UNSPECIFIED., .F., .F.,
 ( 4, 3, 3, 3, 3, 3, 3, 3, 4 ),
 ( 7.730982992130896385E-05, 9.267501192706072816E-05, 0.0001241882240135149700, 0.0001556618703051600237, 0.0001866161554452170994, 0.0002167966385860923466, 0.0002463805737537726106, 0.0002758761370306489122, 0.0002847094172290014712 ),
 .UNSPECIFIED. ) ;
#14630 = CARTESIAN_POINT ( 'NONE',  ( 66.72049918463439155, 57.87600310258397940, -3.999713739232678034 ) ) ;
#14631 = EDGE_CURVE ( 'NONE', #20444, #3707, #413, .T. ) ;
#14632 = DIRECTION ( 'NONE',  ( 1.000000000000000000, 0.000000000000000000, 0.000000000000000000 ) ) ;
#14633 = DIRECTION ( 'NONE',  ( 0.000000000000000000, 1.000000000000000000, 0.000000000000000000 ) ) ;
#14634 = ORIENTED_EDGE ( 'NONE', *, *, #9368, .F. ) ;
#14635 = CARTESIAN_POINT ( 'NONE',  ( -0.4584151234726890900, -32.19663272579155944, 7.712764235869099316 ) ) ;
#14636 = CARTESIAN_POINT ( 'NONE',  ( 3.792809966073827255, -32.24981515609748328, 7.757178535559530630 ) ) ;
#14637 = FACE_OUTER_BOUND ( 'NONE', #8361, .T. ) ;
#14638 = CARTESIAN_POINT ( 'NONE',  ( -74.68498725152623763, 9.372166970630278371, 9.273481029445454382 ) ) ;
#14639 = VERTEX_POINT ( 'NONE', #33906 ) ;
#14640 = CARTESIAN_POINT ( 'NONE',  ( -4.878675913592187108, -26.64985754041175525, 6.800000000000000711 ) ) ;
#14641 = ORIENTED_EDGE ( 'NONE', *, *, #37075, .T. ) ;
#14642 = CARTESIAN_POINT ( 'NONE',  ( 22.87956138668360495, 4.318478688965076806, 3.085875429863905950 ) ) ;
#14643 = CARTESIAN_POINT ( 'NONE',  ( 82.25590015743732408, 64.89408798057370120, -1.328060019258380242 ) ) ;
#14644 = CARTESIAN_POINT ( 'NONE',  ( 80.04018988431747061, 64.49293993294402583, 3.578839808218922780 ) ) ;
#14645 = ORIENTED_EDGE ( 'NONE', *, *, #11255, .T. ) ;
#14646 = CARTESIAN_POINT ( 'NONE',  ( -0.1065785265816254768, -32.45002973820478331, 6.863904403958575706 ) ) ;
#14647 = ORIENTED_EDGE ( 'NONE', *, *, #33943, .T. ) ;
#14648 = CARTESIAN_POINT ( 'NONE',  ( 79.26824131213432167, 60.90178692369111957, -2.725046208697020855 ) ) ;
#14650 = CARTESIAN_POINT ( 'NONE',  ( 14.75163840144606020, -5.120888621327094548, -2.500049689809528797 ) ) ;
#14649 = CARTESIAN_POINT ( 'NONE',  ( 21.78202853633694502, 0.2105828418074676689, 8.406744294290200870 ) ) ;
#14651 = CARTESIAN_POINT ( 'NONE',  ( 78.82533416220574907, 66.11379887182106074, -1.400336002810711244 ) ) ;
#14652 = CARTESIAN_POINT ( 'NONE',  ( 79.75127500915171197, 61.39906162938306977, 2.976941560848460178 ) ) ;
#14653 = VERTEX_POINT ( 'NONE', #9364 ) ;
#14654 = AXIS2_PLACEMENT_3D ( 'NONE', #23358, #1352, #17157 ) ;
#14655 = CARTESIAN_POINT ( 'NONE',  ( -2.652992490026568007, -32.06776532245774547, 7.635761828346577573 ) ) ;
#14656 = VERTEX_POINT ( 'NONE', #11828 ) ;
#14657 = CARTESIAN_POINT ( 'NONE',  ( 82.16824647341044852, 62.22308028923548306, 1.246975333546937348 ) ) ;
#14659 = CARTESIAN_POINT ( 'NONE',  ( 87.04213330793392345, 0.5878691963682337596, -6.000000000000000000 ) ) ;
#14658 = CARTESIAN_POINT ( 'NONE',  ( 3.418165973099760890, -26.63576239896834608, 7.779495906702016406 ) ) ;
#14660 = CARTESIAN_POINT ( 'NONE',  ( 26.86540377008237357, 1.668949755151340586, -4.708546860826485769 ) ) ;
#14661 = CARTESIAN_POINT ( 'NONE',  ( -1.432293644835494373, -27.47664038617742577, -4.000000000000000000 ) ) ;
#14662 = DIRECTION ( 'NONE',  ( 0.000000000000000000, 0.000000000000000000, -1.000000000000000000 ) ) ;
#14663 = ORIENTED_EDGE ( 'NONE', *, *, #18792, .F. ) ;
#14664 = CARTESIAN_POINT ( 'NONE',  ( 1.654198408036650969, -33.06963691447906939, 6.880608371227948439 ) ) ;
#14665 = CARTESIAN_POINT ( 'NONE',  ( 27.41552500817463667, 1.019591371738703955, -4.485159083204544928 ) ) ;
#14666 = EDGE_CURVE ( 'NONE', #29368, #1666, #8955, .T. ) ;
#14667 = CONICAL_SURFACE ( 'NONE', #38362, 3.961287410364449979, 0.08726646259971682085 ) ;
#14668 = CARTESIAN_POINT ( 'NONE',  ( 1.686887486498407140, -26.06995622926011436, 7.635761828346576685 ) ) ;
#14669 = DIRECTION ( 'NONE',  ( -0.000000000000000000, -0.000000000000000000, -1.000000000000000000 ) ) ;
#14670 = CARTESIAN_POINT ( 'NONE',  ( 5.175423985860502007, -29.15262985496314130, 6.961115707816242448 ) ) ;
#14671 = EDGE_CURVE ( 'NONE', #11908, #26319, #18846, .T. ) ;
#14672 = CARTESIAN_POINT ( 'NONE',  ( -71.54330396476282772, 0.01623308404284228706, 3.969121680875197455 ) ) ;
#14673 = CARTESIAN_POINT ( 'NONE',  ( 37.00886176876311140, -2.250709667194641828, -5.913644327890312802 ) ) ;
#14674 = DIRECTION ( 'NONE',  ( 0.000000000000000000, 0.000000000000000000, 1.000000000000000000 ) ) ;
#14675 = DIRECTION ( 'NONE',  ( 1.000000000000000000, 0.000000000000000000, -0.000000000000000000 ) ) ;
#14676 = CARTESIAN_POINT ( 'NONE',  ( 5.043507888204011635, -28.95060522107654677, 7.661510568013096822 ) ) ;
#14677 = DIRECTION ( 'NONE',  ( -0.000000000000000000, -0.000000000000000000, -1.000000000000000000 ) ) ;
#14678 = LINE ( 'NONE', #7906, #22694 ) ;
#14679 = EDGE_CURVE ( 'NONE', #1666, #30327, #14193, .T. ) ;
#14680 = CARTESIAN_POINT ( 'NONE',  ( 4.930594809156889191, -28.50887757203159012, 7.768425012602591551 ) ) ;
#14681 = CARTESIAN_POINT ( 'NONE',  ( 14.75069249142107886, -5.116492627577003738, -2.500060313030776804 ) ) ;
#14682 = CARTESIAN_POINT ( 'NONE',  ( 23.33329484996965419, 2.006436124235808638, -4.751833140929669241 ) ) ;
#14683 = VERTEX_POINT ( 'NONE', #2619 ) ;
#14684 = VERTEX_POINT ( 'NONE', #22158 ) ;
#14685 = CARTESIAN_POINT ( 'NONE',  ( 66.42594280077616986, 57.77978248037118192, 4.000000000000010658 ) ) ;
#14686 = CARTESIAN_POINT ( 'NONE',  ( 69.31827979293011310, 58.50063561948233115, -3.969490915146639765 ) ) ;
#14687 = AXIS2_PLACEMENT_3D ( 'NONE', #17776, #30362, #2169 ) ;
#14688 = ORIENTED_EDGE ( 'NONE', *, *, #22477, .F. ) ;
#14689 = CIRCLE ( 'NONE', #16003, 0.1000000000000028644 ) ;
#14690 = CARTESIAN_POINT ( 'NONE',  ( 1.057242960569752199, -26.12952878737186424, 7.695279973900954751 ) ) ;
#14691 = CARTESIAN_POINT ( 'NONE',  ( 0.1853991482571498706, -26.52611638543517003, 6.959317978105165281 ) ) ;
#14692 = CARTESIAN_POINT ( 'NONE',  ( -68.92837670882107659, -42.87473357531881391, 0.000000000000000000 ) ) ;
#14693 = CARTESIAN_POINT ( 'NONE',  ( -2.949010729501093220, -28.55700733037702221, 6.894806418505347700 ) ) ;
#14694 = PLANE ( 'NONE',  #19894 ) ;
#14695 = ORIENTED_EDGE ( 'NONE', *, *, #264, .T. ) ;
#14696 = CARTESIAN_POINT ( 'NONE',  ( 17.04338035915418459, 48.81061067247630092, -1.000000000000000000 ) ) ;
#14697 = ORIENTED_EDGE ( 'NONE', *, *, #17587, .T. ) ;
#14698 = CARTESIAN_POINT ( 'NONE',  ( 79.36500080098822707, 64.41263654525117488, -3.571698303486884107 ) ) ;
#14699 = CARTESIAN_POINT ( 'NONE',  ( 16.50401505813599101, 9.937674115411510911, -2.499999999999894751 ) ) ;
#14700 = CARTESIAN_POINT ( 'NONE',  ( 81.90837201943155321, 62.87926165960869440, -2.626729253126907526 ) ) ;
#14701 = CARTESIAN_POINT ( 'NONE',  ( 80.53991883815837127, 62.31343731104875872, 3.289664858626286659 ) ) ;
#14702 = ORIENTED_EDGE ( 'NONE', *, *, #24547, .T. ) ;
#14703 = DIRECTION ( 'NONE',  ( -0.7394003126383920099, 0.1303762246624204368, -0.6605219282605403475 ) ) ;
#14704 = CARTESIAN_POINT ( 'NONE',  ( 14.82981423308607560, 12.75311901897797107, -2.505853893009207578 ) ) ;
#14705 = CARTESIAN_POINT ( 'NONE',  ( 2.493210317801513476, -26.25641980554438604, 7.386948897581451234 ) ) ;
#14706 = CARTESIAN_POINT ( 'NONE',  ( 21.85643539959774273, 10.58808081918846256, 0.01331417752983106093 ) ) ;
#14707 = EDGE_LOOP ( 'NONE', ( #10146, #1402, #38117, #5859, #10092 ) ) ;
#14708 = FACE_OUTER_BOUND ( 'NONE', #31494, .T. ) ;
#14709 = CARTESIAN_POINT ( 'NONE',  ( 14.68624896554715598, -4.761818446054777887, 2.499999999999112266 ) ) ;
#14710 = CIRCLE ( 'NONE', #35791, 7.341749246864647915 ) ;
#14711 = CARTESIAN_POINT ( 'NONE',  ( -75.05634802856252463, 7.993964939743821496, -10.46629622540592308 ) ) ;
#14712 = CARTESIAN_POINT ( 'NONE',  ( -59.93345510331043613, 24.73247967741477993, 9.800414904976365804 ) ) ;
#14713 = CARTESIAN_POINT ( 'NONE',  ( 2.460256200828665918, -26.25592905205268224, 6.882085323592685988 ) ) ;
#14714 = CARTESIAN_POINT ( 'NONE',  ( 4.907464300517769829, -30.69894525369553762, 7.693875151218754205 ) ) ;
#14715 = CARTESIAN_POINT ( 'NONE',  ( -7.078675913592194391, -26.64985754041175525, 6.800000000000000711 ) ) ;
#14716 = DIRECTION ( 'NONE',  ( -0.000000000000000000, -1.000000000000000000, -0.000000000000000000 ) ) ;
#14717 = CARTESIAN_POINT ( 'NONE',  ( -70.66690635095469020, 0.1910696742817396265, 9.997314914349638926 ) ) ;
#14718 = CARTESIAN_POINT ( 'NONE',  ( 5.042998615515850602, -28.94786244852631896, 7.721096864323902409 ) ) ;
#14719 = EDGE_CURVE ( 'NONE', #23027, #33929, #19473, .T. ) ;
#14720 = EDGE_CURVE ( 'NONE', #10898, #22409, #15760, .T. ) ;
#14721 = CARTESIAN_POINT ( 'NONE',  ( -70.05472099546194897, -0.2795093347480433477, 3.936269516561393456 ) ) ;
#14722 = CARTESIAN_POINT ( 'NONE',  ( 1.128064129311358244, -33.02281926226938680, 7.685194954629195330 ) ) ;
#14723 = EDGE_CURVE ( 'NONE', #28994, #3514, #18625, .T. ) ;
#14724 = CARTESIAN_POINT ( 'NONE',  ( 4.164674408718673781, -31.91242951707208420, 6.949473656533220023 ) ) ;
#14725 = VECTOR ( 'NONE', #24752, 1000.000000000000114 ) ;
#14726 = ORIENTED_EDGE ( 'NONE', *, *, #3218, .T. ) ;
#14727 = CARTESIAN_POINT ( 'NONE',  ( 68.13924211849639789, 58.08649371134929140, 3.978477839347963840 ) ) ;
#14728 = ORIENTED_EDGE ( 'NONE', *, *, #20447, .T. ) ;
#14729 = CYLINDRICAL_SURFACE ( 'NONE', #19455, 0.1000000000000028644 ) ;
#14730 = CARTESIAN_POINT ( 'NONE',  ( 86.60363381072151867, 0.9779648536402296699, 5.693185077828528229 ) ) ;
#14732 = FACE_OUTER_BOUND ( 'NONE', #33881, .T. ) ;
#14731 = CARTESIAN_POINT ( 'NONE',  ( 29.28314298262022319, 1.964681093867868933, 2.525543949525632659 ) ) ;
#14733 = PRODUCT_DEFINITION_SHAPE ( 'NONE', 'NONE',  #40722 ) ;
#14734 = CARTESIAN_POINT ( 'NONE',  ( -1.613611038107622520, -28.81006407579781126, 6.882085323592686876 ) ) ;
#14735 = CARTESIAN_POINT ( 'NONE',  ( 4.911690090265110165, -28.45299136274915952, 6.894806418505345924 ) ) ;
#14736 = CARTESIAN_POINT ( 'NONE',  ( -0.6288947886013260824, -32.18231164535578159, 6.863784140767622333 ) ) ;
#14737 = VERTEX_POINT ( 'NONE', #37370 ) ;
#14738 = DIRECTION ( 'NONE',  ( -0.000000000000000000, -0.000000000000000000, 1.000000000000000000 ) ) ;
#14739 = AXIS2_PLACEMENT_3D ( 'NONE', #38933, #25794, #13422 ) ;
#14740 = VECTOR ( 'NONE', #15082, 1000.000000000000000 ) ;
#14741 = ORIENTED_EDGE ( 'NONE', *, *, #12021, .F. ) ;
#14742 = CARTESIAN_POINT ( 'NONE',  ( 80.93309715666640614, 61.70751139687529019, -2.576318598473983368 ) ) ;
#14743 = B_SPLINE_CURVE_WITH_KNOTS ( 'NONE', 3,
 ( #3290, #28366, #30861, #19102, #27746, #12715, #24663, #37215, #9008, #21588 ),
 .UNSPECIFIED., .F., .F.,
 ( 4, 3, 3, 4 ),
 ( 0.0002170292169044746994, 0.0002420761345915958753, 0.0002723302478206996065, 0.0002816811360866696996 ),
 .UNSPECIFIED. ) ;
#14744 = CARTESIAN_POINT ( 'NONE',  ( -1.577774374486538678, -28.34370111728035013, 6.894806418505347700 ) ) ;
#14745 = CARTESIAN_POINT ( 'NONE',  ( 79.37669412903255761, 65.14038507876448136, 3.220356845321968198 ) ) ;
#14746 = CARTESIAN_POINT ( 'NONE',  ( 26.00408895386407693, 0.8598023161378668400, 4.425818499699599506 ) ) ;
#14748 = ORIENTED_EDGE ( 'NONE', *, *, #8317, .F. ) ;
#14747 = CARTESIAN_POINT ( 'NONE',  ( 4.764283036282700223, -27.89929580878658655, 7.780491323090172884 ) ) ;
#14749 = CARTESIAN_POINT ( 'NONE',  ( -2.954197855305039422, -12.43481156997016157, -4.000000000000000000 ) ) ;
#14750 = CARTESIAN_POINT ( 'NONE',  ( 73.81116006253010653, 62.20691382096257627, -3.564124015814260638 ) ) ;
#14751 = CARTESIAN_POINT ( 'NONE',  ( 3.217988213875103920, -32.61244741234136768, 6.979335674598004857 ) ) ;
#14752 =( BOUNDED_CURVE ( )  B_SPLINE_CURVE ( 3, ( #21503, #34081, #25196, #37727 ),
 .UNSPECIFIED., .F., .T. ) 
 B_SPLINE_CURVE_WITH_KNOTS ( ( 4, 4 ),
 ( 4.708531083176468179, 4.895802057644189631 ),
 .UNSPECIFIED. ) 
 CURVE ( )  GEOMETRIC_REPRESENTATION_ITEM ( )  RATIONAL_B_SPLINE_CURVE ( ( 1.000000000000000000, 0.9970795998553221295, 0.9970795998553221295, 1.000000000000000000 ) ) 
 REPRESENTATION_ITEM ( '' )  );
#14754 = DIRECTION ( 'NONE',  ( -0.000000000000000000, -0.000000000000000000, 1.000000000000000000 ) ) ;
#14753 = CARTESIAN_POINT ( 'NONE',  ( -57.21827861686057304, 30.45169051924667514, -3.625703664980399754 ) ) ;
#14755 = DIRECTION ( 'NONE',  ( 0.6502177225477915323, -0.3754033771448308521, 0.6605219282605377940 ) ) ;
#14756 = LINE ( 'NONE', #14551, #15621 ) ;
#14757 = CARTESIAN_POINT ( 'NONE',  ( -1.622027358445928158, -30.66236699258251264, 7.766640943994648438 ) ) ;
#14758 = CARTESIAN_POINT ( 'NONE',  ( 22.21474492361291908, 5.152987084292143471, -3.146772455935926693 ) ) ;
#14759 = ORIENTED_EDGE ( 'NONE', *, *, #8812, .T. ) ;
#14760 = CARTESIAN_POINT ( 'NONE',  ( -20.44874870218064444, -25.49307895267003587, 6.800000000000000711 ) ) ;
#14761 = CARTESIAN_POINT ( 'NONE',  ( 23.99854160108877110, 3.116918725036224025, -4.608611027060286247 ) ) ;
#14762 = CARTESIAN_POINT ( 'NONE',  ( -75.45330471031414277, 33.71485196875532608, -8.800414904976364028 ) ) ;
#14763 = VERTEX_POINT ( 'NONE', #40444 ) ;
#14764 = CARTESIAN_POINT ( 'NONE',  ( -70.92837670882107659, -65.19654454972992141, 6.000000000000002665 ) ) ;
#14765 = CARTESIAN_POINT ( 'NONE',  ( 81.16204935228437023, 61.30122352005683695, 1.083735637653854722 ) ) ;
#14766 = CARTESIAN_POINT ( 'NONE',  ( 85.00114435706898064, 2.071954908684588759, 4.651167869591634307 ) ) ;
#14767 = CARTESIAN_POINT ( 'NONE',  ( 17.03294222275471270, 9.497926725977514195, 2.806642516075366078 ) ) ;
#14768 = ORIENTED_EDGE ( 'NONE', *, *, #15097, .T. ) ;
#14769 = CARTESIAN_POINT ( 'NONE',  ( -70.92837670882107659, 3.729367930467589076, 0.000000000000000000 ) ) ;
#14770 = ORIENTED_EDGE ( 'NONE', *, *, #14435, .T. ) ;
#14771 = CIRCLE ( 'NONE', #14739, 0.1000000000000028644 ) ;
#14772 = AXIS2_PLACEMENT_3D ( 'NONE', #27135, #20344, #32923 ) ;
#14773 = CARTESIAN_POINT ( 'NONE',  ( 5.058102131368015009, -29.03535570872796967, 6.887041543973314361 ) ) ;
#14774 = CARTESIAN_POINT ( 'NONE',  ( 14.88813598356257195, -6.116304347389402984, -2.529251432410653422 ) ) ;
#14775 = EDGE_CURVE ( 'NONE', #7027, #33685, #10894, .T. ) ;
#14776 = CARTESIAN_POINT ( 'NONE',  ( 22.91741166320089818, 2.643276093639356006, -3.783214368374389291 ) ) ;
#14777 = DIRECTION ( 'NONE',  ( -0.6662082868431838945, 0.000000000000000000, -0.7457657263118692148 ) ) ;
#14778 = VECTOR ( 'NONE', #3025, 1000.000000000000000 ) ;
#14779 = CARTESIAN_POINT ( 'NONE',  ( -0.3903772972505400451, -26.88875661219547553, 7.754798119455333705 ) ) ;
#14780 = VERTEX_POINT ( 'NONE', #12253 ) ;
#14781 = CARTESIAN_POINT ( 'NONE',  ( 2.859730186744443348, -32.85857677678156819, 7.783750581861600182 ) ) ;
#14782 = AXIS2_PLACEMENT_3D ( 'NONE', #5548, #3260, #8416 ) ;
#14783 = CARTESIAN_POINT ( 'NONE',  ( -1.216810142391697047, -27.82351944452216586, 6.889465824494253710 ) ) ;
#14784 = EDGE_LOOP ( 'NONE', ( #32644, #5404, #32326, #27661, #32767 ) ) ;
#14785 = VERTEX_POINT ( 'NONE', #34729 ) ;
#14787 = CARTESIAN_POINT ( 'NONE',  ( 33.94748962458718466, -0.4853907904003012530, 5.118178450053537887 ) ) ;
#14786 = CARTESIAN_POINT ( 'NONE',  ( 80.61469348477538688, 64.03810969304559819, -3.562450064734663524 ) ) ;
#14788 = CARTESIAN_POINT ( 'NONE',  ( -1.332155549108038795, -31.29987003238072418, 7.778495531946297170 ) ) ;
#14789 = CARTESIAN_POINT ( 'NONE',  ( 14.61802081865039682, 12.48098255133728784, -2.499999999999999556 ) ) ;
#14790 = LINE ( 'NONE', #27359, #23108 ) ;
#14791 = CARTESIAN_POINT ( 'NONE',  ( -16.87867591359218977, -26.64985754041175525, 6.700000000000000178 ) ) ;
#14792 = ORIENTED_EDGE ( 'NONE', *, *, #7675, .F. ) ;
#14793 = ORIENTED_EDGE ( 'NONE', *, *, #13852, .T. ) ;
#14794 = LINE ( 'NONE', #27364, #6909 ) ;
#14795 = CARTESIAN_POINT ( 'NONE',  ( 80.91556171499746597, 62.42588715431494961, -3.188730975143399871 ) ) ;
#14796 = B_SPLINE_CURVE_WITH_KNOTS ( 'NONE', 3,
 ( #36549, #14305, #26680, #33486, #20902, #5464, #11410, #36153, #30168, #24398, #18004, #8118, #17797, #17189, #14923, #30383, #27492, #29964, #21115, #23589, #1571, #20690, #33273, #1775 ),
 .UNSPECIFIED., .F., .F.,
 ( 4, 1, 1, 1, 1, 1, 1, 2, 2, 1, 1, 1, 1, 1, 1, 2, 2, 4 ),
 ( 0.000000000000000000, 0.2499999999999679146, 0.3749999999999522049, 0.4374999999999445999, 0.4687499999999411027, 0.4843749999999393818, 0.4921874999999382716, 0.4960937499999385492, 0.4999999999999388267, 0.6249999999999987788, 0.6875000000000288658, 0.7187500000000447420, 0.7343750000000527356, 0.7421875000000558442, 0.7460937500000575096, 0.7480468750000581757, 0.7500000000000589528, 1.000000000000000000 ),
 .UNSPECIFIED. ) ;
#14797 = DIRECTION ( 'NONE',  ( -0.000000000000000000, -0.000000000000000000, -1.000000000000000000 ) ) ;
#14798 = VERTEX_POINT ( 'NONE', #133 ) ;
#14799 = EDGE_CURVE ( 'NONE', #8440, #34705, #21332, .T. ) ;
#14801 = CARTESIAN_POINT ( 'NONE',  ( 4.282520317648695674, -27.35800574660165196, 7.712764235869103757 ) ) ;
#14800 =( LENGTH_UNIT ( ) NAMED_UNIT ( * ) SI_UNIT ( .MILLI., .METRE. ) );
#14802 = ORIENTED_EDGE ( 'NONE', *, *, #20208, .T. ) ;
#14803 = CARTESIAN_POINT ( 'NONE',  ( 81.16877391194421421, 61.30368580354083008, -1.027726681410897625 ) ) ;
#14804 = AXIS2_PLACEMENT_3D ( 'NONE', #17055, #35628, #22860 ) ;
#14805 = VECTOR ( 'NONE', #33813, 1000.000000000000114 ) ;
#14806 = DIRECTION ( 'NONE',  ( 1.000000000000000000, 0.000000000000000000, 0.000000000000000000 ) ) ;
#14808 = CARTESIAN_POINT ( 'NONE',  ( 17.64783264544855257, -2.926693510814210697, -2.960769117404401740 ) ) ;
#14807 = CARTESIAN_POINT ( 'NONE',  ( -0.02491320616155640738, -26.64019694052143805, 7.730758795053802146 ) ) ;
#14809 = CARTESIAN_POINT ( 'NONE',  ( -1.794668156065684084, -29.38400591384104032, 6.921725064902950031 ) ) ;
#14810 = CARTESIAN_POINT ( 'NONE',  ( 75.07588875331117606, 60.93231399735385878, 3.896954863271551162 ) ) ;
#14811 = ORIENTED_EDGE ( 'NONE', *, *, #14620, .T. ) ;
#14812 = CARTESIAN_POINT ( 'NONE',  ( 23.49894466845412566, 3.019249802179449826, -3.929487204937235134 ) ) ;
#14813 = CARTESIAN_POINT ( 'NONE',  ( 4.200390093233091093, -29.56993018339339940, -8.199999999999999289 ) ) ;
#14814 = AXIS2_PLACEMENT_3D ( 'NONE', #35882, #27755, #36824 ) ;
#14815 = EDGE_CURVE ( 'NONE', #26672, #38094, #3748, .T. ) ;
#14816 = CARTESIAN_POINT ( 'NONE',  ( -0.02262473055865150268, -26.52342071894167574, 6.894806418505347700 ) ) ;
#14817 = FACE_OUTER_BOUND ( 'NONE', #30889, .T. ) ;
#14818 = ORIENTED_EDGE ( 'NONE', *, *, #35359, .F. ) ;
#14819 = PLANE ( 'NONE',  #12292 ) ;
#14820 = CARTESIAN_POINT ( 'NONE',  ( 81.98790212893285911, 62.35967063417187717, 2.110636331688407807 ) ) ;
#14821 = CARTESIAN_POINT ( 'NONE',  ( 86.83829259450851623, 0.8168327605515373069, 4.998615091244022146 ) ) ;
#14822 = CARTESIAN_POINT ( 'NONE',  ( 5.129509330119056187, -30.27076478451887809, 6.864216812888783714 ) ) ;
#14823 = CARTESIAN_POINT ( 'NONE',  ( -1.766085975226569404, -30.05319374170961666, 7.750000000000000888 ) ) ;
#14824 = DIRECTION ( 'NONE',  ( -0.000000000000000000, -0.000000000000000000, -1.000000000000000000 ) ) ;
#14825 = CARTESIAN_POINT ( 'NONE',  ( 14.85476021617353304, -4.543106551388008896, 2.514844559792396517 ) ) ;
#14826 = CARTESIAN_POINT ( 'NONE',  ( -0.009460099485995122209, -26.51599940587959381, 6.880608371227948439 ) ) ;
#14827 = EDGE_CURVE ( 'NONE', #10700, #22883, #14935, .T. ) ;
#14828 = CARTESIAN_POINT ( 'NONE',  ( 36.42092789943291820, -3.115845811384692077, -5.890764660813112563 ) ) ;
#14829 = CARTESIAN_POINT ( 'NONE',  ( -27.07867591359219972, -24.55319635012989110, 6.800000000000000711 ) ) ;
#14830 = DIRECTION ( 'NONE',  ( -0.000000000000000000, -0.000000000000000000, 1.000000000000000000 ) ) ;
#14831 = DIRECTION ( 'NONE',  ( -0.000000000000000000, -0.000000000000000000, 1.000000000000000000 ) ) ;
#14832 = DIRECTION ( 'NONE',  ( 0.000000000000000000, 0.000000000000000000, 1.000000000000000000 ) ) ;
#14833 = DIRECTION ( 'NONE',  ( 1.000000000000000000, 0.000000000000000000, 0.000000000000000000 ) ) ;
#14834 = CIRCLE ( 'NONE', #7619, 0.1000000000000028644 ) ;
#14835 = VERTEX_POINT ( 'NONE', #12036 ) ;
#14836 = CARTESIAN_POINT ( 'NONE',  ( 35.83209424069072924, -3.726939881646061270, 5.625185406441244318 ) ) ;
#14837 = CARTESIAN_POINT ( 'NONE',  ( -71.45635794260526552, 0.07346082103169225552, 3.977567636976454768 ) ) ;
#14838 = CARTESIAN_POINT ( 'NONE',  ( 66.97346358352143625, 58.09330026553017490, -3.997553359131193584 ) ) ;
#14839 = CIRCLE ( 'NONE', #36546, 0.1000000000000028644 ) ;
#14840 = ADVANCED_FACE ( 'NONE', ( #30814 ), #37169, .F. ) ;
#14841 = PLANE ( 'NONE',  #25352 ) ;
#14842 = ORIENTED_EDGE ( 'NONE', *, *, #20828, .T. ) ;
#14843 = DIRECTION ( 'NONE',  ( 0.7660444431189790127, 0.6427876096865381417, 0.000000000000000000 ) ) ;
#14844 = CARTESIAN_POINT ( 'NONE',  ( -80.32062948810629166, -6.645441929077266607, -3.458186301391593886 ) ) ;
#14845 = CARTESIAN_POINT ( 'NONE',  ( 76.46985044344074822, 64.49630587417807703, 2.565399245510498361 ) ) ;
#14846 = DIRECTION ( 'NONE',  ( -0.000000000000000000, -1.000000000000000000, -0.000000000000000000 ) ) ;
#14847 = ORIENTED_EDGE ( 'NONE', *, *, #17643, .F. ) ;
#14848 = DIRECTION ( 'NONE',  ( 1.000000000000000000, 0.000000000000000000, 0.000000000000000000 ) ) ;
#14849 = CARTESIAN_POINT ( 'NONE',  ( 3.559755418260376114, -26.72339534466646427, 7.013842709614101167 ) ) ;
#14850 = ORIENTED_EDGE ( 'NONE', *, *, #8540, .F. ) ;
#14851 = CARTESIAN_POINT ( 'NONE',  ( 22.19529100421578960, 5.229607391819558693, 3.102197625450730634 ) ) ;
#14852 = CARTESIAN_POINT ( 'NONE',  ( 82.18775271763095702, 62.23297483488567394, -1.085061034363232979 ) ) ;
#14853 = CARTESIAN_POINT ( 'NONE',  ( 79.79114114151838066, 64.70569453017795070, 3.482375488376185935 ) ) ;
#14854 = CARTESIAN_POINT ( 'NONE',  ( -72.45330471031414277, 33.71485196875532608, 15.50000000000000000 ) ) ;
#14855 = EDGE_LOOP ( 'NONE', ( #16179, #39607, #32940, #17836 ) ) ;
#14856 = CARTESIAN_POINT ( 'NONE',  ( 77.88532341798189407, 63.74564772441265603, -3.640295653904956907 ) ) ;
#14858 = CARTESIAN_POINT ( 'NONE',  ( 14.75808067079221431, -5.143087478482986974, -2.500015154099217707 ) ) ;
#14857 = CARTESIAN_POINT ( 'NONE',  ( 21.97060183119601007, 0.2202240153287075564, 7.735562088727589547 ) ) ;
#14859 = EDGE_CURVE ( 'NONE', #31349, #8999, #30462, .T. ) ;
#14860 = ADVANCED_FACE ( 'NONE', ( #13477 ), #16754, .F. ) ;
#14861 = CARTESIAN_POINT ( 'NONE',  ( 79.58537830806109525, 65.88021587146388924, -2.518708746843062229 ) ) ;
#14862 = CARTESIAN_POINT ( 'NONE',  ( 77.90798433017856439, 65.01733068894688472, 2.764360460937555164 ) ) ;
#14863 = EDGE_LOOP ( 'NONE', ( #3068, #38342, #2136, #4890 ) ) ;
#14864 = EDGE_CURVE ( 'NONE', #30246, #7186, #15346, .T. ) ;
#14865 = CARTESIAN_POINT ( 'NONE',  ( -0.9263124491650691628, -27.41112496668761622, 7.712764235869100204 ) ) ;
#14866 = CARTESIAN_POINT ( 'NONE',  ( 78.99269976270093707, 66.20980237122186907, 1.093381982072756164 ) ) ;
#14868 = CARTESIAN_POINT ( 'NONE',  ( -1.695213279257311800, -29.39707840662554617, 6.882085323592685100 ) ) ;
#14867 = DIRECTION ( 'NONE',  ( -0.000000000000000000, -0.000000000000000000, 1.000000000000000000 ) ) ;
#14869 = CARTESIAN_POINT ( 'NONE',  ( 30.37020714367901775, -0.1410433206546675144, -5.583699017444894608 ) ) ;
#14870 = CIRCLE ( 'NONE', #12947, 0.1000000000000028644 ) ;
#14871 = CARTESIAN_POINT ( 'NONE',  ( -1.770976519370218494, -30.01676597940898361, 6.887547729233690852 ) ) ;
#14872 = DIRECTION ( 'NONE',  ( 1.000000000000000000, 0.000000000000000000, 0.000000000000000000 ) ) ;
#14873 = CARTESIAN_POINT ( 'NONE',  ( 1.616163289117390711, -33.06891658597750450, 6.865554069792297653 ) ) ;
#14874 = CARTESIAN_POINT ( 'NONE',  ( 24.12552690779179798, 0.5099362638223552402, -5.092848330633646725 ) ) ;
#14875 = AXIS2_PLACEMENT_3D ( 'NONE', #16892, #29472, #13820 ) ;
#14876 = CARTESIAN_POINT ( 'NONE',  ( 6.119163499495797964, -31.21649665547238683, 7.695279973900954751 ) ) ;
#14877 = PLANE ( 'NONE',  #4671 ) ;
#14878 = DIRECTION ( 'NONE',  ( -0.1736481776669206722, -0.9848077530122096857, -0.000000000000000000 ) ) ;
#14879 = CARTESIAN_POINT ( 'NONE',  ( -71.12492995964747422, -48.60730761282789558, 9.998528757544843160 ) ) ;
#14880 = EDGE_CURVE ( 'NONE', #8831, #36530, #36274, .T. ) ;
#14881 = CARTESIAN_POINT ( 'NONE',  ( 34.79194643261769926, -3.831294807337672914, -5.380493905816994271 ) ) ;
#14882 = CARTESIAN_POINT ( 'NONE',  ( 30.84634820625675644, -3.378268544268043350, -4.954352808572474842 ) ) ;
#14883 = FACE_OUTER_BOUND ( 'NONE', #24759, .T. ) ;
#14884 = DIRECTION ( 'NONE',  ( 1.000000000000000000, -0.000000000000000000, -0.000000000000000000 ) ) ;
#14885 = EDGE_CURVE ( 'NONE', #38704, #14835, #13272, .T. ) ;
#14886 = CARTESIAN_POINT ( 'NONE',  ( 0.4527547210032973890, -32.82408303185094667, 7.785593909369613819 ) ) ;
#14887 = DIRECTION ( 'NONE',  ( 0.000000000000000000, 0.000000000000000000, -1.000000000000000000 ) ) ;
#14888 = CARTESIAN_POINT ( 'NONE',  ( -74.02422384641097608, 6.646861260247477254, 10.77237409516136424 ) ) ;
#14889 = CARTESIAN_POINT ( 'NONE',  ( 4.915490139096653444, -28.46397733851794243, 7.785172627573962778 ) ) ;
#14890 = CARTESIAN_POINT ( 'NONE',  ( 14.77222818450456643, -4.461908109758233820, -2.511961494517393145 ) ) ;
#14891 = CARTESIAN_POINT ( 'NONE',  ( 22.53677427111851372, 1.671346796043067462, -5.585631968908431944 ) ) ;
#14892 = CYLINDRICAL_SURFACE ( 'NONE', #8688, 0.1000000000000028644 ) ;
#14893 = ORIENTED_EDGE ( 'NONE', *, *, #32505, .T. ) ;
#14894 = ORIENTED_EDGE ( 'NONE', *, *, #19980, .F. ) ;
#14895 = PLANE ( 'NONE',  #23871 ) ;
#14896 = CARTESIAN_POINT ( 'NONE',  ( 69.84993430378905543, 58.85661355152254970, -3.977789803233258148 ) ) ;
#14897 = EDGE_CURVE ( 'NONE', #17894, #5789, #16002, .T. ) ;
#14898 = AXIS2_PLACEMENT_3D ( 'NONE', #13521, #26092, #33281 ) ;
#14899 = EDGE_LOOP ( 'NONE', ( #38795, #6998, #40700, #11009 ) ) ;
#14900 = CARTESIAN_POINT ( 'NONE',  ( 87.05329302184628659, -1.423768201249274945, 4.835531253876708568 ) ) ;
#14901 = LINE ( 'NONE', #14491, #23245 ) ;
#14902 = CARTESIAN_POINT ( 'NONE',  ( 3.052029408395551702, -26.45014314551610823, 6.988553391373223178 ) ) ;
#14903 = CIRCLE ( 'NONE', #6375, 0.9999999999999971134 ) ;
#14905 = CARTESIAN_POINT ( 'NONE',  ( 1.160481914523016078, -26.21307075903531114, 6.892063359921932530 ) ) ;
#14904 = CARTESIAN_POINT ( 'NONE',  ( -0.9051507792758500814, -27.23301838324232449, 6.865482280155367434 ) ) ;
#14906 = VECTOR ( 'NONE', #13308, 1000.000000000000114 ) ;
#14907 = CONTEXT_DEPENDENT_SHAPE_REPRESENTATION ( #20799, #12483 ) ;
#14908 = EDGE_CURVE ( 'NONE', #12529, #34454, #940, .T. ) ;
#14909 = VECTOR ( 'NONE', #8601, 1000.000000000000000 ) ;
#14910 = FACE_OUTER_BOUND ( 'NONE', #18278, .T. ) ;
#14911 = ORIENTED_EDGE ( 'NONE', *, *, #23703, .F. ) ;
#14912 = CARTESIAN_POINT ( 'NONE',  ( 22.61586509580334337, 4.626878386862768089, 3.038062468280299022 ) ) ;
#14913 = FILL_AREA_STYLE ('',( #21717 ) ) ;
#14914 = CARTESIAN_POINT ( 'NONE',  ( 22.16976678648915922, -3.079849535211031331, 3.569519670046482407 ) ) ;
#14915 = EDGE_CURVE ( 'NONE', #34445, #25426, #22602, .T. ) ;
#14916 = EDGE_LOOP ( 'NONE', ( #27546, #21714, #5139, #10655 ) ) ;
#14917 = CARTESIAN_POINT ( 'NONE',  ( 78.54017873204453792, 65.73972836631979533, -2.148686496494745857 ) ) ;
#14918 = CARTESIAN_POINT ( 'NONE',  ( 17.02720468749124905, 12.19482429969091619, -2.499999999999998668 ) ) ;
#14919 = CARTESIAN_POINT ( 'NONE',  ( 81.81758241818907607, 62.27516227682815497, -2.299173245602590399 ) ) ;
#14920 = CARTESIAN_POINT ( 'NONE',  ( 78.49831277043062983, 65.85142261852138290, 1.827177995460262716 ) ) ;
#14921 = ADVANCED_FACE ( 'NONE', ( #22563 ), #7300, .T. ) ;
#14922 = CARTESIAN_POINT ( 'NONE',  ( 22.91153608851413637, 3.594015725306300979, 3.782297342843620847 ) ) ;
#14923 = CARTESIAN_POINT ( 'NONE',  ( 17.53293928993041106, 14.12932500356599164, 2.499999999999999556 ) ) ;
#14924 = CARTESIAN_POINT ( 'NONE',  ( 21.85643539959774273, 9.214175136349357587, -0.8338435668127727185 ) ) ;
#14925 = EDGE_LOOP ( 'NONE', ( #17775, #34575, #35100, #803, #17799 ) ) ;
#14926 = CARTESIAN_POINT ( 'NONE',  ( -76.92986009040373574, 10.85203011506569304, 8.001236914947885026 ) ) ;
#14927 = CARTESIAN_POINT ( 'NONE',  ( -1.799419790741071168, -29.60642027013681599, 7.697588729724128775 ) ) ;
#14928 = CARTESIAN_POINT ( 'NONE',  ( 3.198709474042557233, -25.09719924859204454, 7.754798119455333705 ) ) ;
#14929 = CIRCLE ( 'NONE', #24820, 7.744449365083023729 ) ;
#14930 = CARTESIAN_POINT ( 'NONE',  ( -74.64436830331966632, 7.527181902581737916, -9.332964955005275343 ) ) ;
#14931 = CARTESIAN_POINT ( 'NONE',  ( 1.513399906207050449, -32.96478432900200062, 7.013842709614101167 ) ) ;
#14932 = DIRECTION ( 'NONE',  ( -0.000000000000000000, -0.000000000000000000, -1.000000000000000000 ) ) ;
#14933 = CARTESIAN_POINT ( 'NONE',  ( -1.739611863387223512, -30.14058980792885123, 7.783750581861600182 ) ) ;
#14934 = CARTESIAN_POINT ( 'NONE',  ( 14.98917483460526512, 12.12204619583915566, 2.538718705410484500 ) ) ;
#14935 = LINE ( 'NONE', #5680, #10723 ) ;
#14936 = CARTESIAN_POINT ( 'NONE',  ( 0.5925143926836328179, -26.24988255990380281, 6.863805608295729499 ) ) ;
#14937 = VECTOR ( 'NONE', #39200, 1000.000000000000000 ) ;
#14938 = CARTESIAN_POINT ( 'NONE',  ( 5.065770593663160071, -29.08591650778173587, 7.768425012602593327 ) ) ;
#14939 = CIRCLE ( 'NONE', #20845, 0.1000000000000028644 ) ;
#14940 = DIRECTION ( 'NONE',  ( 0.000000000000000000, 0.000000000000000000, 1.000000000000000000 ) ) ;
#14941 = CARTESIAN_POINT ( 'NONE',  ( 87.24249188000140975, 0.3628169386305434840, 4.705374253625543624 ) ) ;
#14942 = CARTESIAN_POINT ( 'NONE',  ( 24.72992518470875112, 2.633077311188870340, -3.926889863206841191 ) ) ;
#14943 = ORIENTED_EDGE ( 'NONE', *, *, #8758, .T. ) ;
#14944 = CARTESIAN_POINT ( 'NONE',  ( 67.84886183593677345, 57.97047572268562021, 3.979762160777300828 ) ) ;
#14945 = CARTESIAN_POINT ( 'NONE',  ( 36.66725829508891366, -2.423845347316893939, 5.929210476578201217 ) ) ;
#14946 = CARTESIAN_POINT ( 'NONE',  ( 4.993499329952471477, -30.75545037259727366, 7.756742906098588186 ) ) ;
#14947 = ADVANCED_FACE ( 'NONE', ( #3843 ), #16360, .F. ) ;
#14948 = CARTESIAN_POINT ( 'NONE',  ( -34.87867591359218977, -26.64985754041175525, 6.700000000000000178 ) ) ;
#14949 = CARTESIAN_POINT ( 'NONE',  ( 86.10913233486274976, 1.283334762834210441, -5.698406565159564785 ) ) ;
#14950 = CARTESIAN_POINT ( 'NONE',  ( 4.865842863122197492, -30.81086078644958093, 6.870716933885666400 ) ) ;
#14951 = CARTESIAN_POINT ( 'NONE',  ( -1.555661392733006965, -30.54877068150224417, 6.903372536218459921 ) ) ;
#14952 = ORIENTED_EDGE ( 'NONE', *, *, #3447, .T. ) ;
#14953 = CARTESIAN_POINT ( 'NONE',  ( -1.607612949201309815, -28.78435332836398075, 6.997764925645182821 ) ) ;
#14954 = CYLINDRICAL_SURFACE ( 'NONE', #23915, 0.1000000000000028644 ) ;
#14955 = CARTESIAN_POINT ( 'NONE',  ( -0.6365217069179813780, -32.17547105590234224, 6.865482280155367434 ) ) ;
#14956 = ORIENTED_EDGE ( 'NONE', *, *, #29478, .T. ) ;
#14957 = CARTESIAN_POINT ( 'NONE',  ( -70.60020594839741648, -21.73402473355089271, 3.991851897078962708 ) ) ;
#14958 = EDGE_LOOP ( 'NONE', ( #35660, #25759, #22184, #18079 ) ) ;
#14959 = VERTEX_POINT ( 'NONE', #22964 ) ;
#14960 = CARTESIAN_POINT ( 'NONE',  ( 79.92041472187213458, 64.04075560556069036, -3.697630003121160858 ) ) ;
#14961 = CARTESIAN_POINT ( 'NONE',  ( -73.16330946177717465, -60.53509472482661380, 3.871017079619767376 ) ) ;
#14962 = CARTESIAN_POINT ( 'NONE',  ( -1.519540497997595052, -28.19804604943728421, 6.925313231306334139 ) ) ;
#14963 = VECTOR ( 'NONE', #13366, 1000.000000000000000 ) ;
#14964 = CARTESIAN_POINT ( 'NONE',  ( 79.03702048636715460, 65.49184929578454728, 2.818206040476803231 ) ) ;
#14966 = ORIENTED_EDGE ( 'NONE', *, *, #30612, .F. ) ;
#14965 = CARTESIAN_POINT ( 'NONE',  ( 4.744157865074793534, -27.87191509600810946, 7.785344483711591934 ) ) ;
#14967 = VECTOR ( 'NONE', #9804, 1000.000000000000000 ) ;
#14968 = EDGE_CURVE ( 'NONE', #23776, #17087, #18612, .T. ) ;
#14969 = ADVANCED_FACE ( 'NONE', ( #33240 ), #32640, .T. ) ;
#14970 = CARTESIAN_POINT ( 'NONE',  ( 73.70000790436553473, 62.44749314232891635, -3.395557233589456381 ) ) ;
#14972 = EDGE_CURVE ( 'NONE', #23738, #1317, #30143, .T. ) ;
#14971 = DIRECTION ( 'NONE',  ( 0.000000000000000000, 0.000000000000000000, 1.000000000000000000 ) ) ;
#14974 = CARTESIAN_POINT ( 'NONE',  ( 4.938390203311415748E-15, -42.37473357531882101, 6.000000000000000000 ) ) ;
#14973 = CARTESIAN_POINT ( 'NONE',  ( 4.978554560952730412, -30.79615924950642025, 6.894806418505347700 ) ) ;
#14975 = CARTESIAN_POINT ( 'NONE',  ( -38.87867591359218977, -26.64985754041175525, 6.700000000000000178 ) ) ;
#14976 = DIRECTION ( 'NONE',  ( -0.000000000000000000, 0.000000000000000000, 1.000000000000000000 ) ) ;
#14977 = CARTESIAN_POINT ( 'NONE',  ( 23.73069679916937602, 3.541948203740225232, -3.238583379989644850 ) ) ;
#14978 = EDGE_LOOP ( 'NONE', ( #15735, #34718, #7477, #2061, #21652, #12091 ) ) ;
#14979 = CYLINDRICAL_SURFACE ( 'NONE', #29462, 3.000000000000002665 ) ;
#14980 = CARTESIAN_POINT ( 'NONE',  ( 24.33615536228354514, 0.1518143133650739496, -6.924920736309362113 ) ) ;
#14981 = CARTESIAN_POINT ( 'NONE',  ( 2.882188420740142920, -32.75793850981484212, 7.643333865083957512 ) ) ;
#14982 = CARTESIAN_POINT ( 'NONE',  ( 1.020706351875211304, -32.99074525956162773, 7.782861076432729952 ) ) ;
#14983 = CARTESIAN_POINT ( 'NONE',  ( 80.32731820217895802, 65.01876230294769243, 3.279590910093583389 ) ) ;
#14984 = CARTESIAN_POINT ( 'NONE',  ( 84.44530234979703209, 2.765803402995568927, 2.732740112990733383 ) ) ;
#14985 = CARTESIAN_POINT ( 'NONE',  ( -1.799471907747695942, -29.53885005966835919, 6.894806418505347700 ) ) ;
#14986 = ORIENTED_EDGE ( 'NONE', *, *, #28741, .T. ) ;
#14987 = AXIS2_PLACEMENT_3D ( 'NONE', #29166, #25874, #31856 ) ;
#14988 = DIRECTION ( 'NONE',  ( 0.000000000000000000, 0.000000000000000000, 1.000000000000000000 ) ) ;
#14989 = CARTESIAN_POINT ( 'NONE',  ( -70.92837670882107659, -45.61702805680359063, 10.00000000000000888 ) ) ;
#14990 = VECTOR ( 'NONE', #26398, 1000.000000000000000 ) ;
#14991 = LINE ( 'NONE', #9011, #13183 ) ;
#14992 = CARTESIAN_POINT ( 'NONE',  ( 23.82764572543298698, -2.864586094091185586, -3.920064517359787892 ) ) ;
#14993 = CYLINDRICAL_SURFACE ( 'NONE', #38565, 79.54614097552274643 ) ;
#14994 = LINE ( 'NONE', #15194, #30589 ) ;
#14995 = CARTESIAN_POINT ( 'NONE',  ( 1.887380280259158383, -26.17507603778478753, 7.013842709614101167 ) ) ;
#14996 = CARTESIAN_POINT ( 'NONE',  ( 33.46307027370517062, -3.080941673966315797, 5.429119442261287176 ) ) ;
#14997 = CARTESIAN_POINT ( 'NONE',  ( 88.10293741339057760, -0.6036763236807990429, 2.641732887311516453 ) ) ;
#14998 = ORIENTED_EDGE ( 'NONE', *, *, #24174, .F. ) ;
#14999 = EDGE_LOOP ( 'NONE', ( #25, #1844, #358, #4061 ) ) ;
#15001 = CARTESIAN_POINT ( 'NONE',  ( 36.49386420176196566, -3.561635646996995419, 5.795649267797439386 ) ) ;
#15000 = CARTESIAN_POINT ( 'NONE',  ( 79.39921707337093437, 65.76781561079134519, -2.628317182735761204 ) ) ;
#15002 = CARTESIAN_POINT ( 'NONE',  ( 26.15460830059191011, -2.761060381110045814, 4.288457195536199862 ) ) ;
#15003 = CARTESIAN_POINT ( 'NONE',  ( 17.86011303457873467, -3.180593380899296108, -2.952765578688846038 ) ) ;
#15004 = PLANE ( 'NONE',  #33637 ) ;
#15005 = ORIENTED_EDGE ( 'NONE', *, *, #19261, .F. ) ;
#15006 = DIRECTION ( 'NONE',  ( 0.000000000000000000, 0.000000000000000000, 1.000000000000000000 ) ) ;
#15007 = ORIENTED_EDGE ( 'NONE', *, *, #25306, .F. ) ;
#15008 = ORIENTED_EDGE ( 'NONE', *, *, #7794, .T. ) ;
#15009 = CARTESIAN_POINT ( 'NONE',  ( 0.01209709964644558461, -32.52114463981743597, 7.635761828346577573 ) ) ;
#15010 = CARTESIAN_POINT ( 'NONE',  ( 78.64903117394807452, 66.02922079195218430, -1.215327096190493616 ) ) ;
#15011 =( BOUNDED_CURVE ( )  B_SPLINE_CURVE ( 3, ( #34226, #21445, #5792, #18329 ),
 .UNSPECIFIED., .F., .T. ) 
 B_SPLINE_CURVE_WITH_KNOTS ( ( 4, 4 ),
 ( 4.748221474220559735, 4.941946782021394036 ),
 .UNSPECIFIED. ) 
 CURVE ( )  GEOMETRIC_REPRESENTATION_ITEM ( )  RATIONAL_B_SPLINE_CURVE ( ( 1.000000000000000000, 0.9968749865767494445, 0.9968749865767494445, 1.000000000000000000 ) ) 
 REPRESENTATION_ITEM ( '' )  );
#15012 = CARTESIAN_POINT ( 'NONE',  ( -58.76908243668979281, 27.83904476269671235, -5.922484465878603999 ) ) ;
#15014 = CARTESIAN_POINT ( 'NONE',  ( 31.35971567531513315, 0.5160385187742575486, 4.592137409821144267 ) ) ;
#15013 = CARTESIAN_POINT ( 'NONE',  ( 24.06016172912751472, 2.745221661300574656, 3.954363946542386987 ) ) ;
#15015 = ORIENTED_EDGE ( 'NONE', *, *, #1494, .T. ) ;
#15016 = CARTESIAN_POINT ( 'NONE',  ( 78.97185648144787251, 66.19841638340299994, -1.173033592341553355 ) ) ;
#15017 = ADVANCED_FACE ( 'NONE', ( #2157 ), #17351, .F. ) ;
#15019 = EDGE_CURVE ( 'NONE', #30682, #26162, #4831, .T. ) ;
#15018 = DIRECTION ( 'NONE',  ( -0.5751513419797927851, 0.4826092789263599636, -0.6605219282605403475 ) ) ;
#15020 = EDGE_LOOP ( 'NONE', ( #31692, #13502, #31833, #8616, #39892 ) ) ;
#15022 = DIRECTION ( 'NONE',  ( 0.000000000000000000, -1.000000000000000000, 0.000000000000000000 ) ) ;
#15021 = CARTESIAN_POINT ( 'NONE',  ( 3.343728876470205336, -32.65988526930982516, 7.754798119455333705 ) ) ;
#15023 = CARTESIAN_POINT ( 'NONE',  ( -1.798839535641747034, -29.49580759126772023, 6.867280401193707640 ) ) ;
#15024 = CARTESIAN_POINT ( 'NONE',  ( 74.08781496033066105, 60.06802034872734453, 3.841642203975295544 ) ) ;
#15025 = CARTESIAN_POINT ( 'NONE',  ( 23.72685993228412471, 2.962434847395911230, -3.894494263829419545 ) ) ;
#15026 = ORIENTED_EDGE ( 'NONE', *, *, #22486, .T. ) ;
#15027 = VECTOR ( 'NONE', #33075, 1000.000000000000227 ) ;
#15028 = CARTESIAN_POINT ( 'NONE',  ( 21.85643539959781023, -13.06032977194142930, 9.178732910485948082 ) ) ;
#15029 = FACE_BOUND ( 'NONE', #9586, .T. ) ;
#15030 = ORIENTED_EDGE ( 'NONE', *, *, #14666, .T. ) ;
#15031 = DIRECTION ( 'NONE',  ( -0.9396926207859104263, 0.3420201433256631063, -0.000000000000000000 ) ) ;
#15032 = VERTEX_POINT ( 'NONE', #26847 ) ;
#15033 = CARTESIAN_POINT ( 'NONE',  ( 79.63061436091763312, 66.14207560456347323, 2.046910133536372634 ) ) ;
#15034 = CARTESIAN_POINT ( 'NONE',  ( 87.34032947353671261, 0.2529211099193515166, 5.122688537971352929 ) ) ;
#15035 = CARTESIAN_POINT ( 'NONE',  ( 5.128444259610362543, -30.27593629695848421, 6.864216812847430127 ) ) ;
#15036 = CARTESIAN_POINT ( 'NONE',  ( 2.718906344516694329, -32.91845592554787459, 6.980586498568968068 ) ) ;
#15037 = CARTESIAN_POINT ( 'NONE',  ( 0.6162842664679426541, -26.34739786293889807, 6.870716933885664623 ) ) ;
#15038 = CARTESIAN_POINT ( 'NONE',  ( -1.699609906766908374, -29.77250410202202602, 7.176074147390429481 ) ) ;
#15039 = AXIS2_PLACEMENT_3D ( 'NONE', #38914, #25978, #13815 ) ;
#15040 = CARTESIAN_POINT ( 'NONE',  ( 36.91185272694033870, -2.638231765404660312, -5.967385353207440346 ) ) ;
#15041 = FACE_OUTER_BOUND ( 'NONE', #35153, .T. ) ;
#15042 = CARTESIAN_POINT ( 'NONE',  ( 5.197249530360846137, -29.57011687675261413, 7.767441775592068609 ) ) ;
#15043 = DIRECTION ( 'NONE',  ( -0.8660254037844261621, -0.5000000000000215383, 0.000000000000000000 ) ) ;
#15044 = EDGE_CURVE ( 'NONE', #32450, #5814, #19931, .T. ) ;
#15045 = CARTESIAN_POINT ( 'NONE',  ( 2.410368835147195021, -26.24488429107400478, 7.754798119455333705 ) ) ;
#15046 = CARTESIAN_POINT ( 'NONE',  ( -69.42837670882104817, -46.91912102050241629, 5.809475019311127753 ) ) ;
#15047 = ORIENTED_EDGE ( 'NONE', *, *, #33353, .F. ) ;
#15048 = CARTESIAN_POINT ( 'NONE',  ( 37.15673189557763578, -2.580998988453131027, 5.983779168937476634 ) ) ;
#15049 = B_SPLINE_CURVE_WITH_KNOTS ( 'NONE', 3,
 ( #5861, #6063, #31588, #3412 ),
 .UNSPECIFIED., .F., .F.,
 ( 4, 4 ),
 ( 0.000000000000000000, 0.6850855086804076288 ),
 .UNSPECIFIED. ) ;
#15050 = DIRECTION ( 'NONE',  ( -0.000000000000000000, -0.000000000000000000, -1.000000000000000000 ) ) ;
#15051 = CARTESIAN_POINT ( 'NONE',  ( 67.03255446809592399, 57.93006272621622088, -3.998453671246410934 ) ) ;
#15052 = CARTESIAN_POINT ( 'NONE',  ( -0.4545477510665002496, -26.81228124332190532, 7.754798119455333705 ) ) ;
#15053 = CARTESIAN_POINT ( 'NONE',  ( -62.81463675898083210, 36.67811266762162603, 4.600311178732273021 ) ) ;
#15054 = EDGE_CURVE ( 'NONE', #6497, #1317, #10735, .T. ) ;
#15055 = ORIENTED_EDGE ( 'NONE', *, *, #18627, .F. ) ;
#15056 = CARTESIAN_POINT ( 'NONE',  ( -0.4872815388214248311, -32.17263893204430047, 7.769368695748482878 ) ) ;
#15057 = CARTESIAN_POINT ( 'NONE',  ( -79.81323911311395136, -6.649679829688860622, -4.608218461864638904 ) ) ;
#15058 = CARTESIAN_POINT ( 'NONE',  ( 21.29228973259959901, 5.334523051338725175, 3.529574787382050882 ) ) ;
#15059 = B_SPLINE_SURFACE_WITH_KNOTS ( 'NONE', 3, 3, ( 
 ( #3034, #40249, #28106, #40661 ),
 ( #23988, #11623, #2197, #33694 ),
 ( #6091, #18624, #31213, #37168 ),
 ( #24410, #17807, #15552, #36967 ),
 ( #5473, #27289, #36558, #30392 ),
 ( #39854, #2413, #31013, #20912 ),
 ( #34117, #36761, #8547, #15342 ),
 ( #18016, #30813, #21127, #2818 ),
 ( #30604, #40443, #14934, #27898 ),
 ( #40053, #11827, #27693, #8746 ),
 ( #21331, #8954, #33905, #5679 ),
 ( #12252, #2618, #24824, #12035 ),
 ( #7102, #38180, #22365, #37980 ),
 ( #3639, #16359, #31825, #16164 ),
 ( #19665, #28728, #19256, #540 ),
 ( #3842, #6708, #18845, #6905 ),
 ( #25638, #13076, #22562, #10178 ),
 ( #15759, #32239, #9983, #35127 ),
 ( #12663, #19461, #19056, #25238 ),
 ( #4039, #32035, #28933, #34519 ),
 ( #16555, #28314, #25842, #35333 ),
 ( #734, #37769, #12871, #21947 ),
 ( #25435, #31415, #34728, #3242 ),
 ( #6296, #13271, #132, #31619 ),
 ( #12463, #6508, #38376, #9576 ) ),
 .UNSPECIFIED., .F., .F., .F.,
 ( 4, 3, 3, 3, 3, 3, 3, 3, 4 ),
 ( 4, 4 ),
 ( 0.003645227204780212768, 0.004012130669716890488, 0.004379034134653567341, 0.005112841064526921914, 0.006580454924273630192, 0.008048068784020338470, 0.009515682643767047616, 0.01245091036326046417, 0.01538613808275388073 ),
 ( 0.000000000000000000, 1.006050268738574616 ),
 .UNSPECIFIED. ) ;
#15060 = DIRECTION ( 'NONE',  ( 0.000000000000000000, 0.000000000000000000, 1.000000000000000000 ) ) ;
#15061 = CARTESIAN_POINT ( 'NONE',  ( 4.626733377823518012, -27.83888570657239470, 7.695279973900954751 ) ) ;
#15062 = EDGE_LOOP ( 'NONE', ( #11973, #30357, #27354, #25981, #5346, #38055, #29026, #18038, #15886, #27128, #18887, #2957 ) ) ;
#15063 = CARTESIAN_POINT ( 'NONE',  ( 24.34017676013632325, 3.136949483460702570, 3.398357025751408855 ) ) ;
#15064 = CARTESIAN_POINT ( 'NONE',  ( 81.04763707098177861, 66.10603528134693363, -1.000000000000000000 ) ) ;
#15065 = CARTESIAN_POINT ( 'NONE',  ( 79.66028364141931206, 64.99138685963063722, 3.354617312347331293 ) ) ;
#15066 = B_SPLINE_CURVE_WITH_KNOTS ( 'NONE', 3,
 ( #28874, #3980, #19999, #13018, #7041, #10524, #13221, #680, #4376, #38728, #19609, #7243, #38321, #16899, #22708, #29671, #29480, #13624, #25787, #26397, #883, #7647, #10118, #16691, #35670 ),
 .UNSPECIFIED., .F., .F.,
 ( 4, 3, 3, 3, 3, 3, 3, 3, 4 ),
 ( 6.468151674593620168E-05, 9.076621574722086106E-05, 0.0001210204262067974786, 0.0001512763324577443783, 0.0001815301820994217827, 0.0002117781465860715459, 0.0002420274594459759666, 0.0002722905548971157885, 0.0002816827545175587338 ),
 .UNSPECIFIED. ) ;
#15068 = EDGE_CURVE ( 'NONE', #273, #1547, #3541, .T. ) ;
#15067 = CARTESIAN_POINT ( 'NONE',  ( 2.338742698598150316, -26.23039339646865287, 6.894806418505346812 ) ) ;
#15069 = ORIENTED_EDGE ( 'NONE', *, *, #15999, .T. ) ;
#15070 = CARTESIAN_POINT ( 'NONE',  ( 75.95345872531814280, 63.43160129075363329, -3.385286751594662746 ) ) ;
#15072 = CARTESIAN_POINT ( 'NONE',  ( 14.75748024341934439, -4.578899578309257201, -2.509460294425407412 ) ) ;
#15071 = CARTESIAN_POINT ( 'NONE',  ( 26.06250554953703613, 0.7788941295968891954, 4.421378155111866270 ) ) ;
#15073 = CARTESIAN_POINT ( 'NONE',  ( 78.97265649164266677, 66.09949689503568493, -1.726519205788536571 ) ) ;
#15074 = CARTESIAN_POINT ( 'NONE',  ( 79.44050761702634134, 61.30339496468049987, 3.042889847487580290 ) ) ;
#15075 = ORIENTED_EDGE ( 'NONE', *, *, #10172, .F. ) ;
#15076 = CARTESIAN_POINT ( 'NONE',  ( 1.700390093233090871, -29.56993018339339940, 7.800000000000000711 ) ) ;
#15077 = CARTESIAN_POINT ( 'NONE',  ( 78.98807859296744027, 66.20728402696082071, 1.114595100209202494 ) ) ;
#15079 = CARTESIAN_POINT ( 'NONE',  ( -1.696497448580634781, -29.42448250114750863, 6.868387053540520704 ) ) ;
#15078 = CARTESIAN_POINT ( 'NONE',  ( -7.890026461918812295, -8.913725925455491250, -6.000000000000000000 ) ) ;
#15080 = CARTESIAN_POINT ( 'NONE',  ( 29.21535032918476915, 2.216127810226045547, -1.021449648108430086 ) ) ;
#15081 = CARTESIAN_POINT ( 'NONE',  ( 14.74047039395649605, -5.121629765571634074, -2.499999999999999556 ) ) ;
#15082 = DIRECTION ( 'NONE',  ( -0.000000000000000000, -0.000000000000000000, 1.000000000000000000 ) ) ;
#15083 = CARTESIAN_POINT ( 'NONE',  ( -62.83712641625182016, 35.61106514070144868, 5.789832448495932482 ) ) ;
#15084 = CARTESIAN_POINT ( 'NONE',  ( 24.72931927919737660, 0.6236087402561421023, -4.781898317253668651 ) ) ;
#15085 = AXIS2_PLACEMENT_3D ( 'NONE', #16696, #3586, #6855 ) ;
#15086 = CARTESIAN_POINT ( 'NONE',  ( -34.44874870218064444, -25.49307895267003587, 6.800000000000000711 ) ) ;
#15087 = PLANE ( 'NONE',  #9243 ) ;
#15088 = CARTESIAN_POINT ( 'NONE',  ( -71.72837670882105954, -34.30579396504363388, -1.385640646055078307 ) ) ;
#15089 = CARTESIAN_POINT ( 'NONE',  ( -4.348748702180639469, -25.49307895267003587, 6.700000000000000178 ) ) ;
#15090 = CARTESIAN_POINT ( 'NONE',  ( 36.39222352889621703, -1.827525151019651517, -5.788514553718531630 ) ) ;
#15091 = DIRECTION ( 'NONE',  ( -0.8660254037844399289, 0.000000000000000000, -0.4999999999999977240 ) ) ;
#15092 = CARTESIAN_POINT ( 'NONE',  ( -70.92837670882107659, -23.80776546975053520, 10.00000000000000533 ) ) ;
#15093 = CARTESIAN_POINT ( 'NONE',  ( -21.07867591359219617, -24.55319635012989110, 6.700000000000000178 ) ) ;
#15094 = CARTESIAN_POINT ( 'NONE',  ( -0.02684669743237798334, -25.18051837188491149, 7.754798119455333705 ) ) ;
#15095 = DIRECTION ( 'NONE',  ( -1.000000000000000000, -1.038556294491206740E-15, 0.000000000000000000 ) ) ;
#15096 = CARTESIAN_POINT ( 'NONE',  ( 4.627023651880590727, -27.83937644663651412, 7.680992449362121555 ) ) ;
#15097 = EDGE_CURVE ( 'NONE', #25288, #18231, #36718, .T. ) ;
#15098 = CARTESIAN_POINT ( 'NONE',  ( -64.08758708074093136, 36.43951107222060415, -3.602717568033520834 ) ) ;
#15099 = CARTESIAN_POINT ( 'NONE',  ( 14.73622163650396999, -5.027757633256064729, -2.500471392631596235 ) ) ;
#15100 = CARTESIAN_POINT ( 'NONE',  ( 23.91523202801653269, 2.089873375604069494, -4.428822888773534139 ) ) ;
#15101 = VECTOR ( 'NONE', #7036, 1000.000000000000000 ) ;
#15102 = CARTESIAN_POINT ( 'NONE',  ( -1.519035479433219038, -30.66327089748390122, 6.874555630061440326 ) ) ;
#15103 = EDGE_CURVE ( 'NONE', #34769, #18315, #16962, .T. ) ;
#15104 = CARTESIAN_POINT ( 'NONE',  ( 70.53871541878200446, 60.47550293342311534, -3.775670717450619218 ) ) ;
#15105 = B_SPLINE_CURVE_WITH_KNOTS ( 'NONE', 3,
 ( #13845, #10738, #23318, #1501, #14034, #39146, #39348, #34027, #36475, #2317 ),
 .UNSPECIFIED., .F., .F.,
 ( 4, 3, 3, 4 ),
 ( 0.0002170292169044778436, 0.0002420761345915944658, 0.0002723302478206986307, 0.0002816811360866790779 ),
 .UNSPECIFIED. ) ;
#15106 = ADVANCED_FACE ( 'NONE', ( #7704 ), #20254, .F. ) ;
#15107 = ORIENTED_EDGE ( 'NONE', *, *, #30928, .T. ) ;
#15108 = DIRECTION ( 'NONE',  ( 1.000000000000000000, 0.000000000000000000, 0.000000000000000000 ) ) ;
#15109 = CARTESIAN_POINT ( 'NONE',  ( -0.8786759135921904385, -24.55319635012989110, 6.700000000000000178 ) ) ;
#15110 = CARTESIAN_POINT ( 'NONE',  ( 70.06771224146353916, 58.30163689823704942, 3.863726395435713723 ) ) ;
#15111 = CARTESIAN_POINT ( 'NONE',  ( 5.002097081266497547, -28.40856126717273611, 6.887161170156906209 ) ) ;
#15112 = CARTESIAN_POINT ( 'NONE',  ( -1.416461651392222354, -28.21153572011717614, 6.949473656533217358 ) ) ;
#15113 = CARTESIAN_POINT ( 'NONE',  ( 4.852421344848616869, -30.84456871255493482, 7.757178535559533294 ) ) ;
#15114 = CARTESIAN_POINT ( 'NONE',  ( -1.331572764389289398, -28.01586578234813985, 7.139196562012272373 ) ) ;
#15115 = ORIENTED_EDGE ( 'NONE', *, *, #23481, .T. ) ;
#15116 = CARTESIAN_POINT ( 'NONE',  ( 24.41296328559054984, 3.167430643262210133, 3.253911296061570368 ) ) ;
#15117 = AXIS2_PLACEMENT_3D ( 'NONE', #5818, #27629, #29754 ) ;
#15118 = FACE_OUTER_BOUND ( 'NONE', #35639, .T. ) ;
#15119 = EDGE_CURVE ( 'NONE', #6204, #14209, #36124, .T. ) ;
#15120 = EDGE_LOOP ( 'NONE', ( #38607, #10928, #18870, #14697 ) ) ;
#15121 = CARTESIAN_POINT ( 'NONE',  ( 78.43571320973860850, 65.80086540191352640, -1.884339924308604086 ) ) ;
#15122 = CARTESIAN_POINT ( 'NONE',  ( 15.78341776548205111, 8.012724091073605948, -3.484800346807145566 ) ) ;
#15123 = CARTESIAN_POINT ( 'NONE',  ( 81.56442676284295601, 64.14391357695993179, -3.071899782094856590 ) ) ;
#15124 = CARTESIAN_POINT ( 'NONE',  ( 80.72570547868225788, 61.86964107431865045, 2.884918531047036439 ) ) ;
#15125 = ORIENTED_EDGE ( 'NONE', *, *, #35181, .T. ) ;
#15126 = PLANE ( 'NONE',  #8971 ) ;
#15127 = VECTOR ( 'NONE', #28500, 1000.000000000000000 ) ;
#15128 = CARTESIAN_POINT ( 'NONE',  ( 21.85643539959775339, -5.954433958055524556, -11.26730592371362505 ) ) ;
#15129 = ORIENTED_EDGE ( 'NONE', *, *, #13258, .F. ) ;
#15130 = CARTESIAN_POINT ( 'NONE',  ( -80.85577149014498843, 10.55954795747387820, 1.459777158011418496 ) ) ;
#15131 = CARTESIAN_POINT ( 'NONE',  ( 5.916497905674401814, -30.25835747790444330, 7.695279973900954751 ) ) ;
#15132 = CARTESIAN_POINT ( 'NONE',  ( 3.037211893591657219, -26.44376520468768632, 7.013842709614101167 ) ) ;
#15133 = CARTESIAN_POINT ( 'NONE',  ( 1.580679853655120093, -32.96782274345532926, 7.757178535559534183 ) ) ;
#15134 = CARTESIAN_POINT ( 'NONE',  ( 28.22828621824402973, -3.406067573266987392, -4.612104786675601531 ) ) ;
#15135 = CARTESIAN_POINT ( 'NONE',  ( 27.81756494040502048, 1.846260971994820199, -3.902053172858347185 ) ) ;
#15136 = CARTESIAN_POINT ( 'NONE',  ( 3.723260060725158471, -32.30269659105433533, 6.979335674598008410 ) ) ;
#15137 = PLANE ( 'NONE',  #6979 ) ;
#15138 = CARTESIAN_POINT ( 'NONE',  ( 4.321330788254073241, -31.73572891817300601, 7.652160403243379427 ) ) ;
#15139 = CARTESIAN_POINT ( 'NONE',  ( 5.042542681852490993, -28.94541254208796133, 7.712764235869103757 ) ) ;
#15140 = AXIS2_PLACEMENT_3D ( 'NONE', #40447, #8752, #21546 ) ;
#15141 = B_SPLINE_CURVE_WITH_KNOTS ( 'NONE', 3,
 ( #20112, #17011, #29587, #16419, #35391, #13324, #1002, #10638, #7758, #7161, #14128, #32487, #22621, #23019, #32691, #4678 ),
 .UNSPECIFIED., .F., .F.,
 ( 4, 2, 2, 2, 2, 2, 2, 4 ),
 ( 0.000000000000000000, 0.0004519050042106062602, 0.0009038100084212125204, 0.001355715012631818726, 0.001807620016842425041, 0.002259525021053031355, 0.002711430025263637453, 0.003615240033684850082 ),
 .UNSPECIFIED. ) ;
#15142 = CARTESIAN_POINT ( 'NONE',  ( 3.913215462449400217, -32.15128716865380909, 7.691066658568949777 ) ) ;
#15143 = CARTESIAN_POINT ( 'NONE',  ( 37.13687059807102031, -2.464987586452376256, -5.964471309820316591 ) ) ;
#15144 = CARTESIAN_POINT ( 'NONE',  ( 26.61436230569603723, 1.627489583404493345, -4.333517427382849618 ) ) ;
#15145 = ORIENTED_EDGE ( 'NONE', *, *, #18630, .T. ) ;
#15147 = EDGE_CURVE ( 'NONE', #3289, #30686, #9404, .T. ) ;
#15146 = CARTESIAN_POINT ( 'NONE',  ( 67.21358634547439692, 57.88870193986200974, 3.993497817183392584 ) ) ;
#15148 = CARTESIAN_POINT ( 'NONE',  ( 32.84220568043447486, -0.7495606313452212177, 5.332218506814426995 ) ) ;
#15149 = CARTESIAN_POINT ( 'NONE',  ( 4.995237956833183723, -30.75059844998224179, 7.750000000000001776 ) ) ;
#15150 = ADVANCED_FACE ( 'NONE', ( #39388 ), #30770, .T. ) ;
#15151 = LINE ( 'NONE', #31431, #29960 ) ;
#15152 = PRODUCT_DEFINITION ( 'UNKNOWN', '', #28109, #36584 ) ;
#15153 = CARTESIAN_POINT ( 'NONE',  ( 88.90249899953845159, -1.697492344831515121, -0.8687328377452782080 ) ) ;
#15154 = AXIS2_PLACEMENT_3D ( 'NONE', #30501, #27196, #23702 ) ;
#15156 = CARTESIAN_POINT ( 'NONE',  ( 35.95119605051105083, -2.121419093699826952, -5.817451645281153993 ) ) ;
#15155 = CARTESIAN_POINT ( 'NONE',  ( 29.20166386951125048, 2.268204792580242213, 0.006282727923920283265 ) ) ;
#15157 = ORIENTED_EDGE ( 'NONE', *, *, #21243, .T. ) ;
#15158 = CARTESIAN_POINT ( 'NONE',  ( -1.610418084489225299, -28.79627056164295595, 7.013842709614101167 ) ) ;
#15159 = CARTESIAN_POINT ( 'NONE',  ( -0.6931531239536370403, -32.12354543778459970, 6.951256099901587326 ) ) ;
#15160 = ORIENTED_EDGE ( 'NONE', *, *, #1148, .F. ) ;
#15161 = CARTESIAN_POINT ( 'NONE',  ( -71.15343164110390717, -21.75733751372833069, 3.995777704139396036 ) ) ;
#15162 = ORIENTED_EDGE ( 'NONE', *, *, #34569, .T. ) ;
#15163 = CARTESIAN_POINT ( 'NONE',  ( 80.57935153413077956, 62.61414007970553541, -3.419027627190931451 ) ) ;
#15164 = CARTESIAN_POINT ( 'NONE',  ( -1.571041143654955619, -28.32584913204942012, 6.878641987404677138 ) ) ;
#15165 = CARTESIAN_POINT ( 'NONE',  ( 78.66262733798791373, 65.98865143197195948, 1.634613895560430796 ) ) ;
#15167 = ORIENTED_EDGE ( 'NONE', *, *, #35067, .T. ) ;
#15166 = DIRECTION ( 'NONE',  ( 0.6834397476448829112, 0.000000000000000000, -0.7300069255418737413 ) ) ;
#15168 = AXIS2_PLACEMENT_3D ( 'NONE', #23162, #1962, #10983 ) ;
#15169 = CARTESIAN_POINT ( 'NONE',  ( 74.80267162900737787, 60.00335986791986898, -3.708893976703238948 ) ) ;
#15170 = CARTESIAN_POINT ( 'NONE',  ( 3.281726478462255958, -32.57982635458228060, 6.865312560952604670 ) ) ;
#15171 = B_SPLINE_CURVE_WITH_KNOTS ( 'NONE', 3,
 ( #26166, #11090, #1262, #10892, #10296, #38698 ),
 .UNSPECIFIED., .F., .F.,
 ( 4, 2, 4 ),
 ( 0.000000000000000000, 0.0008616653180068700344, 0.001723330636013740069 ),
 .UNSPECIFIED. ) ;
#15173 = DIRECTION ( 'NONE',  ( -0.000000000000000000, -0.000000000000000000, -1.000000000000000000 ) ) ;
#15172 = CARTESIAN_POINT ( 'NONE',  ( 4.963238934339704755, -30.83638965544459154, 6.867280401193710304 ) ) ;
#15174 = CARTESIAN_POINT ( 'NONE',  ( 3.436873281388448831, -26.53107670108079219, 7.638132480492518361 ) ) ;
#15175 = DIRECTION ( 'NONE',  ( -1.000000000000000000, -0.000000000000000000, -0.000000000000000000 ) ) ;
#15176 = CARTESIAN_POINT ( 'NONE',  ( 23.72115022044104293, 3.525691739180937923, -3.279221235023926262 ) ) ;
#15177 = ORIENTED_EDGE ( 'NONE', *, *, #19034, .F. ) ;
#15178 = CARTESIAN_POINT ( 'NONE',  ( 4.107940300203791750, -27.02011124655863838, 7.387053503561884504 ) ) ;
#15179 = ADVANCED_FACE ( 'NONE', ( #6249 ), #25186, .T. ) ;
#15180 = CARTESIAN_POINT ( 'NONE',  ( 26.75871784592184710, 2.055338430770167424, -4.125980934060708982 ) ) ;
#15181 = CARTESIAN_POINT ( 'NONE',  ( -70.92837670882107659, 15.04836564048558500, 0.000000000000000000 ) ) ;
#15182 = DIRECTION ( 'NONE',  ( -0.7376613619250370624, -0.6751708784618154491, 0.000000000000000000 ) ) ;
#15183 = CARTESIAN_POINT ( 'NONE',  ( 80.79744990009734806, 64.13345242326639095, 3.486376426170536558 ) ) ;
#15184 = CARTESIAN_POINT ( 'NONE',  ( 88.16134551068515179, -2.448791080374484341, 0.2153404935567143075 ) ) ;
#15185 = CARTESIAN_POINT ( 'NONE',  ( 14.77315594796471743, 13.19392823276620419, 2.499999999999996891 ) ) ;
#15186 = ORIENTED_EDGE ( 'NONE', *, *, #14588, .F. ) ;
#15187 = DIRECTION ( 'NONE',  ( -1.000000000000000000, 6.367278819747327815E-17, -0.000000000000000000 ) ) ;
#15188 = CARTESIAN_POINT ( 'NONE',  ( 3.507358713047826093, -26.68983062858202970, 6.863904403958575706 ) ) ;
#15189 = ADVANCED_FACE ( 'NONE', ( #9320 ), #33655, .F. ) ;
#15190 = FACE_OUTER_BOUND ( 'NONE', #28554, .T. ) ;
#15191 = EDGE_CURVE ( 'NONE', #25957, #7083, #18582, .T. ) ;
#15192 = CARTESIAN_POINT ( 'NONE',  ( 33.95701888394219736, -3.573114794754973733, -5.438351141695983770 ) ) ;
#15193 = CARTESIAN_POINT ( 'NONE',  ( 32.77851786469086903, -0.9351265186074488867, -5.322278482871990235 ) ) ;
#15194 = CARTESIAN_POINT ( 'NONE',  ( -23.07867591359219617, -26.64985754041175525, 6.700000000000000178 ) ) ;
#15195 = B_SPLINE_CURVE_WITH_KNOTS ( 'NONE', 3,
 ( #3090, #22005, #25088, #37617, #9416, #6356, #15817 ),
 .UNSPECIFIED., .F., .F.,
 ( 4, 3, 4 ),
 ( 0.006764200096651864190, 0.007395461704374725088, 0.007885996417619594440 ),
 .UNSPECIFIED. ) ;
#15196 = DIRECTION ( 'NONE',  ( 1.000000000000000000, 0.000000000000000000, 0.000000000000000000 ) ) ;
#15197 = ORIENTED_EDGE ( 'NONE', *, *, #14679, .T. ) ;
#15198 = CARTESIAN_POINT ( 'NONE',  ( 22.91836776944852261, 2.645787328278193851, 3.783363591877844101 ) ) ;
#15199 = VECTOR ( 'NONE', #29242, 1000.000000000000114 ) ;
#15200 = ADVANCED_FACE ( 'NONE', ( #31170 ), #34475, .F. ) ;
#15201 = EDGE_CURVE ( 'NONE', #19164, #36530, #36927, .T. ) ;
#15202 = CARTESIAN_POINT ( 'NONE',  ( 87.04213330793400871, 0.5878691963681530464, -4.891134986362597914 ) ) ;
#15203 = ORIENTED_EDGE ( 'NONE', *, *, #21675, .T. ) ;
#15204 = ORIENTED_EDGE ( 'NONE', *, *, #27658, .F. ) ;
#15206 = CARTESIAN_POINT ( 'NONE',  ( 36.68582491073361496, -1.914190917646145129, 5.802815688716031595 ) ) ;
#15205 = CARTESIAN_POINT ( 'NONE',  ( 78.77361741396553896, 66.07891176884447759, -1.467306180864093701 ) ) ;
#15207 = CARTESIAN_POINT ( 'NONE',  ( 15.79641112846907625, -3.685450897386115532, -2.654044247040655335 ) ) ;
#15208 = CARTESIAN_POINT ( 'NONE',  ( 14.71640407929426964, 12.89631605134570691, -2.500000000000019096 ) ) ;
#15209 = EDGE_LOOP ( 'NONE', ( #13914, #39900, #27569 ) ) ;
#15210 = DIRECTION ( 'NONE',  ( 0.000000000000000000, 0.000000000000000000, 1.000000000000000000 ) ) ;
#15211 = VERTEX_POINT ( 'NONE', #34280 ) ;
#15212 = AXIS2_PLACEMENT_3D ( 'NONE', #4559, #26183, #10313 ) ;
#15213 = ORIENTED_EDGE ( 'NONE', *, *, #37455, .F. ) ;
#15214 = CARTESIAN_POINT ( 'NONE',  ( 79.87286157980665280, 64.75688458792352264, -3.459421039841298562 ) ) ;
#15215 = CARTESIAN_POINT ( 'NONE',  ( -58.97877168559173811, 27.59157091290065367, -6.753965997777704899 ) ) ;
#15216 = ORIENTED_EDGE ( 'NONE', *, *, #40287, .F. ) ;
#15218 = CARTESIAN_POINT ( 'NONE',  ( 21.52272803504227383, 7.572183114303116191, -2.831506016415840321 ) ) ;
#15217 = CARTESIAN_POINT ( 'NONE',  ( 24.34875050026406029, 2.411635393770941604, 4.109526650664126812 ) ) ;
#15219 = ORIENTED_EDGE ( 'NONE', *, *, #29796, .F. ) ;
#15220 = CARTESIAN_POINT ( 'NONE',  ( 81.38476203741939230, 61.42515712988156906, -1.285939662725171351 ) ) ;
#15221 = LINE ( 'NONE', #24698, #7106 ) ;
#15222 = LINE ( 'NONE', #30066, #15374 ) ;
#15223 = ORIENTED_EDGE ( 'NONE', *, *, #13587, .T. ) ;
#15225 = CARTESIAN_POINT ( 'NONE',  ( 0.5197218266442334977, -32.86477804699348582, 7.750000000000000888 ) ) ;
#15224 = CARTESIAN_POINT ( 'NONE',  ( -1.740011302788441183, -30.21307731605675073, 7.695279973900954751 ) ) ;
#15226 = DIRECTION ( 'NONE',  ( 1.000000000000000000, -5.253733955815473636E-14, 0.000000000000000000 ) ) ;
#15227 = CARTESIAN_POINT ( 'NONE',  ( 5.200390093233090205, -29.56993018339339940, 6.929570838012950595 ) ) ;
#15228 = CARTESIAN_POINT ( 'NONE',  ( 73.22742653720867168, 60.47695785811286839, 3.944160774617319287 ) ) ;
#15229 = CARTESIAN_POINT ( 'NONE',  ( 23.97548348472609092, 2.871991460080824066, -3.880200249615740393 ) ) ;
#15230 = ORIENTED_EDGE ( 'NONE', *, *, #20088, .F. ) ;
#15231 = LINE ( 'NONE', #27785, #25069 ) ;
#15232 = B_SPLINE_CURVE_WITH_KNOTS ( 'NONE', 3,
 ( #27392, #34421, #40154, #24719, #5990, #36868, #18739, #18527, #5577, #37268 ),
 .UNSPECIFIED., .F., .F.,
 ( 4, 3, 3, 4 ),
 ( 0.0002170292169044763799, 0.0002420761345915966613, 0.0002723302478207007449, 0.0002816811360866726269 ),
 .UNSPECIFIED. ) ;
#15233 = CARTESIAN_POINT ( 'NONE',  ( 21.85643539959775694, 4.302923821179891029, -14.48878861646959315 ) ) ;
#15234 = CARTESIAN_POINT ( 'NONE',  ( -58.11958539874534324, 31.63166798347506159, -4.423482167568619339 ) ) ;
#15235 = ORIENTED_EDGE ( 'NONE', *, *, #22628, .F. ) ;
#15236 = CARTESIAN_POINT ( 'NONE',  ( 81.04721337197119624, 65.04274187704046994, 3.019849704268902535 ) ) ;
#15237 = CARTESIAN_POINT ( 'NONE',  ( 88.66415851257785619, -1.234066499448195131, -0.8261491842984883816 ) ) ;
#15238 = CARTESIAN_POINT ( 'NONE',  ( 29.28314298262022319, 1.964681093867868933, 2.525543949525632659 ) ) ;
#15239 = FACE_OUTER_BOUND ( 'NONE', #2047, .T. ) ;
#15240 = CARTESIAN_POINT ( 'NONE',  ( 31.36171663430588197, -3.287353811999296660, 5.090714763224706729 ) ) ;
#15241 = CARTESIAN_POINT ( 'NONE',  ( -89.00859394718983708, 2.429809908903242555, -12.50000000000000000 ) ) ;
#15242 = AXIS2_PLACEMENT_3D ( 'NONE', #8782, #30012, #36394 ) ;
#15243 = CARTESIAN_POINT ( 'NONE',  ( 36.44757542402881256, -2.353335513535177448, -5.894923651499230921 ) ) ;
#15244 = CARTESIAN_POINT ( 'NONE',  ( 5.144146178010085890, -28.94499496390147186, 7.750000000000002665 ) ) ;
#15245 = CARTESIAN_POINT ( 'NONE',  ( 5.185743982427674759, -29.61328051818922802, 7.785096263473210598 ) ) ;
#15246 = FACE_OUTER_BOUND ( 'NONE', #30256, .T. ) ;
#15247 = EDGE_CURVE ( 'NONE', #8430, #40124, #9124, .T. ) ;
#15248 = CARTESIAN_POINT ( 'NONE',  ( 21.85643539959777115, -33.54387950140291963, 2.500000000000000000 ) ) ;
#15249 = EDGE_CURVE ( 'NONE', #9234, #12066, #2776, .T. ) ;
#15250 = DIRECTION ( 'NONE',  ( 0.8660254037844399289, 0.000000000000000000, 0.4999999999999976685 ) ) ;
#15251 = EDGE_CURVE ( 'NONE', #26757, #446, #2201, .T. ) ;
#15252 = ORIENTED_EDGE ( 'NONE', *, *, #37599, .F. ) ;
#15253 = CARTESIAN_POINT ( 'NONE',  ( 33.67928082117678201, -3.778927839680616518, 5.203631254605035394 ) ) ;
#15254 =( BOUNDED_SURFACE ( )  B_SPLINE_SURFACE ( 3, 2, ( 
 ( #23008, #37818, #34978 ),
 ( #31465, #31669, #3485 ),
 ( #6753, #3685, #16209 ),
 ( #13126, #25685, #7344 ) ),
 .UNSPECIFIED., .F., .F., .T. ) 
 B_SPLINE_SURFACE_WITH_KNOTS ( ( 4, 4 ),
 ( 3, 3 ),
 ( 0.005270629645086826603, 0.007540928297313504239 ),
 ( 0.000000000000000000, 1.000000000000000000 ),
 .UNSPECIFIED. ) 
 GEOMETRIC_REPRESENTATION_ITEM ( )  RATIONAL_B_SPLINE_SURFACE ( (
 ( 1.000000000000000000, 0.8929511290151087577, 1.000000000000000000),
 ( 1.000000000000000000, 0.8751608305411335831, 1.000000000000000000),
 ( 1.000000000000000000, 0.8609515519834827213, 1.000000000000000000),
 ( 1.000000000000000000, 0.8503725744608083836, 1.000000000000000000) ) ) 
 REPRESENTATION_ITEM ( '' )  SURFACE ( )  );
#15255 = CARTESIAN_POINT ( 'NONE',  ( -71.45635794260526552, 0.07346082103169225552, 5.989611775372480018 ) ) ;
#15256 = CARTESIAN_POINT ( 'NONE',  ( 66.82203765260634043, 58.05418649187924274, -3.997265020314329842 ) ) ;
#15257 = CARTESIAN_POINT ( 'NONE',  ( -71.43139732235886186, 0.09104805635102961037, 9.988066921647986263 ) ) ;
#15258 = CARTESIAN_POINT ( 'NONE',  ( -59.00782325774518000, 28.07066389825142139, -6.403654028263551012 ) ) ;
#15259 = ORIENTED_EDGE ( 'NONE', *, *, #7679, .F. ) ;
#15260 = LINE ( 'NONE', #34235, #32469 ) ;
#15261 = CARTESIAN_POINT ( 'NONE',  ( -1.594457770366995319, -28.38926191680453925, 7.750000000000000888 ) ) ;
#15262 = PLANE ( 'NONE',  #35199 ) ;
#15263 = ORIENTED_EDGE ( 'NONE', *, *, #17360, .T. ) ;
#15264 = LINE ( 'NONE', #14640, #414 ) ;
#15265 = DIRECTION ( 'NONE',  ( 0.000000000000000000, 0.000000000000000000, 1.000000000000000000 ) ) ;
#15266 = ORIENTED_EDGE ( 'NONE', *, *, #19381, .F. ) ;
#15267 = CARTESIAN_POINT ( 'NONE',  ( 24.35304765632307067, 3.141127394751760615, 3.377496490332608126 ) ) ;
#15268 = CARTESIAN_POINT ( 'NONE',  ( 82.10909544300281482, 65.20937546977818045, -1.000000000000000000 ) ) ;
#15269 = CARTESIAN_POINT ( 'NONE',  ( 78.62614802285547455, 66.01297166972811681, 1.268354304253248577 ) ) ;
#15270 = CARTESIAN_POINT ( 'NONE',  ( -0.1724601174513000490, -32.40761094210100879, 6.988553391373221402 ) ) ;
#15271 = ORIENTED_EDGE ( 'NONE', *, *, #3950, .T. ) ;
#15272 = CARTESIAN_POINT ( 'NONE',  ( 76.81217388538108537, 61.66049381551730590, -3.848392762315877569 ) ) ;
#15273 = B_SPLINE_CURVE_WITH_KNOTS ( 'NONE', 3,
 ( #25947, #32537, #7402, #16262, #28834, #22667, #38481, #10081, #35828, #7202 ),
 .UNSPECIFIED., .F., .F.,
 ( 4, 3, 3, 4 ),
 ( 1.022834283856302764E-18, 3.025570593003244134E-05, 6.051145698344170592E-05, 6.468151674593708260E-05 ),
 .UNSPECIFIED. ) ;
#15275 = DIRECTION ( 'NONE',  ( -0.000000000000000000, -0.000000000000000000, -1.000000000000000000 ) ) ;
#15274 = CARTESIAN_POINT ( 'NONE',  ( 3.888958500451919154, -32.28338504940279563, 7.784725160561908552 ) ) ;
#15276 = CARTESIAN_POINT ( 'NONE',  ( -55.16612787639762416, 31.23053227951969646, -1.484562114140327793 ) ) ;
#15277 = CARTESIAN_POINT ( 'NONE',  ( 81.29167079631734794, 61.38276384236289829, -1.400336002810706360 ) ) ;
#15278 = CARTESIAN_POINT ( 'NONE',  ( 78.86847112531712867, 61.76850681771009732, 3.535928464255590598 ) ) ;
#15279 = ORIENTED_EDGE ( 'NONE', *, *, #19262, .F. ) ;
#15280 = AXIS2_PLACEMENT_3D ( 'NONE', #10136, #13642, #19422 ) ;
#15281 = EDGE_LOOP ( 'NONE', ( #28338, #455, #37677, #32175 ) ) ;
#15282 = CARTESIAN_POINT ( 'NONE',  ( 1.651639975615219580, -32.96958066925694908, 6.894806418505345036 ) ) ;
#15283 = ORIENTED_EDGE ( 'NONE', *, *, #32006, .T. ) ;
#15284 = CARTESIAN_POINT ( 'NONE',  ( 81.71086237227946469, 61.67650090218641168, 1.250621450094001830 ) ) ;
#15286 = CARTESIAN_POINT ( 'NONE',  ( -1.693125452676301768, -29.36004392926684758, 6.959317978105164393 ) ) ;
#15285 = CARTESIAN_POINT ( 'NONE',  ( -64.08758708074091714, 42.49506848047520435, 2.672779995105290407 ) ) ;
#15287 = CARTESIAN_POINT ( 'NONE',  ( 31.36201648005763332, -1.233860125724708379, -5.969386505766030915 ) ) ;
#15288 = CARTESIAN_POINT ( 'NONE',  ( -1.417651227037130868, -31.15984618490730540, 6.912143950357346966 ) ) ;
#15289 = CARTESIAN_POINT ( 'NONE',  ( -64.08758708074093136, -65.19654454972992141, -8.800414904976381791 ) ) ;
#15290 = CARTESIAN_POINT ( 'NONE',  ( 1.509278095782431217, -33.06470984435662075, 6.971170733404103537 ) ) ;
#15291 = CARTESIAN_POINT ( 'NONE',  ( 21.73499591390137908, 0.2555434075777953118, -9.002945845404971337 ) ) ;
#15292 = FACE_OUTER_BOUND ( 'NONE', #34953, .T. ) ;
#15293 = ORIENTED_EDGE ( 'NONE', *, *, #19677, .T. ) ;
#15294 = DIRECTION ( 'NONE',  ( 0.000000000000000000, 0.000000000000000000, 1.000000000000000000 ) ) ;
#15295 = DIRECTION ( 'NONE',  ( -1.000000000000000000, 0.000000000000000000, 0.000000000000000000 ) ) ;
#15296 = CARTESIAN_POINT ( 'NONE',  ( 5.198039085808181525, -29.69173459304409946, 7.754798119455333705 ) ) ;
#15297 = CARTESIAN_POINT ( 'NONE',  ( -71.31679049852404262, -48.56916478021601336, 9.992914751153948671 ) ) ;
#15298 = CARTESIAN_POINT ( 'NONE',  ( 25.66381174941535903, 2.554701667279945632, -3.769256280910082246 ) ) ;
#15299 = CYLINDRICAL_SURFACE ( 'NONE', #33197, 0.1000000000000028644 ) ;
#15300 = DIRECTION ( 'NONE',  ( -0.5000000000000039968, 0.8660254037844362651, -0.000000000000000000 ) ) ;
#15301 = DIRECTION ( 'NONE',  ( -0.000000000000000000, -0.000000000000000000, -1.000000000000000000 ) ) ;
#15302 = CARTESIAN_POINT ( 'NONE',  ( -0.8560347025813198618, -25.25037435423009669, 7.695279973900954751 ) ) ;
#15303 = DIRECTION ( 'NONE',  ( 0.000000000000000000, 0.000000000000000000, 1.000000000000000000 ) ) ;
#15304 = VECTOR ( 'NONE', #8323, 1000.000000000000000 ) ;
#15305 = CARTESIAN_POINT ( 'NONE',  ( -3.078675913592197944, -24.55319635012989110, 6.700000000000000178 ) ) ;
#15306 = CARTESIAN_POINT ( 'NONE',  ( 14.75656734209353438, -5.138193647293536337, -2.500021671374450971 ) ) ;
#15307 = CARTESIAN_POINT ( 'NONE',  ( 24.36996980807726487, 1.959928190074600174, -4.382497187266871208 ) ) ;
#15308 = EDGE_CURVE ( 'NONE', #4723, #40343, #12620, .T. ) ;
#15309 = DIRECTION ( 'NONE',  ( -0.000000000000000000, -0.000000000000000000, 1.000000000000000000 ) ) ;
#15310 = ORIENTED_EDGE ( 'NONE', *, *, #25355, .T. ) ;
#15311 = FILL_AREA_STYLE ('',( #2582 ) ) ;
#15312 = CARTESIAN_POINT ( 'NONE',  ( 69.03381461298826594, 59.23726071663833181, -3.954017255840780454 ) ) ;
#15313 = CIRCLE ( 'NONE', #14614, 8.080217238368769372 ) ;
#15314 = ORIENTED_EDGE ( 'NONE', *, *, #11883, .F. ) ;
#15315 = CARTESIAN_POINT ( 'NONE',  ( 86.43572624768424362, -0.5192074800720991590, -5.777013305174518720 ) ) ;
#15316 = CARTESIAN_POINT ( 'NONE',  ( 0.1004213051519422251, -26.56991353724522398, 6.864276522220859711 ) ) ;
#15317 = CARTESIAN_POINT ( 'NONE',  ( 4.901715390235392711, -30.71514472345701563, 7.748216051605120391 ) ) ;
#15318 = B_SPLINE_CURVE_WITH_KNOTS ( 'NONE', 3,
 ( #10736, #11536, #39759, #36275 ),
 .UNSPECIFIED., .F., .F.,
 ( 4, 4 ),
 ( 0.000000000000000000, 6.391136169898659513E-06 ),
 .UNSPECIFIED. ) ;
#15319 = CARTESIAN_POINT ( 'NONE',  ( -1.219418532703906877, -27.82788610016705988, 6.894806418505346812 ) ) ;
#15320 = VERTEX_POINT ( 'NONE', #34071 ) ;
#15321 = CARTESIAN_POINT ( 'NONE',  ( 22.61561539124943820, 4.625252967631755752, 3.040925913900980770 ) ) ;
#15322 = FILL_AREA_STYLE_COLOUR ( '', #33982 ) ;
#15323 = ORIENTED_EDGE ( 'NONE', *, *, #40555, .T. ) ;
#15324 = CARTESIAN_POINT ( 'NONE',  ( 80.68211079047073042, 61.32331416546043812, -2.218931858625937004 ) ) ;
#15325 = CARTESIAN_POINT ( 'NONE',  ( -1.003639145148646827, -27.34771824976135335, 7.700536657684222241 ) ) ;
#15326 = CARTESIAN_POINT ( 'NONE',  ( 81.96106518217325743, 62.90574382782719454, -2.573500632437588642 ) ) ;
#15327 = EDGE_CURVE ( 'NONE', #32730, #25213, #27653, .T. ) ;
#15328 = CARTESIAN_POINT ( 'NONE',  ( 78.53532592461078821, 65.52573200842934398, 2.475680338657054058 ) ) ;
#15329 = FACE_OUTER_BOUND ( 'NONE', #26810, .T. ) ;
#15330 = CARTESIAN_POINT ( 'NONE',  ( -70.92837670882107659, -37.87473357531881391, -6.000000000000002665 ) ) ;
#15331 = CARTESIAN_POINT ( 'NONE',  ( 22.49462040199967916, -0.5704057512449431933, -9.208717712401224276 ) ) ;
#15332 = VERTEX_POINT ( 'NONE', #40614 ) ;
#15333 = CARTESIAN_POINT ( 'NONE',  ( -72.84144643148528075, 2.639073776085810508, 9.875428661471469027 ) ) ;
#15334=STYLED_ITEM('',(#40773),#26090);
#15335 = CARTESIAN_POINT ( 'NONE',  ( 37.13484346446838202, -3.067129328972788560, 5.985434385025355297 ) ) ;
#15336 = EDGE_CURVE ( 'NONE', #3101, #31945, #18179, .T. ) ;
#15337 = CARTESIAN_POINT ( 'NONE',  ( -4.878675913592187108, -24.55319635012989110, 6.700000000000000178 ) ) ;
#15338 = PLANE ( 'NONE',  #15743 ) ;
#15339 = CARTESIAN_POINT ( 'NONE',  ( 3.427802856742246274, -26.52591081038080389, 7.737115613922529000 ) ) ;
#15340 = CARTESIAN_POINT ( 'NONE',  ( 30.88496348195457486, 0.7017159523777027896, -4.487237605170554033 ) ) ;
#15341 = DIRECTION ( 'NONE',  ( 0.000000000000000000, 0.000000000000000000, 1.000000000000000000 ) ) ;
#15342 = CARTESIAN_POINT ( 'NONE',  ( 14.88745559820020503, 12.58383137495263426, 2.513086349116905538 ) ) ;
#15343 = CARTESIAN_POINT ( 'NONE',  ( 0.1825688514504736348, 0.000000000000000000, 0.000000000000000000 ) ) ;
#15344 = CARTESIAN_POINT ( 'NONE',  ( 29.66982562896108533, -3.795200865155387238, 4.436618837228561318 ) ) ;
#15345 = CARTESIAN_POINT ( 'NONE',  ( 5.042305363714541855, -28.94414881188822619, 7.695279973900954751 ) ) ;
#15346 = CIRCLE ( 'NONE', #12708, 2.500000000000002220 ) ;
#15347 = CARTESIAN_POINT ( 'NONE',  ( 17.33042790160538615, 14.30105679307200717, -2.500000000000000000 ) ) ;
#15348 = CARTESIAN_POINT ( 'NONE',  ( 26.47073111379101817, 1.156830035182202288, -4.368930852996396830 ) ) ;
#15349 = CARTESIAN_POINT ( 'NONE',  ( 36.88979637976984804, -2.115963839364304544, -5.872280461611828706 ) ) ;
#15350 = CARTESIAN_POINT ( 'NONE',  ( 24.72423210327035648, 2.636217293557414632, -3.925404993220885430 ) ) ;
#15351 = EDGE_CURVE ( 'NONE', #637, #11496, #3429, .T. ) ;
#15352 = EDGE_LOOP ( 'NONE', ( #21989, #16487, #25528, #39191 ) ) ;
#15353 = CARTESIAN_POINT ( 'NONE',  ( 66.99315907379003932, 58.03889713220680591, 3.999016414675010012 ) ) ;
#15354 = CARTESIAN_POINT ( 'NONE',  ( 34.12043071199392585, -3.462209586952626150, 5.516511185785388349 ) ) ;
#15355 = DIRECTION ( 'NONE',  ( 0.1736481776669404897, -0.9848077530122062440, -0.000000000000000000 ) ) ;
#15356 = CIRCLE ( 'NONE', #16014, 83.68529983683480111 ) ;
#15357 = LINE ( 'NONE', #31837, #31955 ) ;
#15358 = CARTESIAN_POINT ( 'NONE',  ( 87.94592890065770519, -0.6044765299818539717, 4.822713664802365408 ) ) ;
#15359 = CARTESIAN_POINT ( 'NONE',  ( 37.05071641422330231, -2.827661766178285685, -5.989058390038934476 ) ) ;
#15360 = EDGE_LOOP ( 'NONE', ( #22640, #19612, #13116, #8642 ) ) ;
#15361 = CARTESIAN_POINT ( 'NONE',  ( 24.70880527336989374, 2.644804217804675339, 3.921322591264182034 ) ) ;
#15362 = CARTESIAN_POINT ( 'NONE',  ( -74.03402466285147909, 19.33157623370696498, -9.800414904976365804 ) ) ;
#15363 = EDGE_CURVE ( 'NONE', #6556, #8986, #3398, .T. ) ;
#15364 = ORIENTED_EDGE ( 'NONE', *, *, #17140, .T. ) ;
#15365 = CARTESIAN_POINT ( 'NONE',  ( -70.30712919725708332, -21.57437711518543111, 3.968280824155048236 ) ) ;
#15366 = VERTEX_POINT ( 'NONE', #35626 ) ;
#15367 = CARTESIAN_POINT ( 'NONE',  ( 80.96289755590194659, 61.39497013797979008, -2.048264032867926687 ) ) ;
#15368 =( BOUNDED_CURVE ( )  B_SPLINE_CURVE ( 3, ( #17575, #7520, #17371, #4644 ),
 .UNSPECIFIED., .F., .F. ) 
 B_SPLINE_CURVE_WITH_KNOTS ( ( 4, 4 ),
 ( 4.712388980384689674, 4.895802057644191407 ),
 .UNSPECIFIED. ) 
 CURVE ( )  GEOMETRIC_REPRESENTATION_ITEM ( )  RATIONAL_B_SPLINE_CURVE ( ( 1.000000000000000000, 0.9971986010846198845, 0.9971986010846198845, 1.000000000000000000 ) ) 
 REPRESENTATION_ITEM ( '' )  );
#15369 = CARTESIAN_POINT ( 'NONE',  ( -1.748552835046873311, -28.97426312752735811, 7.756742906098587298 ) ) ;
#15370 = CARTESIAN_POINT ( 'NONE',  ( 78.87073352949229843, 65.61655597148102004, 2.590854534519452024 ) ) ;
#15372 = ORIENTED_EDGE ( 'NONE', *, *, #35111, .T. ) ;
#15371 = CARTESIAN_POINT ( 'NONE',  ( -1.336220785630046981, -31.09930730182104242, 6.903372536218455480 ) ) ;
#15373 = VECTOR ( 'NONE', #36935, 1000.000000000000000 ) ;
#15374 = VECTOR ( 'NONE', #1879, 1000.000000000000000 ) ;
#15375 = CARTESIAN_POINT ( 'NONE',  ( -59.01453825321729596, 27.97194601286735960, 6.240525879293456590 ) ) ;
#15377 = CARTESIAN_POINT ( 'NONE',  ( -63.05048152672962658, 38.43432252562774210, -4.010992198732260761 ) ) ;
#15376 = CARTESIAN_POINT ( 'NONE',  ( 4.927610109650206738, -30.92457071343696384, 7.013842709614101167 ) ) ;
#15378 = CARTESIAN_POINT ( 'NONE',  ( -51.01549048184568846, -30.38627270959228710, 6.800000000000000711 ) ) ;
#15379 = EDGE_CURVE ( 'NONE', #38060, #7364, #32357, .T. ) ;
#15380 = ADVANCED_FACE ( 'NONE', ( #29436 ), #7582, .T. ) ;
#15381 = CARTESIAN_POINT ( 'NONE',  ( 21.71185578408363881, 6.328645931448866335, 3.192210964217056191 ) ) ;
#15382 = CARTESIAN_POINT ( 'NONE',  ( 22.44128072547340125, 4.727156261423415273, -3.200930849007907586 ) ) ;
#15383 = ORIENTED_EDGE ( 'NONE', *, *, #19766, .F. ) ;
#15384 = DIRECTION ( 'NONE',  ( -7.232507224765808510E-18, 1.000000000000000000, 0.000000000000000000 ) ) ;
#15385 = ADVANCED_FACE ( 'NONE', ( #9632 ), #18903, .F. ) ;
#15386 = VECTOR ( 'NONE', #3003, 1000.000000000000000 ) ;
#15387 = CARTESIAN_POINT ( 'NONE',  ( 25.48535437492803624, -4.309695067542732794, -2.926019122942394191 ) ) ;
#15388 = CARTESIAN_POINT ( 'NONE',  ( -79.68766234410863092, -5.608549218928701841, -4.839603289619596183 ) ) ;
#15389 = FACE_OUTER_BOUND ( 'NONE', #26315, .T. ) ;
#15390 = CARTESIAN_POINT ( 'NONE',  ( 80.79838846785789030, 64.52093256242035579, 3.402511877379641891 ) ) ;
#15391 = CARTESIAN_POINT ( 'NONE',  ( 88.27260010123318068, -2.240648412321151639, -1.886171102315310266 ) ) ;
#15392 = CARTESIAN_POINT ( 'NONE',  ( 14.78134360068729336, 12.96929629928027516, 2.499999999999999112 ) ) ;
#15393 = VERTEX_POINT ( 'NONE', #22414 ) ;
#15394 = CARTESIAN_POINT ( 'NONE',  ( -64.24896514350277243, 34.84424003550355309, -5.066824151024967193 ) ) ;
#15395 = CARTESIAN_POINT ( 'NONE',  ( 5.028764603308605530, -28.48812247857538438, 7.754798119455333705 ) ) ;
#15396 = CARTESIAN_POINT ( 'NONE',  ( 4.089396484546625743, -27.01207004994921590, 6.921725064902951807 ) ) ;
#15397 = CARTESIAN_POINT ( 'NONE',  ( -0.9919418010453353585, -27.33356058713898307, 7.750000000000000888 ) ) ;
#15398 = CARTESIAN_POINT ( 'NONE',  ( -65.27430759792098058, 36.41843883184579056, -8.800656633793916939 ) ) ;
#15399 = DIRECTION ( 'NONE',  ( 0.000000000000000000, 0.000000000000000000, 1.000000000000000000 ) ) ;
#15400 = CARTESIAN_POINT ( 'NONE',  ( 1.864984047224969688, -26.17390644987066040, 6.876076431790004939 ) ) ;
#15401 = CARTESIAN_POINT ( 'NONE',  ( 35.33522214168899467, -3.170233168067363216, 5.721314019424172059 ) ) ;
#15402 = CARTESIAN_POINT ( 'NONE',  ( 85.14289959633329374, 2.721178644307868044, -0.4516327360412458747 ) ) ;
#15403 = ORIENTED_EDGE ( 'NONE', *, *, #37238, .F. ) ;
#15405 = CARTESIAN_POINT ( 'NONE',  ( 0.08532122990943709351, 0.5999999999999996447, 3.903274794823348159 ) ) ;
#15404 = CARTESIAN_POINT ( 'NONE',  ( 81.24448906778437163, 62.55865020921709885, -3.071811904357653500 ) ) ;
#15406 = CARTESIAN_POINT ( 'NONE',  ( -1.326458086256048663, -31.32451895819955112, 7.762796336881259585 ) ) ;
#15407 = CARTESIAN_POINT ( 'NONE',  ( 17.26328941701764919, -2.999363701367865787, 2.900751846394634459 ) ) ;
#15408 = CARTESIAN_POINT ( 'NONE',  ( -1.268168650321787716, -31.22753658603060956, 6.894806418505346812 ) ) ;
#15409 = ORIENTED_EDGE ( 'NONE', *, *, #22662, .T. ) ;
#15410 = CARTESIAN_POINT ( 'NONE',  ( 27.36782613089871674, -4.434391534612712960, -3.677648743169859902 ) ) ;
#15411 = ORIENTED_EDGE ( 'NONE', *, *, #8639, .T. ) ;
#15412 = VERTEX_POINT ( 'NONE', #15397 ) ;
#15413 = CARTESIAN_POINT ( 'NONE',  ( 81.15742489870845588, 61.60174059333855467, -2.174925636353718161 ) ) ;
#15414 = CARTESIAN_POINT ( 'NONE',  ( -1.505759322122861787, -28.43828526875796214, 7.670860738520326905 ) ) ;
#15415 = EDGE_LOOP ( 'NONE', ( #18284, #5927, #19344, #39993 ) ) ;
#15417 = CARTESIAN_POINT ( 'NONE',  ( 21.56339383302955071, 7.351415377951304286, -2.885032705794761121 ) ) ;
#15416 = CARTESIAN_POINT ( 'NONE',  ( 22.04653420616095616, 3.143092986063939165, 4.783053969572811148 ) ) ;
#15418 = ORIENTED_EDGE ( 'NONE', *, *, #14390, .T. ) ;
#15419 = EDGE_CURVE ( 'NONE', #38102, #513, #40498, .T. ) ;
#15420 = CARTESIAN_POINT ( 'NONE',  ( 79.73837173991832117, 66.20136991484926625, -1.918505602738486138 ) ) ;
#15421 = ADVANCED_FACE ( 'NONE', ( #9839 ), #34373, .F. ) ;
#15422 = CARTESIAN_POINT ( 'NONE',  ( 4.748933141249126244, -31.28934451117660487, 7.710604733652628440 ) ) ;
#15423 = B_SPLINE_CURVE_WITH_KNOTS ( 'NONE', 3,
 ( #40597, #30955, #34261, #2759, #15285, #40391, #37310, #9106, #6032, #18566, #31153, #13826, #25784, #25987 ),
 .UNSPECIFIED., .F., .F.,
 ( 4, 2, 2, 2, 2, 2, 4 ),
 ( 0.000000000000000000, 0.0008966178941042668047, 0.001793235788208533609, 0.002241544735260675957, 0.002689853682312818087, 0.003138162629364960217, 0.003586471576417102347 ),
 .UNSPECIFIED. ) ;
#15425 = DIRECTION ( 'NONE',  ( -1.000000000000000000, -7.232507224765808510E-18, 0.000000000000000000 ) ) ;
#15424 = CARTESIAN_POINT ( 'NONE',  ( -70.42444715658567134, 0.09064798068341432813, 5.980032331837195514 ) ) ;
#15426 = CARTESIAN_POINT ( 'NONE',  ( 2.105750943142600029, -32.94567937155306225, 7.013842709614101167 ) ) ;
#15427 = CARTESIAN_POINT ( 'NONE',  ( -69.46331044089802731, 37.03771852125571229, 8.800414904976364028 ) ) ;
#15428 = CARTESIAN_POINT ( 'NONE',  ( 74.86006972221214539, 59.87270642427901635, 3.642458757454619889 ) ) ;
#15429 = CARTESIAN_POINT ( 'NONE',  ( 22.04016737215521360, 3.514630979057402183, -4.507021302255509454 ) ) ;
#15430 = ORIENTED_EDGE ( 'NONE', *, *, #18405, .T. ) ;
#15431 = ADVANCED_FACE ( 'NONE', ( #3693 ), #34581, .F. ) ;
#15432 = VECTOR ( 'NONE', #17554, 1000.000000000000000 ) ;
#15433 = CARTESIAN_POINT ( 'NONE',  ( 21.85643539959776760, 8.340603020592608274, -8.602649199348869402 ) ) ;
#15434 = AXIS2_PLACEMENT_3D ( 'NONE', #22767, #29134, #25034 ) ;
#15435 = CARTESIAN_POINT ( 'NONE',  ( 3.536390127705351993, -26.59562449125457917, 7.771081512783702294 ) ) ;
#15436 = ORIENTED_EDGE ( 'NONE', *, *, #8507, .F. ) ;
#15437 = CARTESIAN_POINT ( 'NONE',  ( 1.064090257649125792, -26.12825580611192677, 7.730015791551948290 ) ) ;
#15438 = CARTESIAN_POINT ( 'NONE',  ( 79.78729094670487143, 65.99503481514538805, 2.368810654844614394 ) ) ;
#15439 = AXIS2_PLACEMENT_3D ( 'NONE', #9785, #31827, #19667 ) ;
#15440 = CARTESIAN_POINT ( 'NONE',  ( 87.34576652878352832, 0.2468139514080059382, -4.863684402402743245 ) ) ;
#15441 = ORIENTED_EDGE ( 'NONE', *, *, #3264, .F. ) ;
#15442 = AXIS2_PLACEMENT_3D ( 'NONE', #18294, #33772, #24063 ) ;
#15443 = CARTESIAN_POINT ( 'NONE',  ( -22.87867591359218977, -24.55319635012989110, 6.800000000000000711 ) ) ;
#15444 = ORIENTED_EDGE ( 'NONE', *, *, #12595, .F. ) ;
#15445 = CARTESIAN_POINT ( 'NONE',  ( 28.88870476122235331, -3.262720734457520422, 4.666716578517512204 ) ) ;
#15446 = CARTESIAN_POINT ( 'NONE',  ( 21.53525696227849551, 7.395501062873577780, -0.9772312434468740650 ) ) ;
#15447 = CARTESIAN_POINT ( 'NONE',  ( 34.93088199418607331, -1.706447725614655520, -5.658206960402972996 ) ) ;
#15448 = CARTESIAN_POINT ( 'NONE',  ( 5.144595142829149204, -29.03130177782659160, 7.784725160561909441 ) ) ;
#15449 = CARTESIAN_POINT ( 'NONE',  ( -1.348517286369408597, -27.85116208076715694, 7.697032948437507294 ) ) ;
#15450 = ORIENTED_EDGE ( 'NONE', *, *, #36484, .F. ) ;
#15451 = DIRECTION ( 'NONE',  ( -0.5171480877355195682, 0.2439873919671761981, 0.8203828422831326295 ) ) ;
#15452 = CARTESIAN_POINT ( 'NONE',  ( -1.225953191357326499, -31.30097466021442187, 7.703977250142848732 ) ) ;
#15453 = VERTEX_POINT ( 'NONE', #28581 ) ;
#15454 = CARTESIAN_POINT ( 'NONE',  ( 36.20082885389868466, -3.649409372564311305, 5.718625934384519383 ) ) ;
#15455 = CARTESIAN_POINT ( 'NONE',  ( -71.77605803285275954, -0.2407680685837292611, 3.940028962036595139 ) ) ;
#15456 = VERTEX_POINT ( 'NONE', #38036 ) ;
#15457 = CARTESIAN_POINT ( 'NONE',  ( 66.74698822326750758, 57.80221319398844315, -3.998057522770657624 ) ) ;
#15458 = CARTESIAN_POINT ( 'NONE',  ( 87.64754863977299237, -2.175244042755086760, -2.906226134380668125 ) ) ;
#15459 = AXIS2_PLACEMENT_3D ( 'NONE', #23838, #36413, #2675 ) ;
#15460 = ORIENTED_EDGE ( 'NONE', *, *, #33958, .T. ) ;
#15461 = TOROIDAL_SURFACE ( 'NONE', #20714, 67.42751648247021024, 3.000000000000000000 ) ;
#15462 = CARTESIAN_POINT ( 'NONE',  ( -55.43956553351903693, 30.97124788692904218, 1.442063311134026637 ) ) ;
#15463 = DIRECTION ( 'NONE',  ( -0.000000000000000000, -0.000000000000000000, 1.000000000000000000 ) ) ;
#15464 = CARTESIAN_POINT ( 'NONE',  ( 74.91345620096926439, 63.41934653362798713, 3.016809678508692194 ) ) ;
#15465 = CARTESIAN_POINT ( 'NONE',  ( -40.87867591359218977, -26.64985754041175525, 6.800000000000000711 ) ) ;
#15466 = CARTESIAN_POINT ( 'NONE',  ( 1.700390093233090871, -29.56993018339339940, 6.850000000000000533 ) ) ;
#15467 = VERTEX_POINT ( 'NONE', #6759 ) ;
#15468 = CARTESIAN_POINT ( 'NONE',  ( 24.03052928095394591, 3.323090062041115011, 3.304702637807089172 ) ) ;
#15469 = VECTOR ( 'NONE', #26062, 1000.000000000000000 ) ;
#15470 = CARTESIAN_POINT ( 'NONE',  ( 79.32563386639210989, 66.29995228605847046, -1.174937739208586907 ) ) ;
#15471 = CARTESIAN_POINT ( 'NONE',  ( 78.64144163184205638, 66.02383098553904972, 1.235082213173782195 ) ) ;
#15472 = FACE_OUTER_BOUND ( 'NONE', #28042, .T. ) ;
#15473 = ORIENTED_EDGE ( 'NONE', *, *, #38202, .F. ) ;
#15474 = CARTESIAN_POINT ( 'NONE',  ( 77.45380151126717294, 63.20247531706575472, -3.748203062644118067 ) ) ;
#15476 = CARTESIAN_POINT ( 'NONE',  ( 0.01877809797159043712, -0.6000000000000005329, 3.829374602102926239 ) ) ;
#15475 = DIRECTION ( 'NONE',  ( 0.9396926207859001012, 0.3420201433256914170, 0.000000000000000000 ) ) ;
#15477 = CARTESIAN_POINT ( 'NONE',  ( 17.79339514573547376, 8.594434151433056002, -2.958563574914779615 ) ) ;
#15478 = CARTESIAN_POINT ( 'NONE',  ( 79.45632949585312588, 65.80330994668889844, -2.596981798947360254 ) ) ;
#15479 = CARTESIAN_POINT ( 'NONE',  ( 78.06740453511714861, 61.95427634543516149, 3.748203062644153150 ) ) ;
#15480 = ORIENTED_EDGE ( 'NONE', *, *, #11400, .T. ) ;
#15481 = EDGE_CURVE ( 'NONE', #38247, #40564, #21265, .T. ) ;
#15482 = EDGE_CURVE ( 'NONE', #33264, #2584, #6561, .T. ) ;
#15483 = CARTESIAN_POINT ( 'NONE',  ( 2.304086713256504382, -32.91590543598751850, 7.635761828346577573 ) ) ;
#15484 = EDGE_CURVE ( 'NONE', #25871, #7218, #37613, .T. ) ;
#15485 = CARTESIAN_POINT ( 'NONE',  ( -57.44572001938779238, 32.97690117809874977, 4.025720541963821120 ) ) ;
#15486 = CARTESIAN_POINT ( 'NONE',  ( 80.49077247797930568, 66.09228938494877070, 1.971256063808053627 ) ) ;
#15487 = B_SPLINE_CURVE_WITH_KNOTS ( 'NONE', 3,
 ( #1811, #17619, #36984, #5086, #2216, #14534, #39658, #5289, #14736, #14955, #5701, #21145, #23803, #39870, #39449, #17413, #27521, #14336, #18035, #20932, #8357, #15159, #26906, #2017, #11238, #5491, #40075, #11854, #8149, #33712, #24633 ),
 .UNSPECIFIED., .F., .F.,
 ( 4, 3, 3, 3, 3, 3, 3, 3, 3, 3, 4 ),
 ( 2.531095456908227149E-18, 3.077658087705945685E-05, 6.152638666999577953E-05, 9.267501192706705719E-05, 0.0001241882240135256765, 0.0001556618703051725191, 0.0001866161554452253123, 0.0002167966385861005865, 0.0002463805737537804711, 0.0002758761370306588869, 0.0002847094172290117711 ),
 .UNSPECIFIED. ) ;
#15489 = DIRECTION ( 'NONE',  ( 0.8660254037844380415, 0.5000000000000009992, -0.000000000000000000 ) ) ;
#15488 = CARTESIAN_POINT ( 'NONE',  ( -16.87867591359218977, -24.55319635012989110, 6.700000000000000178 ) ) ;
#15490 = CARTESIAN_POINT ( 'NONE',  ( 28.73718198699435433, 0.3327373454474676917, -5.564570571917969666 ) ) ;
#15491 = CARTESIAN_POINT ( 'NONE',  ( -1.400655036095836525, -31.19274228153209805, 6.875780273367530171 ) ) ;
#15492 = DIRECTION ( 'NONE',  ( 0.000000000000000000, 0.000000000000000000, 1.000000000000000000 ) ) ;
#15493 = CARTESIAN_POINT ( 'NONE',  ( -64.17177837788707961, 36.63861034030102815, 5.251833000746531255 ) ) ;
#15494 = CARTESIAN_POINT ( 'NONE',  ( 26.64541687229243294, 1.018703328949602138, -4.378789651849845477 ) ) ;
#15495 = DIRECTION ( 'NONE',  ( -0.9267318687906771491, 0.3757233601570964532, 0.000000000000000000 ) ) ;
#15496 = ORIENTED_EDGE ( 'NONE', *, *, #22523, .F. ) ;
#15497 = CIRCLE ( 'NONE', #25350, 6.000000000000005329 ) ;
#15498 = CARTESIAN_POINT ( 'NONE',  ( -0.7622425899803056959, -33.94363691401473915, 7.695279973900954751 ) ) ;
#15499 = VECTOR ( 'NONE', #3364, 1000.000000000000000 ) ;
#15500 = CARTESIAN_POINT ( 'NONE',  ( 0.5312670209085799122, -32.86889349860920362, 7.660770905198776681 ) ) ;
#15501 = DIRECTION ( 'NONE',  ( -0.000000000000000000, -0.000000000000000000, 1.000000000000000000 ) ) ;
#15502 = CARTESIAN_POINT ( 'NONE',  ( 37.17267509869564890, -2.956902742721974953, -5.999791034500704612 ) ) ;
#15503 = CARTESIAN_POINT ( 'NONE',  ( 81.16957891225059996, 61.30398062001309256, -1.000000000000000000 ) ) ;
#15504 = CARTESIAN_POINT ( 'NONE',  ( 5.078421676527827167, -29.18405115796800331, 6.929923840112063971 ) ) ;
#15505 = CARTESIAN_POINT ( 'NONE',  ( -0.9551886663611179884, -31.69313230502388024, 7.782034975670474530 ) ) ;
#15506 =( BOUNDED_SURFACE ( )  B_SPLINE_SURFACE ( 3, 2, ( 
 ( #4649, #1566, #29359 ),
 ( #13712, #14096, #39210 ),
 ( #10998, #14502, #2393 ),
 ( #33266, #40036, #14918 ),
 ( #18000, #1982, #24187 ),
 ( #24595, #14699, #24392 ),
 ( #21522, #36951, #34097 ),
 ( #15122, #30162, #39413 ),
 ( #11608, #5251, #17579 ),
 ( #33679, #5049, #11203 ),
 ( #8528, #36743, #36344 ),
 ( #30585, #30998, #21111 ),
 ( #14299, #27077, #8112 ),
 ( #39622, #23969, #2181 ),
 ( #11809, #11403, #20681 ),
 ( #27268, #8320, #40234 ),
 ( #5459, #27486, #8938 ),
 ( #20894, #33480, #8730 ) ),
 .UNSPECIFIED., .F., .F., .T. ) 
 B_SPLINE_SURFACE_WITH_KNOTS ( ( 4, 2, 2, 2, 2, 2, 2, 2, 4 ),
 ( 3, 3 ),
 ( 0.1120466800099417792, 0.1143735122104352075, 0.1149552202605585716, 0.1151006472730894126, 0.1151733607793548331, 0.1152460742856202536, 0.1155369283106819356, 0.1167003444109286497, 0.1213540088119155202 ),
 ( 0.4204862958135378581, 1.000000000000000000 ),
 .UNSPECIFIED. ) 
 GEOMETRIC_REPRESENTATION_ITEM ( )  RATIONAL_B_SPLINE_SURFACE ( (
 ( 0.9643893222201109783, 0.9576553645928089775, 1.000000000000000000),
 ( 0.9643512025059277626, 0.9576100364637323281, 1.000000000000000000),
 ( 0.9643130339552848929, 0.9575646502632511048, 1.000000000000000000),
 ( 0.9642652639231832357, 0.9575078469469748832, 1.000000000000000000),
 ( 0.9642557069497447175, 0.9574964827556402547, 1.000000000000000000),
 ( 0.9642437570514184042, 0.9574822731387686581, 1.000000000000000000),
 ( 0.9642413668876821387, 0.9574794309965157790, 1.000000000000000000),
 ( 0.9642377813664757547, 0.9574751674554182745, 1.000000000000000000),
 ( 0.9642387421108769008, 0.9574763098760044056, 1.000000000000000000),
 ( 0.9642387421108769008, 0.9574763098760044056, 1.000000000000000000),
 ( 0.9642387421108765677, 0.9574763098760041835, 1.000000000000000000),
 ( 0.9642387421108765677, 0.9574763098760041835, 1.000000000000000000),
 ( 0.9642387421108769008, 0.9574763098760044056, 1.000000000000000000),
 ( 0.9642387421108769008, 0.9574763098760044056, 1.000000000000000000),
 ( 0.9642387421108769008, 0.9574763098760044056, 1.000000000000000000),
 ( 0.9642387421108769008, 0.9574763098760044056, 1.000000000000000000),
 ( 0.9642387421108769008, 0.9574763098760044056, 1.000000000000000000),
 ( 0.9642387421108769008, 0.9574763098760044056, 1.000000000000000000) ) ) 
 REPRESENTATION_ITEM ( '' )  SURFACE ( )  );
#15507 = DIRECTION ( 'NONE',  ( -0.000000000000000000, -0.000000000000000000, -1.000000000000000000 ) ) ;
#15508 = DIRECTION ( 'NONE',  ( -0.000000000000000000, -1.000000000000000000, -0.000000000000000000 ) ) ;
#15509 = CARTESIAN_POINT ( 'NONE',  ( 2.098952397805311065, -32.94648879970292654, 6.903372536218458144 ) ) ;
#15510 = VECTOR ( 'NONE', #27833, 1000.000000000000114 ) ;
#15511 = CARTESIAN_POINT ( 'NONE',  ( 87.06807637922989329, 0.009568187950425697044, -5.830412620327568796 ) ) ;
#15512 = CARTESIAN_POINT ( 'NONE',  ( 2.829405163535267942, -26.36285597610873310, 7.695279973900954751 ) ) ;
#15513 = CARTESIAN_POINT ( 'NONE',  ( -1.516055275688932502, -30.67199249048969278, 6.880147297696980857 ) ) ;
#15514 = ORIENTED_EDGE ( 'NONE', *, *, #3095, .T. ) ;
#15515 = ORIENTED_EDGE ( 'NONE', *, *, #22898, .T. ) ;
#15516 = LINE ( 'NONE', #6259, #16645 ) ;
#15517 = CARTESIAN_POINT ( 'NONE',  ( 69.55412262724962602, 59.60600320152340004, -3.916752429509892774 ) ) ;
#15518 = EDGE_LOOP ( 'NONE', ( #34821, #2438, #22012, #4159 ) ) ;
#15519 = CARTESIAN_POINT ( 'NONE',  ( -2.972149592069638580, -28.62058083279596588, 6.954324564059724878 ) ) ;
#15520 = DIRECTION ( 'NONE',  ( -0.7660444431189813441, 0.6427876096865353661, -0.000000000000000000 ) ) ;
#15521 = PRODUCT ( 'Press Pin', 'Press Pin', '', ( #29549 ) ) ;
#15522 = CARTESIAN_POINT ( 'NONE',  ( 4.860131460834224981, -30.82536650786092380, 7.774064877406526186 ) ) ;
#15523 = DIRECTION ( 'NONE',  ( 1.000000000000000000, 0.000000000000000000, 0.000000000000000000 ) ) ;
#15524 = EDGE_LOOP ( 'NONE', ( #40146, #37659, #9423, #18500, #14144 ) ) ;
#15525 = CARTESIAN_POINT ( 'NONE',  ( 23.43876222436442802, 3.796239004519351923, 3.093510792665742137 ) ) ;
#15526 = DIRECTION ( 'NONE',  ( -1.000000000000000000, 0.000000000000000000, 0.000000000000000000 ) ) ;
#15527 = CARTESIAN_POINT ( 'NONE',  ( 18.65469762088386574, -3.106616286309057617, 3.066837553255504556 ) ) ;
#15528 = AXIS2_PLACEMENT_3D ( 'NONE', #3510, #38258, #410 ) ;
#15529 = ORIENTED_EDGE ( 'NONE', *, *, #12924, .F. ) ;
#15530 = VERTEX_POINT ( 'NONE', #31472 ) ;
#15531 = CARTESIAN_POINT ( 'NONE',  ( 78.83212471655066622, 64.69929012837440041, -3.375657603866064616 ) ) ;
#15533 = CYLINDRICAL_SURFACE ( 'NONE', #24321, 3.399999999999999911 ) ;
#15532 = CARTESIAN_POINT ( 'NONE',  ( 24.67241584745087479, 0.7088272946872185010, 4.794457209858541624 ) ) ;
#15534 = CARTESIAN_POINT ( 'NONE',  ( 81.10335266982598057, 65.07249684831452896, -2.967158453529146644 ) ) ;
#15535 = CARTESIAN_POINT ( 'NONE',  ( 79.38338525671692025, 64.07937768075930762, 3.690346394509879335 ) ) ;
#15536 = CIRCLE ( 'NONE', #7016, 0.1000000000000028644 ) ;
#15537 = CARTESIAN_POINT ( 'NONE',  ( 0.000000000000000000, 0.000000000000000000, 2.500000000000000000 ) ) ;
#15538 = EDGE_CURVE ( 'NONE', #1735, #8999, #15195, .T. ) ;
#15539 = CARTESIAN_POINT ( 'NONE',  ( 80.03496335128151884, 66.36160760684386162, 1.000000000000000000 ) ) ;
#15540 = CARTESIAN_POINT ( 'NONE',  ( 4.668540769505296950, -31.42424039273510061, 7.754798119455333705 ) ) ;
#15541 = CARTESIAN_POINT ( 'NONE',  ( 21.85643539959774628, 5.695295784951009743, -9.764639101464164028 ) ) ;
#15542 = CARTESIAN_POINT ( 'NONE',  ( -1.250824363190944588, -27.88163718980674233, 7.635761828346577573 ) ) ;
#15543 = ORIENTED_EDGE ( 'NONE', *, *, #7725, .F. ) ;
#15544 = CARTESIAN_POINT ( 'NONE',  ( -72.05672345664538625, 4.865640908481359439, 9.936545240694519165 ) ) ;
#15545 = CARTESIAN_POINT ( 'NONE',  ( -0.5767923600352592439, -26.91202874155498037, 7.695279973900954751 ) ) ;
#15546 = ORIENTED_EDGE ( 'NONE', *, *, #17643, .T. ) ;
#15547 = FACE_BOUND ( 'NONE', #40416, .T. ) ;
#15548 = CARTESIAN_POINT ( 'NONE',  ( -80.68923699068490407, 10.55697554841911590, -2.212078010654421334 ) ) ;
#15549 = CARTESIAN_POINT ( 'NONE',  ( 1.646554145741061737, -32.96950506480602883, 6.889465824494256374 ) ) ;
#15550 = CARTESIAN_POINT ( 'NONE',  ( 27.81823897074509233, 1.847144674410869936, -3.899787536903625895 ) ) ;
#15551 = DIRECTION ( 'NONE',  ( -0.000000000000000000, -0.000000000000000000, -1.000000000000000000 ) ) ;
#15552 = CARTESIAN_POINT ( 'NONE',  ( 14.74910353868988899, 12.91027092149337641, 2.503635293877921164 ) ) ;
#15553 = CARTESIAN_POINT ( 'NONE',  ( -41.07867591359219972, -24.55319635012989110, 6.700000000000000178 ) ) ;
#15554 = LINE ( 'NONE', #5891, #17464 ) ;
#15555 = CARTESIAN_POINT ( 'NONE',  ( 5.043527284170251868, -28.95070318796772213, 7.730758795053806587 ) ) ;
#15556 = CARTESIAN_POINT ( 'NONE',  ( -12.44874870218064267, -26.64985754041175525, 6.700000000000000178 ) ) ;
#15557 = CARTESIAN_POINT ( 'NONE',  ( 26.39112261854958064, 1.214606541396050066, -4.362303127903641276 ) ) ;
#15558 = CARTESIAN_POINT ( 'NONE',  ( 30.97689734888565383, -3.765698233401996387, -4.598238574220234298 ) ) ;
#15559 = CARTESIAN_POINT ( 'NONE',  ( 25.99837217835952075, 1.969169038965218332, -4.208579848621752717 ) ) ;
#15560 = ORIENTED_EDGE ( 'NONE', *, *, #17986, .T. ) ;
#15562 = ORIENTED_EDGE ( 'NONE', *, *, #2067, .T. ) ;
#15561 = CONICAL_SURFACE ( 'NONE', #20809, 6.138794830819693793, 0.03429555972217021576 ) ;
#15563 = CARTESIAN_POINT ( 'NONE',  ( 67.00793363329040631, 57.99808316372624972, 3.999354069328931782 ) ) ;
#15564 = CARTESIAN_POINT ( 'NONE',  ( 21.30795797853340900, 3.457867745315728047, 3.532020196095992493 ) ) ;
#15565 = EDGE_CURVE ( 'NONE', #38692, #11094, #21982, .T. ) ;
#15567 = CARTESIAN_POINT ( 'NONE',  ( 4.964848989002191182, -30.79572542994174000, 7.783750581861601070 ) ) ;
#15566 = AXIS2_PLACEMENT_3D ( 'NONE', #7842, #19995, #10715 ) ;
#15568 = CARTESIAN_POINT ( 'NONE',  ( -1.060034464505671403, -31.72168673584834053, 7.750000000000000888 ) ) ;
#15569 = CARTESIAN_POINT ( 'NONE',  ( 85.30740962031771346, 1.871039318281703334, 5.038373847784950676 ) ) ;
#15571 = CARTESIAN_POINT ( 'NONE',  ( 35.94856560473117923, -2.120269416292473785, -5.817041100599634973 ) ) ;
#15570 = VECTOR ( 'NONE', #18414, 1000.000000000000000 ) ;
#15572 = ORIENTED_EDGE ( 'NONE', *, *, #1296, .T. ) ;
#15573 = CARTESIAN_POINT ( 'NONE',  ( 25.19497952292325493, 2.388040330658791621, 4.036871176649600379 ) ) ;
#15574 = DIRECTION ( 'NONE',  ( 1.000000000000000000, 0.000000000000000000, 0.000000000000000000 ) ) ;
#15575 = FACE_OUTER_BOUND ( 'NONE', #3421, .T. ) ;
#15576 = VERTEX_POINT ( 'NONE', #1397 ) ;
#15577 = CYLINDRICAL_SURFACE ( 'NONE', #30680, 0.1000000000000028644 ) ;
#15578 = EDGE_CURVE ( 'NONE', #13284, #4251, #38380, .T. ) ;
#15579 = ORIENTED_EDGE ( 'NONE', *, *, #24794, .F. ) ;
#15580 = CARTESIAN_POINT ( 'NONE',  ( 78.59417545055856635, 65.93066236947775849, -1.724274471760826488 ) ) ;
#15581 = CARTESIAN_POINT ( 'NONE',  ( -1.698895226757518362, -29.49949936766056169, 7.784476445165074310 ) ) ;
#15582 = CARTESIAN_POINT ( 'NONE',  ( 80.77881921633029094, 62.12902493665696824, 3.041370705153006337 ) ) ;
#15584 = EDGE_LOOP ( 'NONE', ( #16664, #27963, #17029, #26122 ) ) ;
#15583 = CARTESIAN_POINT ( 'NONE',  ( -0.8674134075260871990, -27.34139138375608979, 6.887041543973313473 ) ) ;
#15585 = AXIS2_PLACEMENT_3D ( 'NONE', #38676, #17244, #4324 ) ;
#15586 = CARTESIAN_POINT ( 'NONE',  ( 0.02975571862627216652, -26.50603724034379383, 7.780491323090173772 ) ) ;
#15587 = EDGE_CURVE ( 'NONE', #18339, #30328, #25691, .T. ) ;
#15589 = CARTESIAN_POINT ( 'NONE',  ( -64.08758708074093136, 38.34280096101419844, -3.014656224624829850 ) ) ;
#15588 = CARTESIAN_POINT ( 'NONE',  ( -2.978675913592195190, -24.55319635012989110, 6.700000000000000178 ) ) ;
#15590 = CARTESIAN_POINT ( 'NONE',  ( -71.18984706668749141, -21.75705254805669853, 9.997314914349638926 ) ) ;
#15591 =( GEOMETRIC_REPRESENTATION_CONTEXT ( 3 ) GLOBAL_UNCERTAINTY_ASSIGNED_CONTEXT ( ( #24225 ) ) GLOBAL_UNIT_ASSIGNED_CONTEXT ( ( #4937, #13804, #10499 ) ) REPRESENTATION_CONTEXT ( 'NONE', 'WORKASPACE' ) );
#15592 = CARTESIAN_POINT ( 'NONE',  ( -16.34874870218063592, -26.64985754041175525, 6.700000000000000178 ) ) ;
#15593 = CARTESIAN_POINT ( 'NONE',  ( 23.14704033844979492, 3.979479066984730640, -3.185135796097247063 ) ) ;
#15594 = ORIENTED_EDGE ( 'NONE', *, *, #39787, .F. ) ;
#15595 = VECTOR ( 'NONE', #9870, 1000.000000000000000 ) ;
#15596 = CARTESIAN_POINT ( 'NONE',  ( 25.32326662574907772, -3.445015843796760624, -4.932833089913290614 ) ) ;
#15597 = CARTESIAN_POINT ( 'NONE',  ( -77.45835083621990691, -4.875850942340420602, -9.162514641918679814 ) ) ;
#15598 = CARTESIAN_POINT ( 'NONE',  ( 5.010951146761534858, -30.34466785830838376, 6.895222827070022653 ) ) ;
#15599 = CARTESIAN_POINT ( 'NONE',  ( 81.24747667583794453, 63.59436251574997101, 3.343039074470570693 ) ) ;
#15600 = CARTESIAN_POINT ( 'NONE',  ( 86.69339609521894374, -0.1977197225095213562, 5.906572220802119411 ) ) ;
#15601 = CYLINDRICAL_SURFACE ( 'NONE', #12135, 0.09010775117053032579 ) ;
#15602 = ORIENTED_EDGE ( 'NONE', *, *, #11462, .F. ) ;
#15603 = PLANE ( 'NONE',  #34605 ) ;
#15604 = FACE_OUTER_BOUND ( 'NONE', #18466, .T. ) ;
#15605 = EDGE_CURVE ( 'NONE', #37831, #16241, #38745, .T. ) ;
#15606 = CARTESIAN_POINT ( 'NONE',  ( 4.093933310419832772, -27.01631492900221687, 6.951256099901589991 ) ) ;
#15607 = CARTESIAN_POINT ( 'NONE',  ( -1.744066689084928345, -30.19099175420856440, 7.635761828346576685 ) ) ;
#15608 = DIRECTION ( 'NONE',  ( 0.000000000000000000, 0.000000000000000000, 1.000000000000000000 ) ) ;
#15609 = DIRECTION ( 'NONE',  ( 0.000000000000000000, 0.000000000000000000, -1.000000000000000000 ) ) ;
#15610 = ORIENTED_EDGE ( 'NONE', *, *, #2071, .F. ) ;
#15611 = CARTESIAN_POINT ( 'NONE',  ( 34.33227999214794579, -1.487593080494464592, 5.564780640740604412 ) ) ;
#15612 = CARTESIAN_POINT ( 'NONE',  ( -71.92837670882107659, -0.7829914368874774100, 5.916079783099621459 ) ) ;
#15613 = ORIENTED_EDGE ( 'NONE', *, *, #1468, .F. ) ;
#15615 = DIRECTION ( 'NONE',  ( 0.000000000000000000, 0.000000000000000000, 1.000000000000000000 ) ) ;
#15614 = CARTESIAN_POINT ( 'NONE',  ( 80.31657930512767507, 64.64970693426512582, -3.487490852634256733 ) ) ;
#15616 = EDGE_CURVE ( 'NONE', #27554, #35439, #29833, .T. ) ;
#15617 = AXIS2_PLACEMENT_3D ( 'NONE', #3653, #31232, #13286 ) ;
#15618 = ADVANCED_FACE ( 'NONE', ( #26303 ), #13927, .T. ) ;
#15619 = DIRECTION ( 'NONE',  ( 1.000000000000000000, 0.000000000000000000, 0.000000000000000000 ) ) ;
#15620 = CIRCLE ( 'NONE', #5748, 0.1000000000000028644 ) ;
#15621 = VECTOR ( 'NONE', #2035, 1000.000000000000114 ) ;
#15622 = ORIENTED_EDGE ( 'NONE', *, *, #19078, .T. ) ;
#15623 = EDGE_CURVE ( 'NONE', #1123, #31660, #16806, .T. ) ;
#15624 = CARTESIAN_POINT ( 'NONE',  ( 27.35736631516831352, -4.438324952666481416, -3.674147289654650095 ) ) ;
#15625 = ORIENTED_EDGE ( 'NONE', *, *, #27918, .F. ) ;
#15626 = CARTESIAN_POINT ( 'NONE',  ( 1.007971533865419156, -32.89869384730054236, 6.864651958020304257 ) ) ;
#15627 = VERTEX_POINT ( 'NONE', #4482 ) ;
#15628 = CARTESIAN_POINT ( 'NONE',  ( 79.73292928667240176, 64.66788176856890402, -3.497296750721717196 ) ) ;
#15629 = CARTESIAN_POINT ( 'NONE',  ( 34.93810637183052847, -3.179019197238403205, 5.659334499256591045 ) ) ;
#15630 = ORIENTED_EDGE ( 'NONE', *, *, #31064, .F. ) ;
#15632 = CARTESIAN_POINT ( 'NONE',  ( 36.10487649157640533, -1.522124056221337396, 5.639071623872836447 ) ) ;
#15631 = CARTESIAN_POINT ( 'NONE',  ( 24.00126456572668943, 2.472460351644033771, 4.166039721954374997 ) ) ;
#15633 = ORIENTED_EDGE ( 'NONE', *, *, #33161, .T. ) ;
#15634 = CARTESIAN_POINT ( 'NONE',  ( 81.23963933823222305, 65.14454330635804524, -2.817575383041753589 ) ) ;
#15635 = CARTESIAN_POINT ( 'NONE',  ( 4.907464300517769829, -30.69894525369553762, 7.695279973900954751 ) ) ;
#15636 = ADVANCED_FACE ( 'NONE', ( #38836 ), #35775, .T. ) ;
#15638 = CARTESIAN_POINT ( 'NONE',  ( 86.25914659815089180, 1.467357031587646743, -4.709363322567870824 ) ) ;
#15637 = CARTESIAN_POINT ( 'NONE',  ( 3.341357570912008246, -32.66140680771919591, 7.751599049952198506 ) ) ;
#15639 = CARTESIAN_POINT ( 'NONE',  ( -32.24874870218063450, -26.64985754041175525, 6.700000000000000178 ) ) ;
#15640 = CARTESIAN_POINT ( 'NONE',  ( 0.6020978191758283860, -26.25162571309269310, 7.771081512783698741 ) ) ;
#15641 = CARTESIAN_POINT ( 'NONE',  ( 72.96153509227066536, 61.08495594734687018, 3.864208391313482149 ) ) ;
#15642 = ORIENTED_EDGE ( 'NONE', *, *, #36258, .F. ) ;
#15643 = CARTESIAN_POINT ( 'NONE',  ( 22.41886727961536252, 3.592987785001729328, -4.133826006051191548 ) ) ;
#15644 = VERTEX_POINT ( 'NONE', #13131 ) ;
#15645 = CARTESIAN_POINT ( 'NONE',  ( -14.24874870218063450, -26.64985754041175525, 6.800000000000000711 ) ) ;
#15646 = CARTESIAN_POINT ( 'NONE',  ( 21.85643539959775339, -7.728916438363212293, -14.50668795789714771 ) ) ;
#15647 = CARTESIAN_POINT ( 'NONE',  ( 3.449253643630207922, -26.54193261727931485, 7.767720160662275219 ) ) ;
#15648 = ORIENTED_EDGE ( 'NONE', *, *, #28970, .F. ) ;
#15649 = ORIENTED_EDGE ( 'NONE', *, *, #38711, .F. ) ;
#15650 = CARTESIAN_POINT ( 'NONE',  ( -1.610418084489225299, -28.79627056164295595, 7.013842709614101167 ) ) ;
#15651 = CARTESIAN_POINT ( 'NONE',  ( 80.60418185334565067, 65.53338749785490336, 2.819252638153800117 ) ) ;
#15652 = CARTESIAN_POINT ( 'NONE',  ( 86.82658554816774199, 0.8299826706514633612, -5.353109082705294952 ) ) ;
#15653 = ORIENTED_EDGE ( 'NONE', *, *, #30609, .F. ) ;
#15654 = AXIS2_PLACEMENT_3D ( 'NONE', #35026, #31514, #25737 ) ;
#15655 = EDGE_LOOP ( 'NONE', ( #28689, #28804, #39879, #7124 ) ) ;
#15656 = CARTESIAN_POINT ( 'NONE',  ( 16.26588554675592491, -3.448400933796594625, 2.730870020955348476 ) ) ;
#15657 = CARTESIAN_POINT ( 'NONE',  ( 33.68691125750341087, -3.105118810531902085, -5.464055241398425800 ) ) ;
#15658 = CARTESIAN_POINT ( 'NONE',  ( 2.817328913877361618, -32.78123018042540338, 6.894806418505346812 ) ) ;
#15659 = CARTESIAN_POINT ( 'NONE',  ( 0.9730757925788008356, -32.99329091482906762, 7.754798119455333705 ) ) ;
#15660 = PLANE ( 'NONE',  #10554 ) ;
#15661 = ADVANCED_BREP_SHAPE_REPRESENTATION ( '', ( #39057, #30744 ), #7710 ) ;
#15662 = B_SPLINE_CURVE_WITH_KNOTS ( 'NONE', 3,
 ( #30191, #18235, #30825, #29988, #8557, #36172, #7954, #20502, #17405, #8143, #1803, #14328, #5080, #2010, #14529, #34742, #6521, #37179, #28329 ),
 .UNSPECIFIED., .F., .F.,
 ( 4, 3, 3, 3, 3, 3, 4 ),
 ( 4.336808689942017736E-19, 2.546128104244783067E-05, 5.711050680483586430E-05, 8.113074941675582901E-05, 0.0001053129305727050724, 0.0001360598016347148054, 0.0001612931755702014865 ),
 .UNSPECIFIED. ) ;
#15663 = EDGE_CURVE ( 'NONE', #10847, #32112, #35356, .T. ) ;
#15664 = ORIENTED_EDGE ( 'NONE', *, *, #3167, .T. ) ;
#15665 = ORIENTED_EDGE ( 'NONE', *, *, #10098, .T. ) ;
#15666 = CARTESIAN_POINT ( 'NONE',  ( 37.17580397388785229, -2.565365416181118352, 5.981100958229804476 ) ) ;
#15667 = CARTESIAN_POINT ( 'NONE',  ( 66.69400287465482791, 57.94980623640483230, -3.999076693785756920 ) ) ;
#15668 = CARTESIAN_POINT ( 'NONE',  ( 87.68276862112787740, -2.218184809142153657, -2.724441466588327199 ) ) ;
#15669 = B_SPLINE_CURVE_WITH_KNOTS ( 'NONE', 3,
 ( #17206, #14121, #32684, #4481, #39234, #23603, #36167, #7947, #24205, #40665 ),
 .UNSPECIFIED., .F., .F.,
 ( 4, 3, 3, 4 ),
 ( 0.0001585009270395744765, 0.0001815657551981843297, 0.0002118214035944115297, 0.0002170292169044783044 ),
 .UNSPECIFIED. ) ;
#15670 = ADVANCED_FACE ( 'NONE', ( #23604, #33503 ), #18022, .T. ) ;
#15671 = ORIENTED_EDGE ( 'NONE', *, *, #38248, .T. ) ;
#15672 = CARTESIAN_POINT ( 'NONE',  ( -57.29470892912325297, 33.22074752690817689, 3.999999999999999112 ) ) ;
#15673 = DIRECTION ( 'NONE',  ( -0.9396926207859057634, -0.3420201433256757073, -0.000000000000000000 ) ) ;
#15674 = CARTESIAN_POINT ( 'NONE',  ( -13.07867591359219617, -24.55319635012989110, 6.800000000000000711 ) ) ;
#15675 =( LENGTH_UNIT ( ) NAMED_UNIT ( * ) SI_UNIT ( .MILLI., .METRE. ) );
#15676 = ORIENTED_EDGE ( 'NONE', *, *, #24394, .F. ) ;
#15677 = FACE_BOUND ( 'NONE', #37503, .T. ) ;
#15678 = DIRECTION ( 'NONE',  ( 0.5751513419797943394, -0.4826092789263614069, 0.6605219282605379050 ) ) ;
#15679 = ORIENTED_EDGE ( 'NONE', *, *, #22196, .F. ) ;
#15680 = CARTESIAN_POINT ( 'NONE',  ( 21.84320321800310438, 5.888203138701116224, 3.167919337418751091 ) ) ;
#15681 = CARTESIAN_POINT ( 'NONE',  ( 78.99269976270092286, 66.20980237122185486, -1.093381982072927361 ) ) ;
#15682 = CARTESIAN_POINT ( 'NONE',  ( 79.44161963160776452, 65.18980684700308359, 3.197674131580388490 ) ) ;
#15683 = VERTEX_POINT ( 'NONE', #2418 ) ;
#15684 = CARTESIAN_POINT ( 'NONE',  ( 77.42503339237346438, 60.33561942134753764, -3.121245467013774810 ) ) ;
#15685 = CARTESIAN_POINT ( 'NONE',  ( 14.70402854863798048, 12.78588281574406871, -2.501317291925987174 ) ) ;
#15687 = CYLINDRICAL_SURFACE ( 'NONE', #21726, 3.399999999999999911 ) ;
#15686 = CARTESIAN_POINT ( 'NONE',  ( 2.332967242263025653, -33.01229566874723531, 7.651421919295144036 ) ) ;
#15688 = CARTESIAN_POINT ( 'NONE',  ( 15.37524305911110289, 11.52859259604422526, -2.577749823976538401 ) ) ;
#15689 = CARTESIAN_POINT ( 'NONE',  ( 80.07838786650488316, 65.24465706271045917, -3.189931650267179286 ) ) ;
#15690 = CARTESIAN_POINT ( 'NONE',  ( 78.65108613080987254, 60.71083206350697026, 2.889099817377207557 ) ) ;
#15691 = ORIENTED_EDGE ( 'NONE', *, *, #8969, .T. ) ;
#15692 = CARTESIAN_POINT ( 'NONE',  ( -36.97867591359219119, -24.55319635012989110, 6.700000000000000178 ) ) ;
#15693 = CIRCLE ( 'NONE', #18995, 0.1000000000000028644 ) ;
#15694 = DIRECTION ( 'NONE',  ( -0.000000000000000000, -0.000000000000000000, -1.000000000000000000 ) ) ;
#15695 = CARTESIAN_POINT ( 'NONE',  ( 82.44602376881528016, 63.15227202030956732, 1.728104186157677358 ) ) ;
#15697 = CARTESIAN_POINT ( 'NONE',  ( -1.694080628484398332, -29.37610418048680572, 6.903372536218456368 ) ) ;
#15696 = CARTESIAN_POINT ( 'NONE',  ( 4.299012799853332290, -31.91455539574284472, 6.867199677474202346 ) ) ;
#15698 = CARTESIAN_POINT ( 'NONE',  ( 31.58133870531054654, -3.380569343585269504, 5.164673136779329710 ) ) ;
#15699 = PLANE ( 'NONE',  #20111 ) ;
#15700 = CARTESIAN_POINT ( 'NONE',  ( 15.71680133604306029, -1.673294295210183247, 2.499999999999999556 ) ) ;
#15701 = CARTESIAN_POINT ( 'NONE',  ( 1.530693017522448462, -33.06581389177033259, 6.895394898881670009 ) ) ;
#15702 = CARTESIAN_POINT ( 'NONE',  ( 14.77222818450456643, -4.461908109758233820, -2.511961494517393145 ) ) ;
#15704 = EDGE_CURVE ( 'NONE', #39964, #12335, #7948, .T. ) ;
#15703 = EDGE_LOOP ( 'NONE', ( #25505, #37407, #23473, #26712, #6428 ) ) ;
#15705 = CARTESIAN_POINT ( 'NONE',  ( -0.6341309666911102427, -32.04178038199096079, 6.911401339314954484 ) ) ;
#15706 = CARTESIAN_POINT ( 'NONE',  ( 1.680239621640250647, -25.22888099285786012, 7.013842709614101167 ) ) ;
#15707 = DIRECTION ( 'NONE',  ( -1.000000000000000000, 0.000000000000000000, 0.000000000000000000 ) ) ;
#15708 = CARTESIAN_POINT ( 'NONE',  ( 36.07747683933082783, -1.633048991712910736, -5.715736162573779033 ) ) ;
#15709 = CARTESIAN_POINT ( 'NONE',  ( 66.27376694608931018, 57.73522568913554665, -4.000000000000000000 ) ) ;
#15710 = CARTESIAN_POINT ( 'NONE',  ( 1.731267656427840862, -33.06979397732754933, 7.665454363767879364 ) ) ;
#15711 = CARTESIAN_POINT ( 'NONE',  ( 0.4675928667938681893, -32.83026482617694342, 7.785096263473211486 ) ) ;
#15712 = CARTESIAN_POINT ( 'NONE',  ( 1.749297880632027846, -33.07639249659003866, 7.255881584735164758 ) ) ;
#15713 = CARTESIAN_POINT ( 'NONE',  ( 0.4906401998943609177, -26.28564864924214461, 7.635761828346577573 ) ) ;
#15714 = EDGE_CURVE ( 'NONE', #1980, #25803, #20498, .T. ) ;
#15715 = CARTESIAN_POINT ( 'NONE',  ( -80.92837670882107659, 2.429809908903242555, 12.50000000000000000 ) ) ;
#15716 = CIRCLE ( 'NONE', #1273, 0.1000000000000028644 ) ;
#15717 = CARTESIAN_POINT ( 'NONE',  ( 21.88122113745853170, -13.31826209935299232, 2.500000000000000000 ) ) ;
#15718 = EDGE_CURVE ( 'NONE', #9410, #6472, #943, .T. ) ;
#15719 = LINE ( 'NONE', #27860, #1490 ) ;
#15720 = EDGE_LOOP ( 'NONE', ( #34211, #22456, #31607, #2260, #32129 ) ) ;
#15721 = B_SPLINE_CURVE_WITH_KNOTS ( 'NONE', 3,
 ( #14116, #14319, #11020, #26889, #39430, #37569, #6509, #12664, #31014, #6092 ),
 .UNSPECIFIED., .F., .F.,
 ( 4, 3, 3, 4 ),
 ( 0.0002170292169044741302, 0.0002420761345915971492, 0.0002723302478207005281, 0.0002816811360866754458 ),
 .UNSPECIFIED. ) ;
#15722 = DIRECTION ( 'NONE',  ( 0.000000000000000000, 0.000000000000000000, 1.000000000000000000 ) ) ;
#15723 = CARTESIAN_POINT ( 'NONE',  ( 68.00738522489628224, 58.43930376306189345, -3.995571880668716602 ) ) ;
#15724 = EDGE_CURVE ( 'NONE', #26758, #19353, #20919, .T. ) ;
#15725 = ORIENTED_EDGE ( 'NONE', *, *, #8451, .T. ) ;
#15726 = DIRECTION ( 'NONE',  ( 0.7660444431189770143, 0.6427876096865404731, -0.000000000000000000 ) ) ;
#15727 = EDGE_CURVE ( 'NONE', #16031, #2342, #7323, .T. ) ;
#15728 = VECTOR ( 'NONE', #25115, 1000.000000000000000 ) ;
#15729 = CARTESIAN_POINT ( 'NONE',  ( 1.021324086407808585, -24.55319635012989110, 6.700000000000000178 ) ) ;
#15730 = CARTESIAN_POINT ( 'NONE',  ( 1.223729437044696500, -26.20350854924802064, 7.761597726988849644 ) ) ;
#15731 = CARTESIAN_POINT ( 'NONE',  ( -36.24874870218063450, -26.64985754041175525, 6.800000000000000711 ) ) ;
#15732 = ORIENTED_EDGE ( 'NONE', *, *, #13990, .T. ) ;
#15733 = CARTESIAN_POINT ( 'NONE',  ( 21.82879977636547864, 5.975179493283890864, 3.129347940797799765 ) ) ;
#15734 = FILL_AREA_STYLE_COLOUR ( '', #16868 ) ;
#15735 = ORIENTED_EDGE ( 'NONE', *, *, #17536, .F. ) ;
#15736 = FACE_OUTER_BOUND ( 'NONE', #15869, .T. ) ;
#15737 = ORIENTED_EDGE ( 'NONE', *, *, #22477, .T. ) ;
#15738 = CARTESIAN_POINT ( 'NONE',  ( 79.93872656714209768, 63.00306196921508217, -3.690346394509887773 ) ) ;
#15740 = CARTESIAN_POINT ( 'NONE',  ( -1.672621849119248827, -29.99755011404314331, 6.876076431790006716 ) ) ;
#15739 = CARTESIAN_POINT ( 'NONE',  ( 23.60934223726077974, 0.4472814905813886632, 5.505706761109173009 ) ) ;
#15741 = CARTESIAN_POINT ( 'NONE',  ( 81.76814852625381036, 62.80907675923850775, -2.758880570191353687 ) ) ;
#15742 = CARTESIAN_POINT ( 'NONE',  ( 80.44079772350291080, 62.04115482339161503, 3.140153738741080058 ) ) ;
#15743 = AXIS2_PLACEMENT_3D ( 'NONE', #6292, #19051, #34515 ) ;
#15744 = B_SPLINE_CURVE_WITH_KNOTS ( 'NONE', 3,
 ( #24959, #37493, #38109, #34655, #6427, #16090, #22492, #16287, #31546, #19182 ),
 .UNSPECIFIED., .F., .F.,
 ( 4, 2, 2, 2, 4 ),
 ( 0.5001220714135948819, 0.6250915535601961892, 0.7500610357067973855, 0.8750305178533986927, 1.000000000000000000 ),
 .UNSPECIFIED. ) ;
#15745 = CARTESIAN_POINT ( 'NONE',  ( 82.59411735159427792, 63.56171878218358273, 1.000000000000000000 ) ) ;
#15746 =( BOUNDED_CURVE ( )  B_SPLINE_CURVE ( 3, ( #6077, #21727, #12023, #40648 ),
 .UNSPECIFIED., .F., .T. ) 
 B_SPLINE_CURVE_WITH_KNOTS ( ( 4, 4 ),
 ( 4.748221474220558846, 4.941946782021391371 ),
 .UNSPECIFIED. ) 
 CURVE ( )  GEOMETRIC_REPRESENTATION_ITEM ( )  RATIONAL_B_SPLINE_CURVE ( ( 1.000000000000000000, 0.9968749865767494445, 0.9968749865767494445, 1.000000000000000000 ) ) 
 REPRESENTATION_ITEM ( '' )  );
#15748 = VERTEX_POINT ( 'NONE', #27294 ) ;
#15747 = CARTESIAN_POINT ( 'NONE',  ( 2.875320765573441850, -32.76047449742785034, 7.756377446753164762 ) ) ;
#15749 = DIRECTION ( 'NONE',  ( -1.000000000000000000, -1.165409145176969993E-16, 0.000000000000000000 ) ) ;
#15750 = VERTEX_POINT ( 'NONE', #29982 ) ;
#15751 = CARTESIAN_POINT ( 'NONE',  ( -75.06536287548681230, 8.003295856082973003, 10.46294883374669027 ) ) ;
#15752 = CARTESIAN_POINT ( 'NONE',  ( 37.19747299874393320, -2.841585884120807481, 5.999818732555961098 ) ) ;
#15753 = DIRECTION ( 'NONE',  ( 1.000000000000000000, 0.000000000000000000, 0.000000000000000000 ) ) ;
#15754 = CARTESIAN_POINT ( 'NONE',  ( -81.25386658927445183, 10.50434922290921413, -3.708380354180676797 ) ) ;
#15755 = VECTOR ( 'NONE', #16784, 1000.000000000000227 ) ;
#15756 = CARTESIAN_POINT ( 'NONE',  ( 33.46399183110135311, -3.088807006424163948, -5.429263273580746230 ) ) ;
#15757 = CARTESIAN_POINT ( 'NONE',  ( 30.88430831131045906, 0.7006950504784862366, -4.489146872953734047 ) ) ;
#15758 = CARTESIAN_POINT ( 'NONE',  ( -1.799609906766908463, -29.57443106626083562, 7.625529684960262067 ) ) ;
#15759 = CARTESIAN_POINT ( 'NONE',  ( 17.26693970169123560, 8.754007361387712294, 2.901321561600415322 ) ) ;
#15760 = LINE ( 'NONE', #21948, #35908 ) ;
#15761 = CARTESIAN_POINT ( 'NONE',  ( 29.59347476571312185, -3.810682212465021923, 4.411907216274745913 ) ) ;
#15762 = PRODUCT_RELATED_PRODUCT_CATEGORY ( 'part', '', ( #30290 ) ) ;
#15763 = CARTESIAN_POINT ( 'NONE',  ( -4.448748702180642667, -26.64985754041175525, 6.800000000000000711 ) ) ;
#15764 = B_SPLINE_CURVE_WITH_KNOTS ( 'NONE', 3,
 ( #376, #12912, #9825, #3679, #19703, #13519, #16400, #4268, #23002, #1192 ),
 .UNSPECIFIED., .F., .F.,
 ( 4, 3, 3, 4 ),
 ( 0.000000000000000000, 3.025570593003164513E-05, 6.051145698344131968E-05, 6.468151674593574090E-05 ),
 .UNSPECIFIED. ) ;
#15765 = CARTESIAN_POINT ( 'NONE',  ( 5.067738213087761068, -29.09985929542945371, 7.754798119455333705 ) ) ;
#15766 = CARTESIAN_POINT ( 'NONE',  ( 23.17369588073228925, 0.5344006672354065790, -5.787134729987309711 ) ) ;
#15767 = CARTESIAN_POINT ( 'NONE',  ( 31.79454364665378208, -3.762500967924790274, -4.762111375201251384 ) ) ;
#15768 = CARTESIAN_POINT ( 'NONE',  ( 25.68847553089295488, 2.131605409771632598, -4.143887395686703279 ) ) ;
#15769 = VERTEX_POINT ( 'NONE', #11631 ) ;
#15770 = EDGE_LOOP ( 'NONE', ( #9284, #8482, #32025, #25832, #32754, #10503 ) ) ;
#15771 = CARTESIAN_POINT ( 'NONE',  ( 67.06207392303235792, 57.84849753947618467, 3.994852852620101480 ) ) ;
#15772 = CARTESIAN_POINT ( 'NONE',  ( 36.80687207428664465, -3.101440543725207277, 5.951000583394169041 ) ) ;
#15773 = CIRCLE ( 'NONE', #33539, 10.00000000000000533 ) ;
#15774 = EDGE_CURVE ( 'NONE', #38743, #17308, #29429, .T. ) ;
#15775 = CARTESIAN_POINT ( 'NONE',  ( 11.65737507970504439, -23.60493063168009442, 6.000000000000000000 ) ) ;
#15776 = CARTESIAN_POINT ( 'NONE',  ( 84.71993633203089757, 2.603525311087758531, 3.468835001793752593 ) ) ;
#15777 = EDGE_CURVE ( 'NONE', #153, #15748, #15260, .T. ) ;
#15778 = CARTESIAN_POINT ( 'NONE',  ( 22.06574104993566721, 4.215197008693921887, 2.277743168818826991 ) ) ;
#15779 = LINE ( 'NONE', #34745, #10318 ) ;
#15780 = B_SPLINE_CURVE_WITH_KNOTS ( 'NONE', 3,
 ( #30229, #36808, #11467, #1840, #18058, #33736, #24035, #20961, #36606, #5516, #27336, #39278, #14982, #39896, #30649, #30856, #33951, #11876, #11066 ),
 .UNSPECIFIED., .F., .F.,
 ( 4, 3, 3, 3, 3, 3, 4 ),
 ( 1.563658610346375379E-18, 2.546128104244800347E-05, 5.711050680483675200E-05, 8.113074941675925780E-05, 0.0001053129305727098293, 0.0001360598016347188441, 0.0001612931755702000228 ),
 .UNSPECIFIED. ) ;
#15781 = EDGE_LOOP ( 'NONE', ( #19121, #5980, #39562, #10704, #3745 ) ) ;
#15782 = CARTESIAN_POINT ( 'NONE',  ( 26.39040341943793067, 1.756034159389934235, 4.288588000376896581 ) ) ;
#15783 = SHAPE_REPRESENTATION_RELATIONSHIP ( 'NONE' , 'NONE' ,  #28236, #17103 ) ;
#15784 = DIRECTION ( 'NONE',  ( 1.000000000000000000, 0.000000000000000000, 0.000000000000000000 ) ) ;
#15785 = DIRECTION ( 'NONE',  ( -0.000000000000000000, -0.000000000000000000, -1.000000000000000000 ) ) ;
#15786 = ORIENTED_EDGE ( 'NONE', *, *, #10732, .T. ) ;
#15787 = SURFACE_STYLE_FILL_AREA ( #22786 ) ;
#15788 = CARTESIAN_POINT ( 'NONE',  ( -17.69482985384421880, -29.56993018339339940, -2.500000000000000000 ) ) ;
#15789 = AXIS2_PLACEMENT_3D ( 'NONE', #37907, #6639, #21334 ) ;
#15790 = EDGE_LOOP ( 'NONE', ( #32669, #22324, #37632, #26866 ) ) ;
#15791 = CARTESIAN_POINT ( 'NONE',  ( 80.35827824124267238, 62.85331387716615126, -3.547878946066216788 ) ) ;
#15792 = CARTESIAN_POINT ( 'NONE',  ( 89.09355779190869384, 24.84364830758654108, -8.800414904976364028 ) ) ;
#15793 = CARTESIAN_POINT ( 'NONE',  ( 79.58170130377179419, 64.56493525204571426, 3.531602295408449610 ) ) ;
#15796 = ORIENTED_EDGE ( 'NONE', *, *, #29482, .F. ) ;
#15795 = VERTEX_POINT ( 'NONE', #23026 ) ;
#15794 = PLANE ( 'NONE',  #30920 ) ;
#15797 = CARTESIAN_POINT ( 'NONE',  ( -57.21793255368775988, 30.45183801093173770, 3.625376778041544235 ) ) ;
#15798 = CARTESIAN_POINT ( 'NONE',  ( 1.700390093233090871, -29.56993018339339940, 7.750000000000000888 ) ) ;
#15799 = CARTESIAN_POINT ( 'NONE',  ( -70.92837670882238399, -21.78299143689875095, 10.00000000000113154 ) ) ;
#15800 = DIRECTION ( 'NONE',  ( 0.000000000000000000, 0.000000000000000000, 1.000000000000000000 ) ) ;
#15801 = CARTESIAN_POINT ( 'NONE',  ( 22.61627571821124150, 4.610947867309832304, -3.060900723906414100 ) ) ;
#15802 = ORIENTED_EDGE ( 'NONE', *, *, #30918, .F. ) ;
#15803 = DIRECTION ( 'NONE',  ( -0.000000000000000000, -0.000000000000000000, -1.000000000000000000 ) ) ;
#15804 = CARTESIAN_POINT ( 'NONE',  ( -1.006913970787454371, -31.62676587767679237, 6.876076431790007604 ) ) ;
#15805 = CARTESIAN_POINT ( 'NONE',  ( -72.46964309959683703, 39.11862660440054640, 15.50000000000000000 ) ) ;
#15806 = CARTESIAN_POINT ( 'NONE',  ( -79.97971716480111581, -5.605125688071920464, -6.478939869332222656 ) ) ;
#15807 = LINE ( 'NONE', #12914, #23493 ) ;
#15808 = CARTESIAN_POINT ( 'NONE',  ( 80.70340038347129052, 64.47061299330751183, 3.456914256421387499 ) ) ;
#15809 = CARTESIAN_POINT ( 'NONE',  ( 84.89189963960113516, 2.021164017676272184, 4.676249375175704159 ) ) ;
#15810 = CARTESIAN_POINT ( 'NONE',  ( -22.87867591359218977, -26.64985754041175525, 6.800000000000000711 ) ) ;
#15811 = EDGE_LOOP ( 'NONE', ( #20782, #13707, #33619 ) ) ;
#15812 = FACE_OUTER_BOUND ( 'NONE', #1867, .T. ) ;
#15813 = CARTESIAN_POINT ( 'NONE',  ( 21.59025852387176769, 7.197660357961259692, -2.960420257542255129 ) ) ;
#15814 = ORIENTED_EDGE ( 'NONE', *, *, #11832, .T. ) ;
#15815 = CARTESIAN_POINT ( 'NONE',  ( 3.979067762612290338, -26.91330170476399530, 6.887161170156906209 ) ) ;
#15816 = VECTOR ( 'NONE', #7606, 1000.000000000000000 ) ;
#15817 = CARTESIAN_POINT ( 'NONE',  ( 0.1825688514504806015, 0.5999999999999995337, 3.931742364880953744 ) ) ;
#15818 = FACE_OUTER_BOUND ( 'NONE', #37796, .T. ) ;
#15819 = CARTESIAN_POINT ( 'NONE',  ( -54.79610818216033152, 31.51396769785350926, 1.000000000000000000 ) ) ;
#15820 = ORIENTED_EDGE ( 'NONE', *, *, #1283, .F. ) ;
#15821 = CARTESIAN_POINT ( 'NONE',  ( 35.45270935990075856, -1.916751615000411801, 5.739650741265255540 ) ) ;
#15822 = CARTESIAN_POINT ( 'NONE',  ( 88.11777217834651310, -0.6203394357796320202, -3.242821525125987758 ) ) ;
#15823 = ADVANCED_FACE ( 'NONE', ( #9700 ), #35009, .T. ) ;
#15824 = VERTEX_POINT ( 'NONE', #1408 ) ;
#15826 = CARTESIAN_POINT ( 'NONE',  ( 14.66103313215672088, -4.888004096372116969, 2.500000000000000000 ) ) ;
#15825 = CARTESIAN_POINT ( 'NONE',  ( 79.86111789578113473, 65.11834937465496864, -3.286127602909499235 ) ) ;
#15827 = DIRECTION ( 'NONE',  ( -0.000000000000000000, -0.000000000000000000, 1.000000000000000000 ) ) ;
#15828 = ORIENTED_EDGE ( 'NONE', *, *, #28086, .T. ) ;
#15829 = DIRECTION ( 'NONE',  ( 0.000000000000000000, 0.000000000000000000, 1.000000000000000000 ) ) ;
#15830 = VERTEX_POINT ( 'NONE', #29594 ) ;
#15831 = CARTESIAN_POINT ( 'NONE',  ( -78.05373003007660770, -6.395912128405124797, 7.028357164679021274 ) ) ;
#15833 = ORIENTED_EDGE ( 'NONE', *, *, #19360, .T. ) ;
#15832 = ORIENTED_EDGE ( 'NONE', *, *, #32968, .T. ) ;
#15834 = CARTESIAN_POINT ( 'NONE',  ( 80.05321609864766685, 64.11675358990301277, -3.674973878998263110 ) ) ;
#15835 = CARTESIAN_POINT ( 'NONE',  ( 5.150202707224498688, -30.16051711886163744, 7.750000000000001776 ) ) ;
#15837 = CARTESIAN_POINT ( 'NONE',  ( 21.58863023475808873, 7.202558683720228672, -2.923977588977705544 ) ) ;
#15836 = CARTESIAN_POINT ( 'NONE',  ( 22.27216333610519072, 1.991400367839498475, 5.539784122813447453 ) ) ;
#15838 = ORIENTED_EDGE ( 'NONE', *, *, #7540, .F. ) ;
#15839 = VECTOR ( 'NONE', #17409, 1000.000000000000000 ) ;
#15840 = DIRECTION ( 'NONE',  ( 8.398074759113475787E-17, -1.000000000000000000, 0.000000000000000000 ) ) ;
#15842 = CARTESIAN_POINT ( 'NONE',  ( 85.59084391823684257, 2.218026321225774478, -3.342052983375342734 ) ) ;
#15841 = DIRECTION ( 'NONE',  ( -0.000000000000000000, -0.000000000000000000, 1.000000000000000000 ) ) ;
#15843 = LINE ( 'NONE', #12957, #12602 ) ;
#15844 = CARTESIAN_POINT ( 'NONE',  ( 74.96893927862336682, 59.62365076172310552, 3.485789274173446639 ) ) ;
#15845 = EDGE_CURVE ( 'NONE', #4130, #25231, #10238, .T. ) ;
#15846 = CARTESIAN_POINT ( 'NONE',  ( 22.38852551694001036, 3.992526559945270392, -3.863756592174965920 ) ) ;
#15847 = VERTEX_POINT ( 'NONE', #40074 ) ;
#15848 = CARTESIAN_POINT ( 'NONE',  ( 21.85643539959774273, 11.61750052538138256, -3.706567411524428479 ) ) ;
#15849 = CARTESIAN_POINT ( 'NONE',  ( 3.474430093958352117, -26.56792286420624549, 7.783750581861600182 ) ) ;
#15850 = CARTESIAN_POINT ( 'NONE',  ( 1.057242960569753309, -26.12952878737186424, 7.697032948437507294 ) ) ;
#15851 = CARTESIAN_POINT ( 'NONE',  ( 78.68741431065086545, 66.05648362737333912, 1.057717897339650159 ) ) ;
#15852 = B_SPLINE_CURVE_WITH_KNOTS ( 'NONE', 3,
 ( #9468, #1050, #31724, #29038, #842, #35434, #6404, #28420, #226, #12766 ),
 .UNSPECIFIED., .F., .F.,
 ( 4, 3, 3, 4 ),
 ( 0.0001585009270395733923, 0.0001815657551981825950, 0.0002118214035944112044, 0.0002170292169044733984 ),
 .UNSPECIFIED. ) ;
#15853 = CARTESIAN_POINT ( 'NONE',  ( 87.54465900634191655, 0.02340848060778613626, -4.593250482506632260 ) ) ;
#15854 = ORIENTED_EDGE ( 'NONE', *, *, #8041, .T. ) ;
#15855 = EDGE_CURVE ( 'NONE', #9480, #38999, #30406, .T. ) ;
#15856 = AXIS2_PLACEMENT_3D ( 'NONE', #19162, #16268, #22673 ) ;
#15857 = CARTESIAN_POINT ( 'NONE',  ( 0.4278139304635389939, -32.72279481110962251, 7.759451378593096749 ) ) ;
#15858 = CARTESIAN_POINT ( 'NONE',  ( 14.71571335596265229, -5.054827965358537512, 2.496165019355487846 ) ) ;
#15859 = EDGE_CURVE ( 'NONE', #38743, #31898, #21560, .T. ) ;
#15860 = CARTESIAN_POINT ( 'NONE',  ( 22.92029997850032075, 2.650801711463111499, -3.783665159831076874 ) ) ;
#15861 = DIRECTION ( 'NONE',  ( -0.8660254037844399289, 0.000000000000000000, -0.4999999999999977240 ) ) ;
#15862 =( BOUNDED_CURVE ( )  B_SPLINE_CURVE ( 3, ( #9597, #5908, #6526, #18447 ),
 .UNSPECIFIED., .F., .T. ) 
 B_SPLINE_CURVE_WITH_KNOTS ( ( 4, 4 ),
 ( 4.708531083176466403, 4.712388980384689674 ),
 .UNSPECIFIED. ) 
 CURVE ( )  GEOMETRIC_REPRESENTATION_ITEM ( )  RATIONAL_B_SPLINE_CURVE ( ( 1.000000000000000000, 0.9999987597194787137, 0.9999987597194787137, 1.000000000000000000 ) ) 
 REPRESENTATION_ITEM ( '' )  );
#15863 = LINE ( 'NONE', #35235, #22893 ) ;
#15864 = CARTESIAN_POINT ( 'NONE',  ( -1.254331348952123282, -31.25210608373809507, 7.779495906702013741 ) ) ;
#15865 = AXIS2_PLACEMENT_3D ( 'NONE', #27154, #1863, #18289 ) ;
#15866 = FACE_OUTER_BOUND ( 'NONE', #33528, .T. ) ;
#15867 = ADVANCED_FACE ( 'NONE', ( #18034 ), #14954, .F. ) ;
#15868 = VERTEX_POINT ( 'NONE', #2215 ) ;
#15869 = EDGE_LOOP ( 'NONE', ( #8002, #1866, #23767, #32108 ) ) ;
#15870 = LINE ( 'NONE', #18963, #24471 ) ;
#15871 = VERTEX_POINT ( 'NONE', #14735 ) ;
#15872 = CARTESIAN_POINT ( 'NONE',  ( 66.69105935506532035, 57.95800471661298303, -3.998864354720668146 ) ) ;
#15873 = B_SPLINE_CURVE_WITH_KNOTS ( 'NONE', 3,
 ( #25303, #3099, #15405, #3500, #37838, #34992 ),
 .UNSPECIFIED., .F., .F.,
 ( 4, 2, 4 ),
 ( 0.0006940092137399027188, 0.0008426799592462289306, 0.0009913507047525551424 ),
 .UNSPECIFIED. ) ;
#15874 = ORIENTED_EDGE ( 'NONE', *, *, #2166, .F. ) ;
#15875 = CARTESIAN_POINT ( 'NONE',  ( 87.74107704030866728, -0.1972175777057878776, -3.821749651402456482 ) ) ;
#15876 = CARTESIAN_POINT ( 'NONE',  ( 4.919866799368763033, -30.96019790882458622, 7.387053503561884504 ) ) ;
#15877 = CARTESIAN_POINT ( 'NONE',  ( 4.954788903825591007, -28.58559216437443595, 6.895222827070022653 ) ) ;
#15878 = CARTESIAN_POINT ( 'NONE',  ( 4.995237956833183723, -30.75059844998224179, 7.750000000000001776 ) ) ;
#15879 = FACE_BOUND ( 'NONE', #121, .T. ) ;
#15880 = CARTESIAN_POINT ( 'NONE',  ( 5.551251297819359110, -25.49307895267003587, 6.800000000000000711 ) ) ;
#15881 = ORIENTED_EDGE ( 'NONE', *, *, #907, .F. ) ;
#15882 = CARTESIAN_POINT ( 'NONE',  ( 79.67387220895490429, 66.32735109421591346, -1.189854999565593818 ) ) ;
#15883 = ADVANCED_FACE ( 'NONE', ( #27307 ), #3298, .T. ) ;
#15884 = CARTESIAN_POINT ( 'NONE',  ( 80.05321609864766685, 64.11675358990301277, 3.674973878998264443 ) ) ;
#15885 = CARTESIAN_POINT ( 'NONE',  ( -1.750311609132544799, -28.98456041880788092, 7.742274884880765207 ) ) ;
#15886 = ORIENTED_EDGE ( 'NONE', *, *, #5070, .F. ) ;
#15887 = CARTESIAN_POINT ( 'NONE',  ( 77.06614703306246383, 61.11928327932308491, -3.683100983543596385 ) ) ;
#15889 = FACE_OUTER_BOUND ( 'NONE', #26898, .T. ) ;
#15888 = CARTESIAN_POINT ( 'NONE',  ( 3.914596803305051331, -32.26372945462702546, 7.783750581861601070 ) ) ;
#15890 = CARTESIAN_POINT ( 'NONE',  ( 15.50095926939750512, 11.04212219595600430, -2.625697604742827984 ) ) ;
#15891 = CARTESIAN_POINT ( 'NONE',  ( 81.24880315266030095, 62.88501018724373637, -3.211742283750911753 ) ) ;
#15892 = CARTESIAN_POINT ( 'NONE',  ( 79.32401137462350960, 60.77278567581110025, 2.512892981323315844 ) ) ;
#15893 = ORIENTED_EDGE ( 'NONE', *, *, #34525, .F. ) ;
#15894 = CARTESIAN_POINT ( 'NONE',  ( -32.87867591359218977, -24.55319635012989110, 6.700000000000000178 ) ) ;
#15895 = VECTOR ( 'NONE', #3324, 999.9999999999998863 ) ;
#15896 = CARTESIAN_POINT ( 'NONE',  ( -0.7071601137375974622, -32.11974912022817108, 7.387053503561887169 ) ) ;
#15897 = CARTESIAN_POINT ( 'NONE',  ( 81.16398582655347127, 65.83200543430108098, 2.021051955676537393 ) ) ;
#15899 = CARTESIAN_POINT ( 'NONE',  ( 16.81957507921353212, 9.797913115272733009, 2.499999999999583000 ) ) ;
#15898 = DIRECTION ( 'NONE',  ( -0.000000000000000000, -1.000000000000000000, -0.000000000000000000 ) ) ;
#15900 = CARTESIAN_POINT ( 'NONE',  ( 31.28551011801044268, -2.837290201336624129, -5.599793116354693012 ) ) ;
#15901 = ADVANCED_FACE ( 'NONE', ( #3349 ), #25751, .F. ) ;
#15902 = ADVANCED_FACE ( 'NONE', ( #15866 ), #25548, .F. ) ;
#15903 = DIRECTION ( 'NONE',  ( 0.000000000000000000, 0.000000000000000000, 1.000000000000000000 ) ) ;
#15904 = CARTESIAN_POINT ( 'NONE',  ( -26.34874870218063947, -26.64985754041175525, 6.700000000000000178 ) ) ;
#15905 = CARTESIAN_POINT ( 'NONE',  ( -64.08758708074093136, 35.87095250353098663, 3.952250494627216781 ) ) ;
#15906 = EDGE_CURVE ( 'NONE', #2075, #32186, #34339, .T. ) ;
#15907 = CARTESIAN_POINT ( 'NONE',  ( -60.14275962559869981, 24.84364830758654108, -9.154021781743367114 ) ) ;
#15908 = CARTESIAN_POINT ( 'NONE',  ( 1.677658713487880870, -26.07000400068970336, 7.742274884880762542 ) ) ;
#15909 = CARTESIAN_POINT ( 'NONE',  ( -2.248748702180634940, -25.49307895267003587, 6.800000000000000711 ) ) ;
#15910 = CARTESIAN_POINT ( 'NONE',  ( -62.92837670882106238, 0.7293679304675899644, -6.000000000000000000 ) ) ;
#15911 = CARTESIAN_POINT ( 'NONE',  ( 35.81800206278433052, -3.623520638983628750, -5.691500669916689681 ) ) ;
#15912 = CARTESIAN_POINT ( 'NONE',  ( 4.643350526641022213, -31.46439155470594073, 7.013842709614101167 ) ) ;
#15913 = CARTESIAN_POINT ( 'NONE',  ( 4.358391383913280848, -27.29286427772829526, 7.700536657684219577 ) ) ;
#15914 = CARTESIAN_POINT ( 'NONE',  ( 14.81690770463735696, -6.144096738234146926, -2.518934814212393292 ) ) ;
#15915 = CARTESIAN_POINT ( 'NONE',  ( 3.365638799831626837, -32.53422458008159168, 7.784838882742139532 ) ) ;
#15916 = CARTESIAN_POINT ( 'NONE',  ( -60.75950795826495465, 23.17721540975219696, 12.50000000000000000 ) ) ;
#15917 = CARTESIAN_POINT ( 'NONE',  ( -1.451641158382428243, -28.29529165423184622, 7.757178535559533294 ) ) ;
#15918 = ORIENTED_EDGE ( 'NONE', *, *, #6850, .F. ) ;
#15919 = DIRECTION ( 'NONE',  ( -0.6427876096865430267, 0.7660444431189749048, -0.000000000000000000 ) ) ;
#15920 = CARTESIAN_POINT ( 'NONE',  ( 67.85873555399604129, 57.94375731920307260, -3.976226663256417826 ) ) ;
#15921 = ORIENTED_EDGE ( 'NONE', *, *, #15997, .F. ) ;
#15922 = CARTESIAN_POINT ( 'NONE',  ( -75.45330471031414277, 33.71485196875532608, 15.50000000000000000 ) ) ;
#15923 = CARTESIAN_POINT ( 'NONE',  ( -35.07867591359219972, -26.64985754041175525, 6.800000000000000711 ) ) ;
#15924 = CARTESIAN_POINT ( 'NONE',  ( 22.81051389511380378, 3.483508258214782494, 3.928497976265352687 ) ) ;
#15925 = CARTESIAN_POINT ( 'NONE',  ( 1.189432498329193288, -26.20853045501920064, 7.782034975670475418 ) ) ;
#15926 = VECTOR ( 'NONE', #26952, 999.9999999999998863 ) ;
#15927 = CARTESIAN_POINT ( 'NONE',  ( -71.92837670882106238, -42.87473357531881391, 1.732050807568877637 ) ) ;
#15928 = VERTEX_POINT ( 'NONE', #13793 ) ;
#15929 = CARTESIAN_POINT ( 'NONE',  ( 23.75025100005262146, 3.569496731975624115, 3.159471240185062424 ) ) ;
#15930 = LINE ( 'NONE', #3610, #24766 ) ;
#15931 = CARTESIAN_POINT ( 'NONE',  ( -1.116006548226288642, -31.48728922445879519, 7.505001789837628223 ) ) ;
#15932 = EDGE_LOOP ( 'NONE', ( #13039, #8935, #23030, #2940 ) ) ;
#15933 = CARTESIAN_POINT ( 'NONE',  ( 80.71621671784500052, 61.21110637000719379, -1.935054690158737323 ) ) ;
#15935 = CARTESIAN_POINT ( 'NONE',  ( -1.671431054133620586, -30.00687134634513242, 6.871394612369935651 ) ) ;
#15934 = CARTESIAN_POINT ( 'NONE',  ( 27.36415855513426010, 1.088262529702572090, 4.476529622290722266 ) ) ;
#15936 = CARTESIAN_POINT ( 'NONE',  ( 81.32842084066697907, 61.39880091617934710, -1.358900964588043880 ) ) ;
#15937 = CARTESIAN_POINT ( 'NONE',  ( 79.84618440311783161, 63.29375160576378079, 3.738478073092017073 ) ) ;
#15938 = VERTEX_POINT ( 'NONE', #29444 ) ;
#15939 = EDGE_CURVE ( 'NONE', #29684, #9599, #17158, .T. ) ;
#15940 = EDGE_CURVE ( 'NONE', #18417, #18768, #7830, .T. ) ;
#15941 = CARTESIAN_POINT ( 'NONE',  ( -1.617914377067610765, -30.66822245745067477, 7.771081512783700518 ) ) ;
#15942 = DIRECTION ( 'NONE',  ( -0.000000000000000000, 1.000000000000000000, -0.000000000000000000 ) ) ;
#15943 = B_SPLINE_CURVE_WITH_KNOTS ( 'NONE', 3,
 ( #28209, #15452, #39, #12568, #25137, #3348, #6811, #31936, #37668, #37473, #6407, #15864, #9269, #648, #28423, #18957, #31522, #12770, #7007, #25343, #37880, #22269, #28634, #25749, #34837 ),
 .UNSPECIFIED., .F., .F.,
 ( 4, 3, 3, 3, 3, 3, 3, 3, 4 ),
 ( 6.468151674593483288E-05, 9.076621574722077974E-05, 0.0001210204262067974109, 0.0001512763324577400957, 0.0001815301820994215929, 0.0002117781465860753135, 0.0002420274594459748011, 0.0002722905548971200711, 0.0002816827545175596553 ),
 .UNSPECIFIED. ) ;
#15944 = CARTESIAN_POINT ( 'NONE',  ( 22.32365817596653557, 5.835156701882857178, 3.488260158266504263 ) ) ;
#15945 = LINE ( 'NONE', #3022, #31208 ) ;
#15946 = ORIENTED_EDGE ( 'NONE', *, *, #19911, .T. ) ;
#15947 = CARTESIAN_POINT ( 'NONE',  ( -72.95894646306267362, 3.821331306903040126, 10.95076600805725597 ) ) ;
#15948 = CARTESIAN_POINT ( 'NONE',  ( 23.58291088458457452, 0.3979808540708968390, -5.534409494045887890 ) ) ;
#15949 = B_SPLINE_CURVE_WITH_KNOTS ( 'NONE', 3,
 ( #13690, #20456, #17353, #29932, #13479, #26259, #14280, #26849, #5027, #39390, #7502, #32642, #23752, #8093, #5231, #36522, #27248, #5433, #27656, #27054, #24785, #40211, #12212, #21497, #5641, #20870, #18181, #17972, #30558, #39816, #11383 ),
 .UNSPECIFIED., .F., .F.,
 ( 4, 3, 3, 3, 3, 3, 3, 3, 3, 3, 4 ),
 ( 1.734723475976807094E-18, 2.999644130997484968E-05, 6.002588995694506797E-05, 8.960886084587879282E-05, 0.0001190604700446485644, 0.0001489538463052720186, 0.0001796139255493970147, 0.0002109707048517054523, 0.0002426195318110361155, 0.0002740640997890075935, 0.0002849778069099933643 ),
 .UNSPECIFIED. ) ;
#15950 = ORIENTED_EDGE ( 'NONE', *, *, #35033, .T. ) ;
#15951 = EDGE_CURVE ( 'NONE', #10008, #13769, #11416, .T. ) ;
#15952 = CYLINDRICAL_SURFACE ( 'NONE', #37948, 0.1000000000000028644 ) ;
#15953 = ORIENTED_EDGE ( 'NONE', *, *, #22949, .T. ) ;
#15954 = CARTESIAN_POINT ( 'NONE',  ( -80.96011311534428501, 11.45103779093585139, -0.1896456026672926065 ) ) ;
#15955 = CARTESIAN_POINT ( 'NONE',  ( 32.88854752500713374, -3.408127832021003112, -5.320408019716786896 ) ) ;
#15956 = CARTESIAN_POINT ( 'NONE',  ( 29.48946025503517987, 1.221228239622528911, -4.218580362071199019 ) ) ;
#15957 = CARTESIAN_POINT ( 'NONE',  ( -1.559432610588336932, -30.53614500623134376, 6.979335674598009298 ) ) ;
#15958 = LINE ( 'NONE', #938, #19627 ) ;
#15959 = LINE ( 'NONE', #28521, #18020 ) ;
#15960 = CARTESIAN_POINT ( 'NONE',  ( 5.199376495817195298, -29.65415698750913265, 6.865554069792298542 ) ) ;
#15961 = CARTESIAN_POINT ( 'NONE',  ( 4.327845609297687801, -31.72781746291050098, 7.691066658568941783 ) ) ;
#15962 = CARTESIAN_POINT ( 'NONE',  ( 3.481437286441587897, -32.58288071328335178, 7.695279973900954751 ) ) ;
#15963 = AXIS2_PLACEMENT_3D ( 'NONE', #15466, #27619, #34034 ) ;
#15964 = DIRECTION ( 'NONE',  ( -0.7376613619250370624, -0.6751708784618154491, -0.000000000000000000 ) ) ;
#15965 = CARTESIAN_POINT ( 'NONE',  ( 24.90850614488217474, 1.271311299353267366, -4.572860818722448428 ) ) ;
#15966 = CARTESIAN_POINT ( 'NONE',  ( 30.12331966194739508, -3.814067162060288396, -4.420979061340549521 ) ) ;
#15967 = CARTESIAN_POINT ( 'NONE',  ( -63.08758708074093136, 38.76906266698301806, -4.000000000000000000 ) ) ;
#15968 = ORIENTED_EDGE ( 'NONE', *, *, #35812, .F. ) ;
#15969 = CARTESIAN_POINT ( 'NONE',  ( 67.22540103859083160, 57.85622601175691671, 3.990981480864019826 ) ) ;
#15970 = LINE ( 'NONE', #18439, #33243 ) ;
#15971 = CARTESIAN_POINT ( 'NONE',  ( 85.98972789526511917, 0.6168376674493800671, -5.987237289632960646 ) ) ;
#15972 = ORIENTED_EDGE ( 'NONE', *, *, #2122, .T. ) ;
#15973 = CARTESIAN_POINT ( 'NONE',  ( 24.62487772016506327, 2.984843784653229193, 3.535646819143488884 ) ) ;
#15974 = CARTESIAN_POINT ( 'NONE',  ( 0.000000000000000000, 0.000000000000000000, 0.000000000000000000 ) ) ;
#15975 = DIRECTION ( 'NONE',  ( -0.4582725098355649451, 0.8888117386314224877, 0.000000000000000000 ) ) ;
#15976 = CARTESIAN_POINT ( 'NONE',  ( 0.02590584277092264007, -32.52900140506991988, 7.661510568013096822 ) ) ;
#15977 = ORIENTED_EDGE ( 'NONE', *, *, #6880, .F. ) ;
#15978 = CARTESIAN_POINT ( 'NONE',  ( -38.44874870218063734, -25.49307895267003587, 6.800000000000000711 ) ) ;
#15979 = UNCERTAINTY_MEASURE_WITH_UNIT (LENGTH_MEASURE( 1.000000000000000082E-05 ), #14800, 'distance_accuracy_value', 'NONE');
#15980 = VERTEX_POINT ( 'NONE', #37426 ) ;
#15981 = ORIENTED_EDGE ( 'NONE', *, *, #236, .T. ) ;
#15982 = CARTESIAN_POINT ( 'NONE',  ( 79.40192692649263506, 64.80415203875445229, -3.426353657592664526 ) ) ;
#15983 = CARTESIAN_POINT ( 'NONE',  ( -1.699178655868960552, -29.51577928193538369, 7.785387725071490905 ) ) ;
#15984 = CARTESIAN_POINT ( 'NONE',  ( 81.02333598550073646, 61.30014629029354722, 1.703597047176645507 ) ) ;
#15988 = VERTEX_POINT ( 'NONE', #31073 ) ;
#15987 = ORIENTED_EDGE ( 'NONE', *, *, #31206, .T. ) ;
#15986 = DIRECTION ( 'NONE',  ( 0.000000000000000000, 0.000000000000000000, 1.000000000000000000 ) ) ;
#15985 =( GEOMETRIC_REPRESENTATION_CONTEXT ( 3 ) GLOBAL_UNCERTAINTY_ASSIGNED_CONTEXT ( ( #15979 ) ) GLOBAL_UNIT_ASSIGNED_CONTEXT ( ( #14800, #35844, #16837 ) ) REPRESENTATION_CONTEXT ( 'NONE', 'WORKASPACE' ) );
#15989 = CYLINDRICAL_SURFACE ( 'NONE', #6470, 4.500000000000003553 ) ;
#15990 = CARTESIAN_POINT ( 'NONE',  ( -57.80310541255629886, 30.11675026092115104, 4.211351614731054127 ) ) ;
#15991 = CARTESIAN_POINT ( 'NONE',  ( 4.104433119696450305, -25.16239669867571749, 7.754798119455333705 ) ) ;
#15992 = CARTESIAN_POINT ( 'NONE',  ( 3.419158195859357097, -26.52102280379090971, 7.686927408461904143 ) ) ;
#15993 = DIRECTION ( 'NONE',  ( -1.000000000000000000, 0.000000000000000000, 0.000000000000000000 ) ) ;
#15994 = CARTESIAN_POINT ( 'NONE',  ( 23.42789715074077606, 3.768348859778905435, -3.162797842696227324 ) ) ;
#15995 = VERTEX_POINT ( 'NONE', #3096 ) ;
#15996 = DIRECTION ( 'NONE',  ( -0.3420201433256725987, 0.9396926207859068736, -0.000000000000000000 ) ) ;
#15997 = EDGE_CURVE ( 'NONE', #21048, #24927, #38616, .T. ) ;
#15998 = VERTEX_POINT ( 'NONE', #21801 ) ;
#15999 = EDGE_CURVE ( 'NONE', #2110, #5237, #34483, .T. ) ;
#16000 = CARTESIAN_POINT ( 'NONE',  ( -1.001222095928207656, -31.63424290415207096, 6.871394612369937427 ) ) ;
#16001 = LINE ( 'NONE', #33392, #29382 ) ;
#16002 = CIRCLE ( 'NONE', #11388, 0.1000000000000028644 ) ;
#16003 = AXIS2_PLACEMENT_3D ( 'NONE', #13660, #39158, #2542 ) ;
#16004 = EDGE_CURVE ( 'NONE', #6415, #36097, #9019, .T. ) ;
#16005 = CARTESIAN_POINT ( 'NONE',  ( -79.68099787142058688, -6.645740692013860418, -4.853373096521103491 ) ) ;
#16006 = CARTESIAN_POINT ( 'NONE',  ( -69.08758708074091714, 24.84364830758654108, -8.800414904976364028 ) ) ;
#16007 = FACE_OUTER_BOUND ( 'NONE', #30252, .T. ) ;
#16008 = CARTESIAN_POINT ( 'NONE',  ( 78.77947119303419754, 66.08315628559923027, 1.459100623883111902 ) ) ;
#16009 = CARTESIAN_POINT ( 'NONE',  ( 86.92455237868826146, -1.249784692553891574, -5.093375875629621241 ) ) ;
#16010 = DIRECTION ( 'NONE',  ( 0.000000000000000000, 0.000000000000000000, 1.000000000000000000 ) ) ;
#16011 = ORIENTED_EDGE ( 'NONE', *, *, #22804, .F. ) ;
#16012 = CARTESIAN_POINT ( 'NONE',  ( 2.474049714983522108, -26.25912200567108457, 7.013842709614101167 ) ) ;
#16013 = CARTESIAN_POINT ( 'NONE',  ( 21.58875153664575919, 7.202486658336689551, 2.923638573957438869 ) ) ;
#16014 = AXIS2_PLACEMENT_3D ( 'NONE', #3208, #37733, #27869 ) ;
#16015 = CARTESIAN_POINT ( 'NONE',  ( 1.703254855081945740, -26.16993139028485871, 7.769368695748487319 ) ) ;
#16016 = DIRECTION ( 'NONE',  ( -0.6834397476448871300, 0.000000000000000000, -0.7300069255418698555 ) ) ;
#16017 = DIRECTION ( 'NONE',  ( 0.000000000000000000, 0.000000000000000000, 1.000000000000000000 ) ) ;
#16018 = CARTESIAN_POINT ( 'NONE',  ( -1.003736583562488072, -27.34783681995375915, 7.686927408461907696 ) ) ;
#16019 = CARTESIAN_POINT ( 'NONE',  ( 29.09974842620354707, 0.3540232340485665596, 4.748117540621001886 ) ) ;
#16020 = CARTESIAN_POINT ( 'NONE',  ( 86.42578330747443260, 1.280182770620154953, -5.202446006352976937 ) ) ;
#16021 = ORIENTED_EDGE ( 'NONE', *, *, #23744, .T. ) ;
#16023 = CARTESIAN_POINT ( 'NONE',  ( -7.078675913592194391, -26.64985754041175525, 6.700000000000000178 ) ) ;
#16022 = CARTESIAN_POINT ( 'NONE',  ( 81.14234681338471944, 61.29401378075402818, -1.159471704397073477 ) ) ;
#16024 = CARTESIAN_POINT ( 'NONE',  ( -81.45877670850643426, 35.14220020903839270, 15.50000000000000000 ) ) ;
#16025 = VERTEX_POINT ( 'NONE', #15612 ) ;
#16026 = PLANE ( 'NONE',  #32625 ) ;
#16027 = ORIENTED_EDGE ( 'NONE', *, *, #9729, .T. ) ;
#16028 = DIRECTION ( 'NONE',  ( -0.000000000000000000, -1.000000000000000000, -0.000000000000000000 ) ) ;
#16029 = VECTOR ( 'NONE', #20668, 1000.000000000000000 ) ;
#16030 = AXIS2_PLACEMENT_3D ( 'NONE', #14250, #7476, #23537 ) ;
#16031 = VERTEX_POINT ( 'NONE', #31276 ) ;
#16032 = CARTESIAN_POINT ( 'NONE',  ( 80.50045704793726031, 63.23530725187647050, -3.614403801066807365 ) ) ;
#16033 = CARTESIAN_POINT ( 'NONE',  ( 21.71185578408363881, 6.328645931448866335, 3.192210964217056191 ) ) ;
#16035 = CARTESIAN_POINT ( 'NONE',  ( 5.166400672645620418, -29.08388956939788272, 7.753200566781577763 ) ) ;
#16034 = CARTESIAN_POINT ( 'NONE',  ( 22.81665940757572031, 1.447765978769897766, 5.493635244331218637 ) ) ;
#16037 = ORIENTED_EDGE ( 'NONE', *, *, #4609, .T. ) ;
#16036 = ORIENTED_EDGE ( 'NONE', *, *, #8041, .F. ) ;
#16038 = CARTESIAN_POINT ( 'NONE',  ( 82.07485033897415860, 63.29559580402020913, -2.558871340112543358 ) ) ;
#16039 = VECTOR ( 'NONE', #16080, 1000.000000000000000 ) ;
#16040 = CARTESIAN_POINT ( 'NONE',  ( 4.700406739381271848, -27.96996139531226433, 6.864276522220859711 ) ) ;
#16041 = CARTESIAN_POINT ( 'NONE',  ( 4.554642986601973753, -31.41742589940882269, 6.882085323592685988 ) ) ;
#16042 = CARTESIAN_POINT ( 'NONE',  ( 3.960473582032317363, -32.24238647371081612, 7.635761828346576685 ) ) ;
#16043 = CARTESIAN_POINT ( 'NONE',  ( 5.144846875551112753, -28.94886861257825572, 7.635761828346576685 ) ) ;
#16044 = CARTESIAN_POINT ( 'NONE',  ( 69.67664977695649497, 59.29623187989270150, 3.972683913566358971 ) ) ;
#16045 = ORIENTED_EDGE ( 'NONE', *, *, #7396, .F. ) ;
#16046 = CARTESIAN_POINT ( 'NONE',  ( 22.40063203884636067, 3.836966881894201098, -3.968227663424939600 ) ) ;
#16047 = ORIENTED_EDGE ( 'NONE', *, *, #34232, .T. ) ;
#16048 = ORIENTED_EDGE ( 'NONE', *, *, #18786, .F. ) ;
#16049 = CARTESIAN_POINT ( 'NONE',  ( 21.85643539959779247, -11.31796667593991401, 0.7532527802845886411 ) ) ;
#16051 = ADVANCED_FACE ( 'NONE', ( #20977 ), #33819, .T. ) ;
#16050 = DIRECTION ( 'NONE',  ( -1.000000000000000000, 0.000000000000000000, 0.000000000000000000 ) ) ;
#16052 = CARTESIAN_POINT ( 'NONE',  ( -1.266401589527426763, -27.89466816046029862, 7.257242401810563237 ) ) ;
#16053 = CARTESIAN_POINT ( 'NONE',  ( 78.85932765206025863, 66.13466208585964523, 1.358900964592133054 ) ) ;
#16054 = CARTESIAN_POINT ( 'NONE',  ( 84.92887162652053235, 2.911150016110632510, -2.020846097872043501 ) ) ;
#16055 = VERTEX_POINT ( 'NONE', #11793 ) ;
#16056 = CARTESIAN_POINT ( 'NONE',  ( -81.77906269993763999, -5.605534135063645174, 1.073826742008731294 ) ) ;
#16057 = ORIENTED_EDGE ( 'NONE', *, *, #23460, .T. ) ;
#16058 = CARTESIAN_POINT ( 'NONE',  ( 19.69623932494216945, -2.759629735801022665, 3.280472520642130352 ) ) ;
#16059 = VECTOR ( 'NONE', #21207, 1000.000000000000000 ) ;
#16060 = AXIS2_PLACEMENT_3D ( 'NONE', #31813, #16153, #28717 ) ;
#16061 = CARTESIAN_POINT ( 'NONE',  ( 36.64613206243796384, -2.461592254012722414, -5.925913217033152769 ) ) ;
#16062 = CARTESIAN_POINT ( 'NONE',  ( 5.100338292692609521, -29.55116209899513180, 7.748216051605116839 ) ) ;
#16063 = CARTESIAN_POINT ( 'NONE',  ( 21.79065355195778153, 5.486589654648796888, 3.529560796445746274 ) ) ;
#16064 = CARTESIAN_POINT ( 'NONE',  ( 3.751251297819363728, -25.49307895267003587, 6.700000000000000178 ) ) ;
#16065 = EDGE_LOOP ( 'NONE', ( #21812, #8755, #23082, #9649 ) ) ;
#16066 = FACE_OUTER_BOUND ( 'NONE', #3329, .T. ) ;
#16067 = AXIS2_PLACEMENT_3D ( 'NONE', #35478, #35876, #19813 ) ;
#16068 = FACE_OUTER_BOUND ( 'NONE', #19425, .T. ) ;
#16069 = CARTESIAN_POINT ( 'NONE',  ( 30.68859365574981624, -3.022523058033317778, 4.996095265064695923 ) ) ;
#16070 = ORIENTED_EDGE ( 'NONE', *, *, #21656, .F. ) ;
#16071 = ORIENTED_EDGE ( 'NONE', *, *, #30204, .F. ) ;
#16072 = CARTESIAN_POINT ( 'NONE',  ( 25.73193413792037987, 2.635028621324468467, 3.526313263793730446 ) ) ;
#16073 = CARTESIAN_POINT ( 'NONE',  ( 1.691556635064260350, -33.06436417196861299, 7.773839561854632763 ) ) ;
#16074 = CARTESIAN_POINT ( 'NONE',  ( 1.754226040725147096, -26.17035530198076643, 6.889465824494257262 ) ) ;
#16075 = ORIENTED_EDGE ( 'NONE', *, *, #2258, .F. ) ;
#16076 = EDGE_CURVE ( 'NONE', #4319, #17865, #28527, .T. ) ;
#16077 = CARTESIAN_POINT ( 'NONE',  ( 66.27376694609004915, 57.73522568913436004, -4.000000000000000000 ) ) ;
#16078 = CARTESIAN_POINT ( 'NONE',  ( -0.5138166168388553778, -26.87613091215975913, 7.783750581861601070 ) ) ;
#16079 = VERTEX_POINT ( 'NONE', #8101 ) ;
#16080 = DIRECTION ( 'NONE',  ( -0.9396926207859104263, 0.3420201433256631063, -0.000000000000000000 ) ) ;
#16081 = CARTESIAN_POINT ( 'NONE',  ( 4.945111664236113924, -28.55411654084933204, 6.871394612369935651 ) ) ;
#16082 = LINE ( 'NONE', #19380, #3048 ) ;
#16083 = CARTESIAN_POINT ( 'NONE',  ( 3.804543977483544559, -32.36680995045413312, 6.921725064902950031 ) ) ;
#16084 = VERTEX_POINT ( 'NONE', #37135 ) ;
#16085 = CARTESIAN_POINT ( 'NONE',  ( 81.46991160412488853, 61.46693516840311133, -1.070820504727074685 ) ) ;
#16086 = EDGE_CURVE ( 'NONE', #19840, #22023, #11390, .T. ) ;
#16088 = AXIS2_PLACEMENT_3D ( 'NONE', #29726, #937, #20451 ) ;
#16087 = CARTESIAN_POINT ( 'NONE',  ( 80.99344733541434493, 61.93321701578161509, 2.778975589575234384 ) ) ;
#16089 = CIRCLE ( 'NONE', #29260, 9.386006772603931125 ) ;
#16090 = CARTESIAN_POINT ( 'NONE',  ( -70.12981335532620619, -21.39869996748758396, 3.947339383427191262 ) ) ;
#16091 = ORIENTED_EDGE ( 'NONE', *, *, #8585, .F. ) ;
#16092 = CARTESIAN_POINT ( 'NONE',  ( 75.57967633106541427, 61.33476069914100748, -3.901127667181007119 ) ) ;
#16094 = LINE ( 'NONE', #25569, #32892 ) ;
#16093 = CARTESIAN_POINT ( 'NONE',  ( -71.31920275879095072, -45.66549222223517290, 5.988038532114558166 ) ) ;
#16095 = CARTESIAN_POINT ( 'NONE',  ( 19.02761876096537463, 7.101601804412763563, -3.176118110984106568 ) ) ;
#16096 = CARTESIAN_POINT ( 'NONE',  ( 78.94073822560471854, 66.07870154842751731, -1.754135932968032163 ) ) ;
#16097 = CARTESIAN_POINT ( 'NONE',  ( 76.19461364182981811, 62.94386820200828225, 3.683100983535307904 ) ) ;
#16098 = EDGE_LOOP ( 'NONE', ( #22875, #30119, #32630, #15833 ) ) ;
#16099 = AXIS2_PLACEMENT_3D ( 'NONE', #23175, #757, #20077 ) ;
#16100 = DIRECTION ( 'NONE',  ( 0.8660254037844380415, 0.5000000000000009992, -0.000000000000000000 ) ) ;
#16102 = EDGE_CURVE ( 'NONE', #19329, #35983, #17985, .T. ) ;
#16101 = DIRECTION ( 'NONE',  ( 1.000000000000000000, 0.000000000000000000, 0.000000000000000000 ) ) ;
#16103 = CARTESIAN_POINT ( 'NONE',  ( 78.68995612299298159, 66.05828935306207939, 1.022614849746397159 ) ) ;
#16104 =( BOUNDED_CURVE ( )  B_SPLINE_CURVE ( 3, ( #26706, #39240, #39651, #33511 ),
 .UNSPECIFIED., .F., .F. ) 
 B_SPLINE_CURVE_WITH_KNOTS ( ( 4, 4 ),
 ( 1.381924640371167579, 1.574767692156076038 ),
 .UNSPECIFIED. ) 
 CURVE ( )  GEOMETRIC_REPRESENTATION_ITEM ( )  RATIONAL_B_SPLINE_CURVE ( ( 1.000000000000000000, 0.9969033633783032089, 0.9969033633783032089, 1.000000000000000000 ) ) 
 REPRESENTATION_ITEM ( '' )  );
#16106 = DIRECTION ( 'NONE',  ( -0.000000000000000000, -1.000000000000000000, -0.000000000000000000 ) ) ;
#16105 = CARTESIAN_POINT ( 'NONE',  ( -0.2133591888346773602, -32.50038470195961082, 6.951256099901593544 ) ) ;
#16107 = CARTESIAN_POINT ( 'NONE',  ( 30.07020345058763766, -4.232275913155626235, -2.900971327107725983 ) ) ;
#16108 = CARTESIAN_POINT ( 'NONE',  ( -59.87552183813137674, 24.84364830758654108, 9.800414904976365804 ) ) ;
#16109 = CARTESIAN_POINT ( 'NONE',  ( -1.265720463714046895, -27.71192368072266277, 7.750000000000000888 ) ) ;
#16110 = CARTESIAN_POINT ( 'NONE',  ( 4.707770054155486328, -31.33846319669150660, 7.781480525794719938 ) ) ;
#16111 = CARTESIAN_POINT ( 'NONE',  ( -66.99872204295122913, 28.48507918597134037, -46.17089178453873188 ) ) ;
#16112 = LINE ( 'NONE', #22713, #17685 ) ;
#16113 = CARTESIAN_POINT ( 'NONE',  ( 33.43921609458320177, -3.587388448609353020, -5.336552248008303856 ) ) ;
#16114 = CARTESIAN_POINT ( 'NONE',  ( 32.91483545724720017, -0.5485586877609884837, -5.320376416278755904 ) ) ;
#16115 = CARTESIAN_POINT ( 'NONE',  ( -70.92837670882107659, -36.87473357531881391, 0.000000000000000000 ) ) ;
#16116 = CARTESIAN_POINT ( 'NONE',  ( -0.8817401311824972776, -31.78185462018515750, 7.712764235869105534 ) ) ;
#16117 = CARTESIAN_POINT ( 'NONE',  ( 1.720554196122513257, -32.96987691609166404, 7.643333865083956624 ) ) ;
#16118 = DIRECTION ( 'NONE',  ( -0.5751513419797880111, -0.4826092789263689564, 0.6605219282605377940 ) ) ;
#16119 = EDGE_CURVE ( 'NONE', #33685, #13364, #39608, .T. ) ;
#16120 = CIRCLE ( 'NONE', #15459, 6.000000000000002665 ) ;
#16121 = CARTESIAN_POINT ( 'NONE',  ( 22.22081959608184931, -10.19411496085875157, 2.499999999999999556 ) ) ;
#16122 = AXIS2_PLACEMENT_3D ( 'NONE', #20127, #16827, #20516 ) ;
#16123 = DIRECTION ( 'NONE',  ( -0.000000000000000000, -0.000000000000000000, -1.000000000000000000 ) ) ;
#16125 = ORIENTED_EDGE ( 'NONE', *, *, #28206, .T. ) ;
#16124 = AXIS2_PLACEMENT_3D ( 'NONE', #27900, #22159, #3445 ) ;
#16126 = CARTESIAN_POINT ( 'NONE',  ( 2.884763386751913572, -26.27641232226080703, 7.635761828346579350 ) ) ;
#16127 = CARTESIAN_POINT ( 'NONE',  ( 68.66337269546751543, 58.46565884629779930, -3.990501929453247332 ) ) ;
#16128 = TOROIDAL_SURFACE ( 'NONE', #33840, 6.999999999999986677, 1.000000000000000000 ) ;
#16129 = ORIENTED_EDGE ( 'NONE', *, *, #7442, .F. ) ;
#16130 = LINE ( 'NONE', #37536, #21295 ) ;
#16131 = CARTESIAN_POINT ( 'NONE',  ( 30.88699261567396093, -3.468694606085327425, 4.911399322420932911 ) ) ;
#16132 = CARTESIAN_POINT ( 'NONE',  ( 22.78168706071813077, 3.725697157195321019, 3.755607005719465263 ) ) ;
#16133 = CARTESIAN_POINT ( 'NONE',  ( -1.431314549547642256, -28.24613789213861281, 6.882085323592685100 ) ) ;
#16134 = EDGE_CURVE ( 'NONE', #6556, #27970, #10750, .T. ) ;
#16135 = EDGE_CURVE ( 'NONE', #169, #25414, #27666, .T. ) ;
#16136 = CARTESIAN_POINT ( 'NONE',  ( 3.608934358494904515, -26.63608308657048340, 6.921725064902951807 ) ) ;
#16137 = CARTESIAN_POINT ( 'NONE',  ( 1.123253381486050140, -26.11784194350818211, 6.894806418505347700 ) ) ;
#16138 = ORIENTED_EDGE ( 'NONE', *, *, #7615, .F. ) ;
#16139 = ADVANCED_FACE ( 'NONE', ( #40221 ), #12004, .T. ) ;
#16140 = CARTESIAN_POINT ( 'NONE',  ( -81.07947155388369254, 30.81399289130168384, -46.17089178453873188 ) ) ;
#16141 = CARTESIAN_POINT ( 'NONE',  ( 81.23686708412715518, 61.78859655676697571, 2.419967184825709161 ) ) ;
#16142 = CARTESIAN_POINT ( 'NONE',  ( 0.8902999215273917910, -32.98191326122828571, 7.387053503561886281 ) ) ;
#16143 = EDGE_LOOP ( 'NONE', ( #17978, #31862, #17755, #35006 ) ) ;
#16144 = CARTESIAN_POINT ( 'NONE',  ( 78.20000946334697289, 65.71092203236408125, -1.748505333477076817 ) ) ;
#16146 = CARTESIAN_POINT ( 'NONE',  ( -1.658561354524213716, -30.09671981084580850, 6.880147297696979969 ) ) ;
#16145 = CARTESIAN_POINT ( 'NONE',  ( 22.64667696449940237, 0.3053113478315905849, 6.452936397408012503 ) ) ;
#16147 = CARTESIAN_POINT ( 'NONE',  ( 81.46069228693599484, 61.55470069442471015, -1.644402879615779689 ) ) ;
#16148 = CARTESIAN_POINT ( 'NONE',  ( 80.23310653198076636, 61.53645999506316144, 2.845586111146968467 ) ) ;
#16149 = VECTOR ( 'NONE', #194, 1000.000000000000000 ) ;
#16150 = ADVANCED_FACE ( 'NONE', ( #36531 ), #5238, .F. ) ;
#16151 = CARTESIAN_POINT ( 'NONE',  ( -63.63077514377983590, 43.97264056304742752, 2.477143415600858933 ) ) ;
#16152 = CARTESIAN_POINT ( 'NONE',  ( 22.79131883835711037, -5.922936844141047708, 5.170149038749508819 ) ) ;
#16153 = DIRECTION ( 'NONE',  ( 0.000000000000000000, 0.000000000000000000, 1.000000000000000000 ) ) ;
#16154 = VERTEX_POINT ( 'NONE', #14690 ) ;
#16155 = CARTESIAN_POINT ( 'NONE',  ( -74.32232877538925209, 7.099204298189413009, 10.69770487804055215 ) ) ;
#16156 = CARTESIAN_POINT ( 'NONE',  ( 23.04471710095623038, 0.3232145568372689626, -5.972274008649366195 ) ) ;
#16157 = ORIENTED_EDGE ( 'NONE', *, *, #29614, .F. ) ;
#16158 = AXIS2_PLACEMENT_3D ( 'NONE', #12676, #9180, #22173 ) ;
#16159 = CARTESIAN_POINT ( 'NONE',  ( 0.6211818808881177656, -26.24046902339169307, 7.751599049952197618 ) ) ;
#16160 = CARTESIAN_POINT ( 'NONE',  ( -1.019135405902276581, -31.75353427597946165, 7.782861076432733505 ) ) ;
#16161 = CARTESIAN_POINT ( 'NONE',  ( 28.41783740563939631, -4.024351259184133944, -4.165758313493220122 ) ) ;
#16162 = CARTESIAN_POINT ( 'NONE',  ( 36.44474408801026755, -1.733425704062592221, -5.731406469632323031 ) ) ;
#16163 = CARTESIAN_POINT ( 'NONE',  ( 3.757225787516494275, -32.27723424741392932, 6.876076431790008492 ) ) ;
#16164 = CARTESIAN_POINT ( 'NONE',  ( 16.22309343533386539, 10.39346123325232085, 2.693864712708880393 ) ) ;
#16165 = CARTESIAN_POINT ( 'NONE',  ( -36.34874870218064302, -26.64985754041175525, 6.800000000000000711 ) ) ;
#16166 = DIRECTION ( 'NONE',  ( 0.000000000000000000, 0.000000000000000000, 1.000000000000000000 ) ) ;
#16167 = CARTESIAN_POINT ( 'NONE',  ( -70.92837670882107659, 26.72470171467712063, -6.406751979251626317 ) ) ;
#16168 = CARTESIAN_POINT ( 'NONE',  ( -32.34874870218063592, -26.64985754041175525, 6.700000000000000178 ) ) ;
#16169 = CARTESIAN_POINT ( 'NONE',  ( 34.59489306780999129, -0.7688126975909262972, -5.270100711184057651 ) ) ;
#16170 = CARTESIAN_POINT ( 'NONE',  ( -36.24874870218063450, -25.49307895267003587, 6.700000000000000178 ) ) ;
#16171 = EDGE_LOOP ( 'NONE', ( #14647, #39765, #29111, #25307 ) ) ;
#16172 = CARTESIAN_POINT ( 'NONE',  ( 66.71461092208421917, 57.89240490252945648, 3.999756211082519552 ) ) ;
#16173 = EDGE_CURVE ( 'NONE', #15412, #40099, #6734, .T. ) ;
#16174 = VECTOR ( 'NONE', #37770, 1000.000000000000000 ) ;
#16175 = VECTOR ( 'NONE', #36045, 1000.000000000000000 ) ;
#16177 = EDGE_CURVE ( 'NONE', #26349, #7986, #12834, .T. ) ;
#16176 = CARTESIAN_POINT ( 'NONE',  ( 84.35358620389857265, 3.041238144818853684, 1.123552906098365112 ) ) ;
#16178 = CARTESIAN_POINT ( 'NONE',  ( 1.646239191775039412, -25.86893018339335981, 7.695279973900954751 ) ) ;
#16179 = ORIENTED_EDGE ( 'NONE', *, *, #24487, .T. ) ;
#16180 = CARTESIAN_POINT ( 'NONE',  ( 24.86489394813727216, 2.560632942376066534, 3.960803519163274444 ) ) ;
#16181 = CARTESIAN_POINT ( 'NONE',  ( 0.000000000000000000, 0.000000000000000000, 0.000000000000000000 ) ) ;
#16182 = VECTOR ( 'NONE', #36109, 1000.000000000000114 ) ;
#16183 = DIRECTION ( 'NONE',  ( 0.000000000000000000, 0.000000000000000000, 1.000000000000000000 ) ) ;
#16184 = ADVANCED_FACE ( 'NONE', ( #13239 ), #34291, .F. ) ;
#16185 = DIRECTION ( 'NONE',  ( -1.000000000000000000, -0.000000000000000000, -0.000000000000000000 ) ) ;
#16186 = ORIENTED_EDGE ( 'NONE', *, *, #10627, .F. ) ;
#16187 = CARTESIAN_POINT ( 'NONE',  ( 4.041943119853272037, -26.96886997397920638, 7.754798119455333705 ) ) ;
#16188 = ORIENTED_EDGE ( 'NONE', *, *, #38248, .F. ) ;
#16189 = CARTESIAN_POINT ( 'NONE',  ( 79.12326768591945836, 65.24646460380061797, -3.052025427726081652 ) ) ;
#16190 = DIRECTION ( 'NONE',  ( 1.000000000000000000, 0.000000000000000000, 0.000000000000000000 ) ) ;
#16191 = ADVANCED_FACE ( 'NONE', ( #34696 ), #25404, .T. ) ;
#16192 = CARTESIAN_POINT ( 'NONE',  ( 78.59417545055856635, 65.93066236947775849, 1.724274471760826488 ) ) ;
#16195 = ORIENTED_EDGE ( 'NONE', *, *, #36863, .F. ) ;
#16194 = VERTEX_POINT ( 'NONE', #9135 ) ;
#16193 = CARTESIAN_POINT ( 'NONE',  ( -11.07867591359219794, -24.55319635012989110, 6.800000000000000711 ) ) ;
#16196 = FACE_OUTER_BOUND ( 'NONE', #30269, .T. ) ;
#16197 = LINE ( 'NONE', #15991, #15755 ) ;
#16198 = FACE_OUTER_BOUND ( 'NONE', #19479, .T. ) ;
#16199 = CARTESIAN_POINT ( 'NONE',  ( 21.85643539959774273, 11.82890447862143546, -1.931159885854170311 ) ) ;
#16200 = CARTESIAN_POINT ( 'NONE',  ( 23.42914634548708364, 3.774006297069265159, -3.150363682666455389 ) ) ;
#16201 = ORIENTED_EDGE ( 'NONE', *, *, #7066, .T. ) ;
#16202 = EDGE_LOOP ( 'NONE', ( #34144, #31191, #1439, #24185 ) ) ;
#16203 = CARTESIAN_POINT ( 'NONE',  ( -1.758549627899453682, -30.10456852828691865, 6.867280401193707640 ) ) ;
#16204 = DIRECTION ( 'NONE',  ( -0.000000000000000000, -0.000000000000000000, -1.000000000000000000 ) ) ;
#16205 = FACE_OUTER_BOUND ( 'NONE', #31585, .T. ) ;
#16206 = DIRECTION ( 'NONE',  ( 1.000000000000000000, 7.232507224765808510E-18, 0.000000000000000000 ) ) ;
#16207 = CARTESIAN_POINT ( 'NONE',  ( 79.58096101840206416, 65.58481148403340910, 2.850064543546717566 ) ) ;
#16208 = DIRECTION ( 'NONE',  ( 1.000000000000000000, 0.000000000000000000, 0.000000000000000000 ) ) ;
#16209 = CARTESIAN_POINT ( 'NONE',  ( 21.63116867190874260, 6.951708668987069295, -2.990534277344490732 ) ) ;
#16210 = CARTESIAN_POINT ( 'NONE',  ( -1.577145252566735767, -30.79784596747070680, 7.720710062488887360 ) ) ;
#16211 = CARTESIAN_POINT ( 'NONE',  ( 25.01091298175674993, 3.329590532569525418, 1.936828115940083084 ) ) ;
#16212 = MECHANICAL_DESIGN_GEOMETRIC_PRESENTATION_REPRESENTATION (  '', ( #39862 ), #3750 ) ;
#16213 = VECTOR ( 'NONE', #30275, 1000.000000000000000 ) ;
#16214 = ADVANCED_FACE ( 'NONE', ( #25601 ), #18808, .F. ) ;
#16215 = CARTESIAN_POINT ( 'NONE',  ( -22.44874870218064089, -26.64985754041175525, 6.800000000000000711 ) ) ;
#16216 = CARTESIAN_POINT ( 'NONE',  ( 6.064999797981664997, -27.09154098917056785, 7.695279973900954751 ) ) ;
#16217 = CARTESIAN_POINT ( 'NONE',  ( 4.693152714189181118, -27.95640678116755851, 7.774064877406527074 ) ) ;
#16218 = CYLINDRICAL_SURFACE ( 'NONE', #38496, 21.28220113893567245 ) ;
#16219 = ORIENTED_EDGE ( 'NONE', *, *, #1916, .F. ) ;
#16220 = CARTESIAN_POINT ( 'NONE',  ( 36.42101398311888261, -3.115835042429591972, 5.890778096254243756 ) ) ;
#16221 = CARTESIAN_POINT ( 'NONE',  ( 86.07545474579461597, 1.673688438695506431, -4.651254279175787154 ) ) ;
#16222 = ORIENTED_EDGE ( 'NONE', *, *, #11233, .F. ) ;
#16224 = CARTESIAN_POINT ( 'NONE',  ( 21.74105249613594992, 4.237279478211291028, 2.792868651270881131 ) ) ;
#16223 = CARTESIAN_POINT ( 'NONE',  ( 81.02539575022784391, 62.78269734341446195, -3.300462285847916899 ) ) ;
#16225 = DIRECTION ( 'NONE',  ( 0.000000000000000000, 0.000000000000000000, 1.000000000000000000 ) ) ;
#16226 = LINE ( 'NONE', #31281, #2074 ) ;
#16227 = ORIENTED_EDGE ( 'NONE', *, *, #22931, .T. ) ;
#16228 = LINE ( 'NONE', #25506, #16149 ) ;
#16229 = EDGE_CURVE ( 'NONE', #21394, #20712, #24582, .T. ) ;
#16230 = ORIENTED_EDGE ( 'NONE', *, *, #11604, .F. ) ;
#16231 = CARTESIAN_POINT ( 'NONE',  ( -79.77824834640263418, -6.648693431677500598, 4.674947531023576630 ) ) ;
#16232 = AXIS2_PLACEMENT_3D ( 'NONE', #33923, #21558, #6313 ) ;
#16233 = EDGE_CURVE ( 'NONE', #17469, #463, #3002, .T. ) ;
#16235 = ORIENTED_EDGE ( 'NONE', *, *, #16721, .F. ) ;
#16234 = ORIENTED_EDGE ( 'NONE', *, *, #32592, .T. ) ;
#16236 = CARTESIAN_POINT ( 'NONE',  ( 81.04163241827636455, 61.94641952267326701, -2.758686562281577270 ) ) ;
#16237 = AXIS2_PLACEMENT_3D ( 'NONE', #21806, #15827, #15619 ) ;
#16238 = CARTESIAN_POINT ( 'NONE',  ( 22.35184836610467229, 4.907951308887271935, 3.033114723143640390 ) ) ;
#16239 = CIRCLE ( 'NONE', #3112, 0.1000000000000028644 ) ;
#16240 = CARTESIAN_POINT ( 'NONE',  ( 24.81935351061392936, 2.321748820690546111, 4.088153248315227195 ) ) ;
#16241 = VERTEX_POINT ( 'NONE', #31586 ) ;
#16242 = CIRCLE ( 'NONE', #18197, 3.499999999999999556 ) ;
#16243 = CARTESIAN_POINT ( 'NONE',  ( 4.690406051945708477, -27.95131943120609463, 6.866852738645442322 ) ) ;
#16245 = CARTESIAN_POINT ( 'NONE',  ( -75.45330471031414277, 33.71485196875532608, 21.52833696633422988 ) ) ;
#16244 = CARTESIAN_POINT ( 'NONE',  ( 4.586012032047667830, -31.36803641669331455, 6.864276522220859711 ) ) ;
#16246 = CARTESIAN_POINT ( 'NONE',  ( -2.639489883291917138, -27.04870784343005141, 7.635761828346577573 ) ) ;
#16247 = CARTESIAN_POINT ( 'NONE',  ( 69.70139497306261944, 59.23354404394888917, 3.977789803233246158 ) ) ;
#16248 = ORIENTED_EDGE ( 'NONE', *, *, #6318, .T. ) ;
#16249 = CARTESIAN_POINT ( 'NONE',  ( 23.88318583406893936, 3.159564200708308235, -3.647954507178626127 ) ) ;
#16250 = ORIENTED_EDGE ( 'NONE', *, *, #6059, .F. ) ;
#16251 = VERTEX_POINT ( 'NONE', #99 ) ;
#16252 = CARTESIAN_POINT ( 'NONE',  ( 21.85643539959774273, -8.640774161329524361, 8.772446831725494221 ) ) ;
#16253 = CARTESIAN_POINT ( 'NONE',  ( 21.87751110071505778, 4.134169920263886411, 2.121951800777925445 ) ) ;
#16254 = DIRECTION ( 'NONE',  ( 0.000000000000000000, 0.000000000000000000, 1.000000000000000000 ) ) ;
#16255 = CARTESIAN_POINT ( 'NONE',  ( 80.14223387229885986, 65.61881967978085584, 2.852119850618825669 ) ) ;
#16256 = ORIENTED_EDGE ( 'NONE', *, *, #30787, .F. ) ;
#16257 = CARTESIAN_POINT ( 'NONE',  ( 14.72830186850272938, 12.61371249416686702, 2.505105730543339515 ) ) ;
#16258 = CARTESIAN_POINT ( 'NONE',  ( 16.21738897043104899, -3.323621905045633262, 2.737513786506908353 ) ) ;
#16259 = CARTESIAN_POINT ( 'NONE',  ( 36.76006098925728338, -2.519186585992552185, 5.943694581444969316 ) ) ;
#16260 = CARTESIAN_POINT ( 'NONE',  ( 33.25546742218144658, -3.823472235995165835, 5.051159332570485105 ) ) ;
#16261 = CARTESIAN_POINT ( 'NONE',  ( 36.44714645434917344, -2.354196673243254434, -5.894856700406053029 ) ) ;
#16262 = CARTESIAN_POINT ( 'NONE',  ( 0.5651823463118889057, -32.77481760284047141, 7.661510568013097711 ) ) ;
#16263 = DIRECTION ( 'NONE',  ( 0.1736481776669273613, 0.9848077530122086864, -0.000000000000000000 ) ) ;
#16264 = VECTOR ( 'NONE', #34646, 1000.000000000000000 ) ;
#16265 = DIRECTION ( 'NONE',  ( 1.000000000000000000, 0.000000000000000000, 0.000000000000000000 ) ) ;
#16266 = VECTOR ( 'NONE', #7698, 1000.000000000000000 ) ;
#16267 = AXIS2_PLACEMENT_3D ( 'NONE', #17172, #33045, #26266 ) ;
#16268 = DIRECTION ( 'NONE',  ( -0.000000000000000000, -0.000000000000000000, 1.000000000000000000 ) ) ;
#16269 = CARTESIAN_POINT ( 'NONE',  ( 28.79959244091942594, -3.877818713555981400, 4.349622696032581004 ) ) ;
#16270 = ORIENTED_EDGE ( 'NONE', *, *, #2864, .F. ) ;
#16271 = ORIENTED_EDGE ( 'NONE', *, *, #26830, .T. ) ;
#16272 = CARTESIAN_POINT ( 'NONE',  ( 33.45666195923615049, -3.831709260703673792, 5.091247116679021190 ) ) ;
#16273 = CARTESIAN_POINT ( 'NONE',  ( -44.23414840393349579, -30.38627270959228710, 6.800000000000000711 ) ) ;
#16274 = CARTESIAN_POINT ( 'NONE',  ( 66.55613647995218685, 57.87265654107390844, -3.999745625243888547 ) ) ;
#16275 = EDGE_CURVE ( 'NONE', #9053, #9101, #16130, .T. ) ;
#16276 = EDGE_LOOP ( 'NONE', ( #16865, #31950 ) ) ;
#16277 = EDGE_CURVE ( 'NONE', #12271, #12509, #6263, .T. ) ;
#16278 = CARTESIAN_POINT ( 'NONE',  ( -61.24591834330252027, 3.729367930467589076, 2.500000000000000000 ) ) ;
#16279 = B_SPLINE_CURVE_WITH_KNOTS ( 'NONE', 3,
 ( #29427, #1038, #38275, #13968 ),
 .UNSPECIFIED., .F., .F.,
 ( 4, 4 ),
 ( 0.000000000000000000, 6.391136169993976977E-06 ),
 .UNSPECIFIED. ) ;
#16280 = EDGE_LOOP ( 'NONE', ( #26381, #35167 ) ) ;
#16281 = DIRECTION ( 'NONE',  ( -0.000000000000000000, -0.000000000000000000, 1.000000000000000000 ) ) ;
#16282 = CARTESIAN_POINT ( 'NONE',  ( -22.87867591359218977, -26.64985754041175525, 6.700000000000000178 ) ) ;
#16283 = VERTEX_POINT ( 'NONE', #9751 ) ;
#16284 = CARTESIAN_POINT ( 'NONE',  ( 23.71002378246611997, 3.505939628316281809, 3.324835373315420561 ) ) ;
#16285 = CARTESIAN_POINT ( 'NONE',  ( 81.92984576605157088, 61.94483778347744618, -1.306649493517271221 ) ) ;
#16286 = VECTOR ( 'NONE', #24241, 1000.000000000000114 ) ;
#16287 = CARTESIAN_POINT ( 'NONE',  ( -69.95498688392430608, -21.04617888798872727, 3.920732911918689556 ) ) ;
#16288 = VERTEX_POINT ( 'NONE', #3411 ) ;
#16289 = VERTEX_POINT ( 'NONE', #21911 ) ;
#16290 = CARTESIAN_POINT ( 'NONE',  ( 76.19819836466999163, 59.97076997751577210, -3.322260703561257245 ) ) ;
#16292 = DIRECTION ( 'NONE',  ( 0.000000000000000000, 0.000000000000000000, 1.000000000000000000 ) ) ;
#16291 = CARTESIAN_POINT ( 'NONE',  ( -70.92837670882107659, 15.04836564048558500, -6.406751979251626317 ) ) ;
#16293 = CARTESIAN_POINT ( 'NONE',  ( 14.83458786958485121, 12.32104755890018843, -2.521694231548856191 ) ) ;
#16294 = CARTESIAN_POINT ( 'NONE',  ( 76.31287196683638285, 61.24236878174156828, 3.825872951957600243 ) ) ;
#16295 = VECTOR ( 'NONE', #11103, 1000.000000000000000 ) ;
#16296 = ORIENTED_EDGE ( 'NONE', *, *, #9414, .T. ) ;
#16297 = ORIENTED_EDGE ( 'NONE', *, *, #29780, .F. ) ;
#16298 = CARTESIAN_POINT ( 'NONE',  ( 14.61802081865033820, 0.000000000000000000, 2.500000000000000000 ) ) ;
#16299 = CARTESIAN_POINT ( 'NONE',  ( 1.785524755912862194, -26.08120387293316256, 7.780491323090171996 ) ) ;
#16300 = LINE ( 'NONE', #38317, #38108 ) ;
#16301 = CARTESIAN_POINT ( 'NONE',  ( 79.53094818655506515, 66.25005786596111079, 1.601045042264325646 ) ) ;
#16303 = FACE_OUTER_BOUND ( 'NONE', #4954, .T. ) ;
#16302 = CARTESIAN_POINT ( 'NONE',  ( 3.915288987740546567, -32.15886406078164583, 7.257242401810560573 ) ) ;
#16304 = CARTESIAN_POINT ( 'NONE',  ( 30.11529565287584020, -4.511537616843412479, 1.859944388213511157 ) ) ;
#16305 = ADVANCED_FACE ( 'NONE', ( #19023 ), #34486, .F. ) ;
#16306 = DIRECTION ( 'NONE',  ( -0.3420201433256601642, -0.9396926207859115365, -0.000000000000000000 ) ) ;
#16307 = CARTESIAN_POINT ( 'NONE',  ( -70.31378976201078501, -21.58254907604969119, 9.981524770340065800 ) ) ;
#16308 = CARTESIAN_POINT ( 'NONE',  ( 0.3263088656926940168, -26.34351183019633069, 7.139344958878410807 ) ) ;
#16309 = ORIENTED_EDGE ( 'NONE', *, *, #35907, .F. ) ;
#16310 = CARTESIAN_POINT ( 'NONE',  ( 2.277526804980155362, -33.02201842327861669, 6.894806418505347700 ) ) ;
#16311 = LINE ( 'NONE', #22514, #13096 ) ;
#16312 = CARTESIAN_POINT ( 'NONE',  ( 31.93469105406368413, 0.01670955582175310053, -5.060964027022966327 ) ) ;
#16313 = LINE ( 'NONE', #10128, #32561 ) ;
#16314 = CARTESIAN_POINT ( 'NONE',  ( 4.367281360980026506, -27.30327784999532525, 7.743886751744251562 ) ) ;
#16315 = LINE ( 'NONE', #28883, #9533 ) ;
#16316 = CARTESIAN_POINT ( 'NONE',  ( -69.92837670882107659, 28.72470171467712063, 5.916079783099620570 ) ) ;
#16317 = EDGE_CURVE ( 'NONE', #309, #320, #35095, .T. ) ;
#16318 = CARTESIAN_POINT ( 'NONE',  ( -1.496426596291860811, -28.41215999167467743, 7.763628509615286610 ) ) ;
#16319 = CARTESIAN_POINT ( 'NONE',  ( 68.42229528291726126, 59.10113456467039583, -3.941639393089740651 ) ) ;
#16320 = CIRCLE ( 'NONE', #1889, 15.73502530973474478 ) ;
#16321 = VERTEX_POINT ( 'NONE', #12629 ) ;
#16322 = CARTESIAN_POINT ( 'NONE',  ( 5.401390093233090717, -28.86392406983564385, 6.954324564059724878 ) ) ;
#16324 = EDGE_CURVE ( 'NONE', #40691, #35752, #25200, .T. ) ;
#16323 = CARTESIAN_POINT ( 'NONE',  ( -64.08758708074094557, 37.77509509994077774, 3.093168342234559276 ) ) ;
#16325 = CARTESIAN_POINT ( 'NONE',  ( 22.59185701846717365, 3.735489254463754349, 3.886158523879209348 ) ) ;
#16326 = CARTESIAN_POINT ( 'NONE',  ( 1.097341463758161773, -26.22383283646636087, 7.756377446753166538 ) ) ;
#16327 = CARTESIAN_POINT ( 'NONE',  ( 4.392794304683587114, -31.80621346007680827, 7.640616322432098428 ) ) ;
#16328 = ORIENTED_EDGE ( 'NONE', *, *, #2641, .F. ) ;
#16329 = CARTESIAN_POINT ( 'NONE',  ( 22.18602618867068443, 5.272228373216523600, 3.073292335441606848 ) ) ;
#16330 = CARTESIAN_POINT ( 'NONE',  ( -40.24874870218063450, -26.64985754041175525, 6.700000000000000178 ) ) ;
#16331 = CARTESIAN_POINT ( 'NONE',  ( 79.42059605865688354, 65.48104909687435793, 2.923497156821689646 ) ) ;
#16332 = AXIS2_PLACEMENT_3D ( 'NONE', #29868, #14012, #11312 ) ;
#16333 = CYLINDRICAL_SURFACE ( 'NONE', #10090, 3.399999999999999911 ) ;
#16334 = VERTEX_POINT ( 'NONE', #19826 ) ;
#16335 = CARTESIAN_POINT ( 'NONE',  ( 78.41725481636187567, 64.09006905928654874, -3.590127757398426489 ) ) ;
#16336 =( BOUNDED_CURVE ( )  B_SPLINE_CURVE ( 3, ( #708, #32406, #13655, #13044 ),
 .UNSPECIFIED., .F., .T. ) 
 B_SPLINE_CURVE_WITH_KNOTS ( ( 4, 4 ),
 ( 1.347909859412854239, 1.534781240595298968 ),
 .UNSPECIFIED. ) 
 CURVE ( )  GEOMETRIC_REPRESENTATION_ITEM ( )  RATIONAL_B_SPLINE_CURVE ( ( 1.000000000000000000, 0.9970920404276226723, 0.9970920404276226723, 1.000000000000000000 ) ) 
 REPRESENTATION_ITEM ( '' )  );
#16337 = AXIS2_PLACEMENT_3D ( 'NONE', #37311, #15489, #24347 ) ;
#16339 = CARTESIAN_POINT ( 'NONE',  ( -1.713032059046489142, -28.79627056164295595, 7.013842709614101167 ) ) ;
#16338 = CARTESIAN_POINT ( 'NONE',  ( 21.79343922618468810, 0.2295100222190576966, 8.344713507481587911 ) ) ;
#16340 = CARTESIAN_POINT ( 'NONE',  ( 80.85068185327205015, 64.93836743323436167, -3.187395722549116961 ) ) ;
#16341 = CARTESIAN_POINT ( 'NONE',  ( 79.72787136111028872, 62.61980214589643623, 3.627744115730415775 ) ) ;
#16342 = EDGE_LOOP ( 'NONE', ( #8486, #17243, #14759, #11085 ) ) ;
#16343 = CARTESIAN_POINT ( 'NONE',  ( 11.65737507970504439, -27.06993018339339940, 6.800000000000000711 ) ) ;
#16344 = CARTESIAN_POINT ( 'NONE',  ( 79.33205627562975337, 66.30342423254383277, 1.132734665583299272 ) ) ;
#16345 = CARTESIAN_POINT ( 'NONE',  ( -64.08758708074093136, 44.09647858371769047, 1.000000000000000000 ) ) ;
#16346 = DIRECTION ( 'NONE',  ( 0.000000000000000000, 0.000000000000000000, -1.000000000000000000 ) ) ;
#16347 = CARTESIAN_POINT ( 'NONE',  ( 25.22633673370294360, -3.172752697882940343, -5.351597462314125586 ) ) ;
#16348 = ADVANCED_FACE ( 'NONE', ( #29893 ), #29098, .F. ) ;
#16349 = FACE_OUTER_BOUND ( 'NONE', #20013, .T. ) ;
#16350 = VERTEX_POINT ( 'NONE', #16712 ) ;
#16351 = CARTESIAN_POINT ( 'NONE',  ( -74.87498290905593024, -4.683714315110599102, 9.194508750764200045 ) ) ;
#16352 = CARTESIAN_POINT ( 'NONE',  ( 21.73387437812568734, 0.2123458951770110792, -9.115319698840053775 ) ) ;
#16353 = ORIENTED_EDGE ( 'NONE', *, *, #3110, .T. ) ;
#16354 = LINE ( 'NONE', #36313, #38618 ) ;
#16355 = CARTESIAN_POINT ( 'NONE',  ( 66.27376694608931018, 57.73522568913554665, -4.000000000000000000 ) ) ;
#16356 = CARTESIAN_POINT ( 'NONE',  ( 28.33577056900993085, -3.844698498189621283, -4.468379450010504961 ) ) ;
#16357 = CARTESIAN_POINT ( 'NONE',  ( 37.21170653579515175, -2.744006139658493826, -6.000908227333882294 ) ) ;
#16358 = CARTESIAN_POINT ( 'NONE',  ( 3.402382127344176777, -32.62823414405891498, 6.875671892026064214 ) ) ;
#16359 = CARTESIAN_POINT ( 'NONE',  ( 16.06488434713086022, 10.27331943285140703, 2.713711751702661434 ) ) ;
#16360 = CYLINDRICAL_SURFACE ( 'NONE', #20597, 0.09010775117052903516 ) ;
#16361 = CARTESIAN_POINT ( 'NONE',  ( -0.5596933955661176352, -26.89747389307597203, 7.635761828346574909 ) ) ;
#16362 = EDGE_CURVE ( 'NONE', #1149, #22787, #32996, .T. ) ;
#16363 = CARTESIAN_POINT ( 'NONE',  ( -59.87552183813137674, 24.84364830758654108, -9.800414904976365804 ) ) ;
#16364 = ADVANCED_FACE ( 'NONE', ( #16522 ), #10545, .T. ) ;
#16365 = ADVANCED_FACE ( 'NONE', ( #38750 ), #10352, .F. ) ;
#16366 = FACE_OUTER_BOUND ( 'NONE', #7519, .T. ) ;
#16367 = CARTESIAN_POINT ( 'NONE',  ( 25.86636253853731304, 2.039549717436321963, -4.181506972325073512 ) ) ;
#16368 = CARTESIAN_POINT ( 'NONE',  ( 28.98805360192195835, 1.403918898879884747, -4.132826440151677438 ) ) ;
#16369 = PLANE ( 'NONE',  #32830 ) ;
#16370 = ORIENTED_EDGE ( 'NONE', *, *, #14439, .F. ) ;
#16371 = EDGE_LOOP ( 'NONE', ( #28620, #24446, #4350, #28341 ) ) ;
#16372 = CARTESIAN_POINT ( 'NONE',  ( 66.85741207324237223, 57.95599960577073517, 3.999594749380519954 ) ) ;
#16373 = CARTESIAN_POINT ( 'NONE',  ( 88.23373314635465192, -2.194529332924425091, 2.156499936145213070 ) ) ;
#16374 = EDGE_CURVE ( 'NONE', #28154, #18594, #26417, .T. ) ;
#16375 = ORIENTED_EDGE ( 'NONE', *, *, #13335, .F. ) ;
#16376 = CARTESIAN_POINT ( 'NONE',  ( -78.43906097479739969, 10.12407436886776857, -8.325837142764415333 ) ) ;
#16377 = DIRECTION ( 'NONE',  ( 1.000000000000000000, 0.000000000000000000, 0.000000000000000000 ) ) ;
#16378 = DIRECTION ( 'NONE',  ( 0.1736481776669193677, 0.9848077530122099077, 0.000000000000000000 ) ) ;
#16379 = DIRECTION ( 'NONE',  ( -0.000000000000000000, -0.000000000000000000, 1.000000000000000000 ) ) ;
#16380 = TOROIDAL_SURFACE ( 'NONE', #36118, 80.68529983683480111, 3.000000000000000000 ) ;
#16381 = ORIENTED_EDGE ( 'NONE', *, *, #15481, .T. ) ;
#16382 = LINE ( 'NONE', #38004, #14967 ) ;
#16383 = ORIENTED_EDGE ( 'NONE', *, *, #3818, .F. ) ;
#16384 = CARTESIAN_POINT ( 'NONE',  ( 78.69934701664531929, 65.67047266146688855, -2.368006059521097217 ) ) ;
#16385 = CARTESIAN_POINT ( 'NONE',  ( -1.721720316595480860, -28.87059949175516849, 7.776484688137387025 ) ) ;
#16386 = CARTESIAN_POINT ( 'NONE',  ( 80.80742440666425352, 61.88848183320469332, 2.854164747637849775 ) ) ;
#16388 = ORIENTED_EDGE ( 'NONE', *, *, #1551, .F. ) ;
#16387 = CARTESIAN_POINT ( 'NONE',  ( -1.699493400058616821, -29.53742913049718766, 6.912949926530957967 ) ) ;
#16389 = EDGE_CURVE ( 'NONE', #3169, #12201, #7667, .T. ) ;
#16390 = FACE_OUTER_BOUND ( 'NONE', #20788, .T. ) ;
#16391 = AXIS2_PLACEMENT_3D ( 'NONE', #40143, #23877, #4959 ) ;
#16392 = CARTESIAN_POINT ( 'NONE',  ( 1.056572603559534418, -33.01021068541466263, 6.888594555015730592 ) ) ;
#16393 = CARTESIAN_POINT ( 'NONE',  ( -34.24874870218063450, -26.64985754041175525, 6.700000000000000178 ) ) ;
#16394 = CARTESIAN_POINT ( 'NONE',  ( 21.85643539959774984, 10.28856666709980594, -7.862822601098399034 ) ) ;
#16395 = CARTESIAN_POINT ( 'NONE',  ( 22.39111293279836090, 4.899164074087773990, -3.083163210143192057 ) ) ;
#16396 = ORIENTED_EDGE ( 'NONE', *, *, #23923, .T. ) ;
#16397 = CARTESIAN_POINT ( 'NONE',  ( 5.200213681912021713, -29.53468019335948824, 7.680160680325413658 ) ) ;
#16398 = EDGE_LOOP ( 'NONE', ( #7811, #24296, #32303, #21465 ) ) ;
#16399 = CARTESIAN_POINT ( 'NONE',  ( -1.011899981717923724, -31.62016981556380202, 6.882085323592687764 ) ) ;
#16400 = CARTESIAN_POINT ( 'NONE',  ( 4.281747078493526537, -27.35710481417712003, 7.691066658568948000 ) ) ;
#16401 = CARTESIAN_POINT ( 'NONE',  ( -73.27260478087752915, -2.820680093043031356, -9.724700656314139380 ) ) ;
#16402 = CARTESIAN_POINT ( 'NONE',  ( 4.716878747747901279, -27.79488195948977136, 7.730015791551948290 ) ) ;
#16403 = CARTESIAN_POINT ( 'NONE',  ( 4.256814889047467076, -33.88948601255670212, 7.695279973900954751 ) ) ;
#16404 = CARTESIAN_POINT ( 'NONE',  ( 80.58645273467570291, 64.40825618792595719, 3.509897338574980541 ) ) ;
#16405 = CARTESIAN_POINT ( 'NONE',  ( 84.23599009083828548, 2.852497016463987567, -2.111805961397795084 ) ) ;
#16406 = CARTESIAN_POINT ( 'NONE',  ( -0.01837800939314764015, -32.61883756299590686, 7.697032948437509070 ) ) ;
#16407 = CARTESIAN_POINT ( 'NONE',  ( -1.287675252634163270, -27.77617148390492474, 7.785593909369613819 ) ) ;
#16408 = CARTESIAN_POINT ( 'NONE',  ( 21.53535333134909635, 7.395104665118339859, -0.5014549742099433383 ) ) ;
#16409 = CARTESIAN_POINT ( 'NONE',  ( 33.33044624270629441, -1.121386909979642077, 5.408420254699600527 ) ) ;
#16410 = EDGE_CURVE ( 'NONE', #23047, #30342, #40373, .T. ) ;
#16411 = ADVANCED_FACE ( 'NONE', ( #23321 ), #26014, .F. ) ;
#16412 = AXIS2_PLACEMENT_3D ( 'NONE', #30913, #20324, #23625 ) ;
#16413 = DIRECTION ( 'NONE',  ( -0.000000000000000000, -0.000000000000000000, -1.000000000000000000 ) ) ;
#16414 = DIRECTION ( 'NONE',  ( -0.8660254037844344888, -0.5000000000000069944, -0.000000000000000000 ) ) ;
#16415 = CARTESIAN_POINT ( 'NONE',  ( -59.93345510331042902, 24.73247967741478703, -46.17089178453873188 ) ) ;
#16416 = DIRECTION ( 'NONE',  ( -0.000000000000000000, -0.000000000000000000, -1.000000000000000000 ) ) ;
#16417 = CARTESIAN_POINT ( 'NONE',  ( 68.45414103466679023, 59.01732383939346249, 3.957896739784462881 ) ) ;
#16418 = CARTESIAN_POINT ( 'NONE',  ( 37.04599030669736237, -2.800861170604020511, 5.988320766658103089 ) ) ;
#16419 = CARTESIAN_POINT ( 'NONE',  ( -64.08758708074093136, 43.50509228255777572, -1.592748443927769486 ) ) ;
#16420 = CARTESIAN_POINT ( 'NONE',  ( 88.48259847388298738, -1.030129646626848361, 1.133857545573457415 ) ) ;
#16421 = AXIS2_PLACEMENT_3D ( 'NONE', #6841, #15694, #28044 ) ;
#16422 = EDGE_LOOP ( 'NONE', ( #31533, #24631, #8415, #25710 ) ) ;
#16424 = CARTESIAN_POINT ( 'NONE',  ( 1.312110113526856914, -26.18508844559277549, 7.386948897581449458 ) ) ;
#16423 = CARTESIAN_POINT ( 'NONE',  ( 80.79424907316142423, 63.37012793878832184, -3.540619799101249576 ) ) ;
#16425 = CARTESIAN_POINT ( 'NONE',  ( -23.07867591359219617, -24.55319635012989110, 6.800000000000000711 ) ) ;
#16426 = ORIENTED_EDGE ( 'NONE', *, *, #36326, .T. ) ;
#16427 = CARTESIAN_POINT ( 'NONE',  ( 24.55255634016017297, -6.099742195186348859, -2.771823335699560964 ) ) ;
#16428 = ORIENTED_EDGE ( 'NONE', *, *, #32842, .T. ) ;
#16429 = CARTESIAN_POINT ( 'NONE',  ( -73.43598941707226402, -3.052414302668824853, 9.681195182795574894 ) ) ;
#16430 = ORIENTED_EDGE ( 'NONE', *, *, #29933, .F. ) ;
#16431 = CARTESIAN_POINT ( 'NONE',  ( 81.12912465015324415, 61.32884242822650833, -1.592560325354577255 ) ) ;
#16432 = B_SPLINE_CURVE_WITH_KNOTS ( 'NONE', 3,
 ( #33880, #2176, #30368, #23575 ),
 .UNSPECIFIED., .F., .F.,
 ( 4, 4 ),
 ( 8.940560153363745023E-19, 2.475319317933450300E-05 ),
 .UNSPECIFIED. ) ;
#16433 = CARTESIAN_POINT ( 'NONE',  ( -61.24591834330252027, -23.80776546975053520, 2.500000000000000000 ) ) ;
#16434 = CARTESIAN_POINT ( 'NONE',  ( 22.25885516624144600, 1.430813568335262964, 6.081876650313324362 ) ) ;
#16436 = ORIENTED_EDGE ( 'NONE', *, *, #20897, .F. ) ;
#16435 = ORIENTED_EDGE ( 'NONE', *, *, #25527, .F. ) ;
#16437 = VECTOR ( 'NONE', #22612, 1000.000000000000000 ) ;
#16438 = CARTESIAN_POINT ( 'NONE',  ( -0.009267658575196100618, -32.50883118978046582, 7.775108481317163367 ) ) ;
#16440 = CARTESIAN_POINT ( 'NONE',  ( 85.30059172038076554, 2.544051366058079466, 2.076667998869941911 ) ) ;
#16439 = CARTESIAN_POINT ( 'NONE',  ( 4.540213033195567682, -31.43953463181986407, 6.997764925645181933 ) ) ;
#16441 = CARTESIAN_POINT ( 'NONE',  ( -8.295002936191391285, 28.24537450226321411, -2.500000000000000000 ) ) ;
#16442 = B_SPLINE_SURFACE_WITH_KNOTS ( 'NONE', 5, 3, ( 
 ( #14996, #36618, #39490, #30448, #33352, #5331, #7997, #1645, #11890, #8804, #36417, #40111, #4920, #14183, #20553, #26753, #30040, #8189, #20761, #8402, #39293, #11485, #33556, #5128, #23651, #24259, #1855, #5531, #17866, #14377, #36822, #30243, #2058, #11279 ),
 ( #18075, #17661, #27145, #30664, #27555, #39697, #30870, #5944, #9420, #34583, #34987, #40718, #22417, #18279, #9017, #2678, #18482, #37225, #27959, #6150, #185, #15821, #21597, #27754, #2879, #18691, #40307, #3496, #16019, #12518, #25092, #15198, #394, #12932 ),
 ( #3299, #31069, #34788, #28376, #15401, #34177, #9637, #12723, #12313, #37621, #40502, #25297, #24888, #12097, #6565, #25494, #22008, #37425, #24674, #34377, #6360, #38042, #31274, #15611, #31476, #9221, #31678, #9842, #28163, #21800, #18907, #3094, #37832, #22218 ),
 ( #19111, #28584, #22619, #38642, #10636, #26110, #10439, #10037, #10833, #26503, #35585, #32295, #7554, #16418, #23213, #7159, #39034, #32099, #38841, #35389, #20109, #999, #28991, #7356, #10240, #23017, #25694, #23409, #29585, #13932, #792, #17010, #35187, #19314 ),
 ( #19914, #6960, #16605, #6762, #1401, #19721, #16811, #16220, #31886, #29391, #3697, #13322, #32689, #19519, #28789, #596, #4093, #38434, #3903, #4488, #32485, #38237, #13136, #1210, #13535, #29189, #25899, #22820, #4284, #13744, #26308, #35778, #40062, #11843 ),
 ( #17211, #8348, #7756, #39238, #21138, #33508, #1596, #27099, #20710, #7953, #36568, #17610, #30187, #36370, #20303, #32889, #4868, #33704, #5484, #2008, #14528, #30616, #27511, #14126, #4676, #5279, #27298, #20924, #20501, #11635, #30402, #33083, #11027, #39864 ),
 ( #39649, #17402, #2207, #29985, #29778, #24212, #18027, #11433, #1801, #26704, #11229, #23997, #2425, #8141, #33296, #36773, #14326, #14945, #26895, #5079, #39438, #23796, #27910, #16517, #30822, #18856, #25047, #6103, #9588, #31225, #37579, #29093, #15564, #12674 ),
 ( #895, #12476, #9177, #25250, #34129, #144, #24836, #24421, #8963, #15772, #12264, #37781, #18639, #5898, #9375, #40453, #40672, #2628, #36977, #6519, #31630, #18436, #34741, #27707, #21341, #15148, #33913, #40261, #31025, #2832, #3044, #5692, #28120, #21961 ),
 ( #6307, #18233, #15354, #22170, #12045, #24624, #37177, #21749, #37384, #21552, #19066, #34534, #34332, #31429, #3253, #28328, #23314, #26008, #1110, #4586, #29685, #30102, #35884, #17508, #13431, #4189, #38539, #13640, #32396, #23117, #1305, #36084, #10938, #16706 ),
 ( #26213, #14031, #7662, #29296, #1498, #13842, #26411, #35686, #7257, #20213, #17309, #7861, #26806, #38744, #19821, #10346, #10539, #38940, #7459, #14234, #4980, #20014, #39142, #32990, #4774, #35486, #26605, #22918, #32596, #39344, #23517, #4394, #17114, #10734 ),
 ( #16916, #11136, #23707, #32796, #20411, #8048, #29496, #29886, #1703, #36273, #20606, #33193, #30297, #18331, #40165, #2111, #5183, #34023, #27608, #36669, #36878, #27202, #37072, #11535, #18538, #30923, #24730, #21235, #8453, #11333, #17924, #33809, #37282, #2313 ),
 ( #23898, #15253, #9073, #39965, #1911, #5588, #5384, #21650, #8246, #8862, #2523, #24314, #27806, #8658, #15048, #34229, #18128, #2730, #6001, #14432, #30720, #11946, #24522, #21448, #5794, #40360, #24106, #21036, #27003, #12156, #39549, #36469, #20816, #33412 ),
 ( #17715, #14627, #39758, #33610, #30507, #14836, #27403, #11736, #2938, #21851, #28014, #6206, #25140, #9473, #25346, #38292, #12775, #37885, #34636, #7011, #12987, #25754, #35040, #19166, #34427, #34840, #13188, #37672, #35241, #10094, #16072, #22678, #28638, #234 ),
 ( #22272, #6818, #9694, #6615, #18749, #31123, #15454, #31732, #28427, #31940, #43, #19372, #31527, #40561, #15666, #22472, #18961, #3747, #3546, #12572, #443, #6410, #25551, #9273, #12373, #24943, #37476, #22062, #652, #31325, #28212, #3352, #38092, #9895 ),
 ( #16272, #28844, #19966, #29641, #29045, #26759, #1453, #39299, #1057, #20363, #35441, #3954, #13381, #16866, #10491, #22871, #32942, #38897, #38491, #16473, #13985, #13796, #29448, #32155, #7211, #10691, #35837, #36224, #1260, #23658, #19579, #10293, #850, #19775 ),
 ( #32350, #4730, #17063, #25959, #23271, #4343, #4145, #20164, #26364, #7611, #32545, #16659, #29246, #13590, #26164, #1653, #14188, #38694, #32750, #23073, #17264, #35640, #4542, #7410, #26558, #39094, #29838, #11086, #10890, #23465, #36033, #7812, #8003, #4925 ),
 ( #14578, #17458, #24054, #39915, #30877, #8409, #5337, #21189, #30045, #18081, #1860, #40313, #30669, #39497, #11689, #2683, #2063, #12102, #15206, #33760, #27759, #5540, #17871, #33561, #23847, #24267, #11896, #27356, #36829, #11284, #24680, #20559, #8611, #30455 ),
 ( #40118, #2262, #17666, #27151, #33143, #33971, #2478, #15001, #5744, #24469, #36423, #14382, #27561, #37026, #26951, #8194, #8810, #39704, #20765, #21396, #18286, #33359, #5133, #30248, #14787, #11491, #36623, #20982, #6570, #5948, #3703, #19116, #16224, #18697 ) ),
 .UNSPECIFIED., .F., .F., .F.,
 ( 6, 5, 2, 5, 6 ),
 ( 4, 1, 1, 1, 1, 1, 1, 1, 1, 1, 1, 1, 1, 1, 1, 1, 1, 1, 1, 1, 1, 1, 1, 1, 1, 1, 1, 1, 1, 1, 1, 4 ),
 ( -0.01000000000000000021, 0.000000000000000000, 0.5000000000000000000, 1.000000000000000000, 1.010000000000000009 ),
 ( 0.000000000000000000, 0.0006830822270650580572, 0.001366164454130116114, 0.001935399643350998100, 0.002390787794727703471, 0.002732328908260232229, 0.003016946502870673438, 0.003244640578559025799, 0.003386949375864246187, 0.003500796413708422584, 0.003586181692091554990, 0.003671566970474687830, 0.003756952248857819369, 0.003842337527240952209, 0.003956184565085128606, 0.004098493362390348560, 0.004269263919156613372, 0.004496957994844966167, 0.004781575589455406942, 0.005123116702987936567, 0.005578504854364642156, 0.006147740043585522840, 0.006830822270650581222, 0.007513904497715638738, 0.008424680800469050782, 0.009563151178910813885, 0.01092931563304092892, 0.01229548008717104568, 0.01411703269267786803, 0.01639397344956139424, 0.01912630235782162777, 0.02185863126608186130 ),
 .UNSPECIFIED. ) ;
#16443 = CARTESIAN_POINT ( 'NONE',  ( 71.70339147920792300, 60.88422586754656152, 3.784404822148339953 ) ) ;
#16444 = VERTEX_POINT ( 'NONE', #38945 ) ;
#16445 = CARTESIAN_POINT ( 'NONE',  ( 24.34601857225426613, 2.911169162268197663, -3.762662789421892029 ) ) ;
#16446 = ORIENTED_EDGE ( 'NONE', *, *, #3312, .T. ) ;
#16447 = EDGE_CURVE ( 'NONE', #14079, #10139, #10740, .T. ) ;
#16448 = ORIENTED_EDGE ( 'NONE', *, *, #23470, .F. ) ;
#16449 = CARTESIAN_POINT ( 'NONE',  ( 21.85643539959777826, -9.955546997263933662, -6.545918539092090427 ) ) ;
#16450 = EDGE_CURVE ( 'NONE', #11806, #15412, #38411, .T. ) ;
#16451 = VECTOR ( 'NONE', #30946, 1000.000000000000000 ) ;
#16452 = CARTESIAN_POINT ( 'NONE',  ( 21.85643539958836357, 4.448544635526659796, 2.117591927225508375 ) ) ;
#16453 = CARTESIAN_POINT ( 'NONE',  ( 0.3928816666250639633, -32.70848353550643139, 6.871394612369935651 ) ) ;
#16454 = CARTESIAN_POINT ( 'NONE',  ( 81.52287143523093960, 61.74508502528568954, 1.930361577756008806 ) ) ;
#16455 = CARTESIAN_POINT ( 'NONE',  ( 88.42327724305060599, -1.151963697325209202, 3.685007885677881401 ) ) ;
#16456 = ORIENTED_EDGE ( 'NONE', *, *, #22474, .T. ) ;
#16457 = ADVANCED_FACE ( 'NONE', ( #23122 ), #16921, .F. ) ;
#16458 = CARTESIAN_POINT ( 'NONE',  ( 0.5607539575979699764, -32.77325105075146894, 7.740055089680399902 ) ) ;
#16459 = DIRECTION ( 'NONE',  ( -0.7126435865141264037, 0.000000000000000000, -0.7015262779114428415 ) ) ;
#16460 = CARTESIAN_POINT ( 'NONE',  ( 35.96749414751118223, -2.128554350996951339, 5.819995357488987331 ) ) ;
#16461 = CARTESIAN_POINT ( 'NONE',  ( 5.075416774377466744, -29.15851806602221785, 6.887945620086119547 ) ) ;
#16462 = EDGE_CURVE ( 'NONE', #4265, #10217, #39148, .T. ) ;
#16463 = CARTESIAN_POINT ( 'NONE',  ( 36.19435599471948706, -2.231546916727529695, -5.855402635420312585 ) ) ;
#16464 = DIRECTION ( 'NONE',  ( -0.000000000000000000, -1.000000000000000000, -0.000000000000000000 ) ) ;
#16465 = CARTESIAN_POINT ( 'NONE',  ( 84.35969326541092528, 2.698637575869491378, 2.857603098124533947 ) ) ;
#16466 = DIRECTION ( 'NONE',  ( -1.000000000000000000, 6.367278819747327815E-17, -0.000000000000000000 ) ) ;
#16467 = CARTESIAN_POINT ( 'NONE',  ( 2.908998754795610875, -32.85463590341955609, 7.756742906098588186 ) ) ;
#16468 = CIRCLE ( 'NONE', #25038, 0.1000000000000028644 ) ;
#16469 = CARTESIAN_POINT ( 'NONE',  ( 3.431434570054124222, -32.49627346798381211, 7.695279973900954751 ) ) ;
#16470 = CARTESIAN_POINT ( 'NONE',  ( 30.68920804271916936, -3.119417099748506672, 4.996191155010656360 ) ) ;
#16471 = ORIENTED_EDGE ( 'NONE', *, *, #28207, .F. ) ;
#16472 = ORIENTED_EDGE ( 'NONE', *, *, #15201, .F. ) ;
#16473 = CARTESIAN_POINT ( 'NONE',  ( 36.44468416319452331, -1.733384222877294878, 5.731389134260409080 ) ) ;
#16474 = CARTESIAN_POINT ( 'NONE',  ( -1.613120284615923605, -28.77710995882498324, 7.386948897581451234 ) ) ;
#16475 = CARTESIAN_POINT ( 'NONE',  ( 66.58744840590414071, 57.78483400379950297, -3.999444518112384106 ) ) ;
#16476 = DIRECTION ( 'NONE',  ( -0.000000000000000000, -1.000000000000000000, -0.000000000000000000 ) ) ;
#16477 = ORIENTED_EDGE ( 'NONE', *, *, #33744, .T. ) ;
#16478 = AXIS2_PLACEMENT_3D ( 'NONE', #21441, #34017, #3539 ) ;
#16479 = CARTESIAN_POINT ( 'NONE',  ( 5.401390093233090717, -29.51577928193538369, 7.785387725071483800 ) ) ;
#16480 = FACE_OUTER_BOUND ( 'NONE', #24223, .T. ) ;
#16481 = FACE_BOUND ( 'NONE', #25053, .T. ) ;
#16482 = CARTESIAN_POINT ( 'NONE',  ( 3.844330250123625170, -32.33644520256172683, 6.870724624169666228 ) ) ;
#16483 = EDGE_LOOP ( 'NONE', ( #38141, #25771, #37865, #11792 ) ) ;
#16484 = CARTESIAN_POINT ( 'NONE',  ( 24.61641440591999341, 2.982913459046241833, 3.546506353475846307 ) ) ;
#16485 = CARTESIAN_POINT ( 'NONE',  ( 82.07520363809490505, 62.17599436785806688, -1.599335268229508111 ) ) ;
#16486 = CARTESIAN_POINT ( 'NONE',  ( 27.60344192425479193, 81.15229837709949834, 4.000000000000000000 ) ) ;
#16487 = ORIENTED_EDGE ( 'NONE', *, *, #9843, .F. ) ;
#16488 = CARTESIAN_POINT ( 'NONE',  ( 75.50377651103727317, 61.49872921062497255, -3.901127667181019110 ) ) ;
#16490 = CARTESIAN_POINT ( 'NONE',  ( 1.090397816225957328, 0.5999999999999995337, -4.012069227840649788 ) ) ;
#16489 = CARTESIAN_POINT ( 'NONE',  ( -25.39999999999996305, 0.000000000000000000, 2.500000000000000000 ) ) ;
#16491 = FACE_OUTER_BOUND ( 'NONE', #18408, .T. ) ;
#16492 = CARTESIAN_POINT ( 'NONE',  ( 77.35950424652857293, 60.48040194676344328, 3.253266109310522847 ) ) ;
#16493 = CARTESIAN_POINT ( 'NONE',  ( 4.339220620109727200, -27.42596629983610512, 6.889465824494258150 ) ) ;
#16494 = CARTESIAN_POINT ( 'NONE',  ( 1.803259918365761605, -26.07610587814439285, 7.771081512783698741 ) ) ;
#16495 = CARTESIAN_POINT ( 'NONE',  ( 22.36662521325363429, 4.219501547067421754, -3.697250822039899187 ) ) ;
#16496 = CARTESIAN_POINT ( 'NONE',  ( 81.61324681686122062, 61.62795767120283585, 1.465632304122483465 ) ) ;
#16497 = CARTESIAN_POINT ( 'NONE',  ( -0.2049548994135422797, -32.50585849072293598, 6.912143950357353184 ) ) ;
#16498 = CARTESIAN_POINT ( 'NONE',  ( 28.70293208761703241, -1.592347763559425200, -5.966126087555218227 ) ) ;
#16499 = CARTESIAN_POINT ( 'NONE',  ( -1.699556639465169106, -29.59009428628278471, 7.643333865083955736 ) ) ;
#16500 = LINE ( 'NONE', #38928, #18941 ) ;
#16501 = EDGE_CURVE ( 'NONE', #28513, #13346, #38935, .T. ) ;
#16502 = ADVANCED_FACE ( 'NONE', ( #32204 ), #901, .F. ) ;
#16503 = DIRECTION ( 'NONE',  ( -0.000000000000000000, -0.000000000000000000, -1.000000000000000000 ) ) ;
#16504 = CARTESIAN_POINT ( 'NONE',  ( 0.7269655568601173234, -26.31225054053048140, 6.911401339314956260 ) ) ;
#16505 = PLANE ( 'NONE',  #15085 ) ;
#16506 = AXIS2_PLACEMENT_3D ( 'NONE', #25905, #1406, #16610 ) ;
#16507 = EDGE_CURVE ( 'NONE', #10538, #1864, #29302, .T. ) ;
#16508 = CARTESIAN_POINT ( 'NONE',  ( 35.10421778843286944, -1.272554766392203440, -5.608957993449237733 ) ) ;
#16509 = CARTESIAN_POINT ( 'NONE',  ( 1.134318422345943267, -32.92248114710984197, 7.740055089680399014 ) ) ;
#16510 = DIRECTION ( 'NONE',  ( -0.9396926207859104263, 0.3420201433256631063, -0.000000000000000000 ) ) ;
#16511 = B_SPLINE_CURVE_WITH_KNOTS ( 'NONE', 3,
 ( #14973, #40086, #11660, #21160, #6127, #15172, #2448, #24235, #40695, #37000, #5923, #12287, #33727, #36796, #3071, #18255, #2653, #34355, #11865, #18663, #24440, #27730, #33939, #31250, #37200, #18461, #5714, #30846, #31047, #2855, #15376 ),
 .UNSPECIFIED., .F., .F.,
 ( 4, 3, 3, 3, 3, 3, 3, 3, 3, 3, 4 ),
 ( 8.673617379884035472E-19, 3.077658087705409682E-05, 6.152638666998541184E-05, 9.267501192706129737E-05, 0.0001241882240135219902, 0.0001556618703051623547, 0.0001866161554452190510, 0.0002167966385860956805, 0.0002463805737537764053, 0.0002758761370306536285, 0.0002847094172290138311 ),
 .UNSPECIFIED. ) ;
#16512 = CARTESIAN_POINT ( 'NONE',  ( 3.339037877594524417, -32.54901303308319171, 7.784476445165072533 ) ) ;
#16513 = CARTESIAN_POINT ( 'NONE',  ( -1.551693178343154012, -28.31429354101616269, 7.784725160561910329 ) ) ;
#16514 = CARTESIAN_POINT ( 'NONE',  ( 14.77222812468899349, 12.33286846116284252, -2.511961485181726239 ) ) ;
#16515 = DIRECTION ( 'NONE',  ( -0.000000000000000000, -0.000000000000000000, 1.000000000000000000 ) ) ;
#16516 = ORIENTED_EDGE ( 'NONE', *, *, #24074, .F. ) ;
#16517 = CARTESIAN_POINT ( 'NONE',  ( 34.36128308910517859, -1.406858267515045169, 5.569307275463330598 ) ) ;
#16518 = DIRECTION ( 'NONE',  ( 0.4999999999999979461, 0.8660254037844397068, -0.000000000000000000 ) ) ;
#16519 = CARTESIAN_POINT ( 'NONE',  ( 67.83896914621323049, 57.99724189137371155, -3.982857479566772607 ) ) ;
#16520 = CARTESIAN_POINT ( 'NONE',  ( -25.07867591359219617, -26.64985754041175525, 6.700000000000000178 ) ) ;
#16521 = EDGE_LOOP ( 'NONE', ( #19191, #17665, #21197, #34531 ) ) ;
#16522 = FACE_OUTER_BOUND ( 'NONE', #3416, .T. ) ;
#16523 = DIRECTION ( 'NONE',  ( -7.232507224765808510E-18, 1.000000000000000000, 0.000000000000000000 ) ) ;
#16524 = CARTESIAN_POINT ( 'NONE',  ( 23.02262922662109546, 3.378767241194165383, 3.887974689243142823 ) ) ;
#16525 = CARTESIAN_POINT ( 'NONE',  ( 0.9145606489677439166, -32.87787577969059782, 6.911401339314955372 ) ) ;
#16526 = CARTESIAN_POINT ( 'NONE',  ( 1.230319205269136518, -26.20258206353872765, 7.754798119455333705 ) ) ;
#16527 = CARTESIAN_POINT ( 'NONE',  ( -64.08758708074093136, 43.61223004741322740, -1.000000000000000000 ) ) ;
#16528 = ORIENTED_EDGE ( 'NONE', *, *, #31297, .F. ) ;
#16529 = CARTESIAN_POINT ( 'NONE',  ( 23.14201580508249734, 4.050829872694250433, 3.071595331972348131 ) ) ;
#16530 = CARTESIAN_POINT ( 'NONE',  ( 81.74784679736075077, 61.69507302169112251, -1.000000000000000000 ) ) ;
#16531 = CARTESIAN_POINT ( 'NONE',  ( 79.30685661404396569, 65.70718262327383741, 2.676159939830902168 ) ) ;
#16532 = VECTOR ( 'NONE', #39707, 1000.000000000000000 ) ;
#16533 = CARTESIAN_POINT ( 'NONE',  ( 0.4788954889883382249, -26.28999729831613053, 7.737115613922530777 ) ) ;
#16534 = VERTEX_POINT ( 'NONE', #32602 ) ;
#16535 = CARTESIAN_POINT ( 'NONE',  ( 80.24754081275330009, 61.06584331557482415, -2.177161688561031649 ) ) ;
#16537 = CARTESIAN_POINT ( 'NONE',  ( 14.61802060715431750, -4.492938368545131844, -2.500000000000015987 ) ) ;
#16536 = CARTESIAN_POINT ( 'NONE',  ( 25.39364064017554767, 0.7063433326595477402, 4.600238427421414755 ) ) ;
#16538 = CARTESIAN_POINT ( 'NONE',  ( 81.48777377604515948, 63.71638886501444432, -3.187395722549115185 ) ) ;
#16539 = CARTESIAN_POINT ( 'NONE',  ( 80.56990227295247564, 61.62418804268437356, 2.732428818688230621 ) ) ;
#16540 = ORIENTED_EDGE ( 'NONE', *, *, #38522, .F. ) ;
#16541 = CARTESIAN_POINT ( 'NONE',  ( -1.627984416835427162, -30.65173788820889200, 7.754798119455333705 ) ) ;
#16542 = CARTESIAN_POINT ( 'NONE',  ( 82.54941478318340842, 63.90107490703085347, 1.303631908148715990 ) ) ;
#16543 = CARTESIAN_POINT ( 'NONE',  ( -63.60823941500427736, 43.84876827539012822, 2.657415981336364919 ) ) ;
#16544 = CARTESIAN_POINT ( 'NONE',  ( 22.46150523612397976, 0.3089437977474873143, 9.145744397224946809 ) ) ;
#16545 = CARTESIAN_POINT ( 'NONE',  ( 5.085231831033718564, -29.18165020368717322, 7.386948897581451234 ) ) ;
#16546 = ORIENTED_EDGE ( 'NONE', *, *, #1562, .T. ) ;
#16547 = CARTESIAN_POINT ( 'NONE',  ( -75.80815061396138788, -5.389879833924653418, 8.736367909994982028 ) ) ;
#16548 = CARTESIAN_POINT ( 'NONE',  ( 24.12050462314963895, 0.4787749110952863596, -5.098002984902643142 ) ) ;
#16549 = CARTESIAN_POINT ( 'NONE',  ( -63.96477757089261473, 34.57625524247897175, 15.50000000000000000 ) ) ;
#16550 = ORIENTED_EDGE ( 'NONE', *, *, #22056, .T. ) ;
#16551 = DIRECTION ( 'NONE',  ( -0.000000000000000000, -0.000000000000000000, 1.000000000000000000 ) ) ;
#16552 = EDGE_CURVE ( 'NONE', #22181, #32450, #12619, .T. ) ;
#16553 = CARTESIAN_POINT ( 'NONE',  ( 21.73904017688714063, 4.235523729101259072, -2.801162699060028238 ) ) ;
#16554 = CARTESIAN_POINT ( 'NONE',  ( 1.700390093233090871, -29.56993018339339940, -8.199999999999999289 ) ) ;
#16555 = CARTESIAN_POINT ( 'NONE',  ( 19.02452760875551618, 7.104206974277733622, 3.175635661921960118 ) ) ;
#16556 = DIRECTION ( 'NONE',  ( -0.9848077530122149037, 0.1736481776668921395, 0.000000000000000000 ) ) ;
#16557 = LINE ( 'NONE', #29136, #39113 ) ;
#16558 = CARTESIAN_POINT ( 'NONE',  ( 3.475438317136747113, -32.58641883790819094, 7.730015791551950954 ) ) ;
#16559 = CARTESIAN_POINT ( 'NONE',  ( -18.87867591359219333, -26.64985754041175525, 6.800000000000000711 ) ) ;
#16560 = CARTESIAN_POINT ( 'NONE',  ( 31.70551703006545097, 0.3859655886019467408, -4.660405379804645420 ) ) ;
#16561 = CARTESIAN_POINT ( 'NONE',  ( -62.92837670882106238, -39.37473357531882101, -6.000000000000000000 ) ) ;
#16562 = VERTEX_POINT ( 'NONE', #17513 ) ;
#16563 = CARTESIAN_POINT ( 'NONE',  ( 66.73816075044196339, 57.82680446425992926, 3.998864354716218816 ) ) ;
#16564 = VECTOR ( 'NONE', #22679, 1000.000000000000000 ) ;
#16565 = CARTESIAN_POINT ( 'NONE',  ( 21.71182896267971074, 6.328908860361642574, -3.192117583127509928 ) ) ;
#16566 = CARTESIAN_POINT ( 'NONE',  ( 84.75081314860828741, 2.206698042984908792, -4.319373971756642838 ) ) ;
#16567 = DIRECTION ( 'NONE',  ( 0.000000000000000000, 0.000000000000000000, -1.000000000000000000 ) ) ;
#16568 =( BOUNDED_CURVE ( )  B_SPLINE_CURVE ( 3, ( #25033, #12662, #15758, #34727 ),
 .UNSPECIFIED., .F., .T. ) 
 B_SPLINE_CURVE_WITH_KNOTS ( ( 4, 4 ),
 ( 4.708531083176466403, 4.712388980384689674 ),
 .UNSPECIFIED. ) 
 CURVE ( )  GEOMETRIC_REPRESENTATION_ITEM ( )  RATIONAL_B_SPLINE_CURVE ( ( 1.000000000000000000, 0.9999987597194787137, 0.9999987597194787137, 1.000000000000000000 ) ) 
 REPRESENTATION_ITEM ( '' )  );
#16569 = ORIENTED_EDGE ( 'NONE', *, *, #39786, .T. ) ;
#16570 = CARTESIAN_POINT ( 'NONE',  ( -80.84835038658981432, 10.51112849907171132, -4.793973201337777823 ) ) ;
#16571 = EDGE_CURVE ( 'NONE', #37970, #11084, #36884, .T. ) ;
#16572 = CARTESIAN_POINT ( 'NONE',  ( 2.911470930621151698, -26.29543661044079528, 7.778495531946298058 ) ) ;
#16573 = CARTESIAN_POINT ( 'NONE',  ( 0.000000000000000000, 0.000000000000000000, 0.000000000000000000 ) ) ;
#16574 = EDGE_LOOP ( 'NONE', ( #12862, #2638, #20760, #24010 ) ) ;
#16575 = CARTESIAN_POINT ( 'NONE',  ( 4.008117074447018702, -26.95213428602776773, 7.780491323090171107 ) ) ;
#16576 = EDGE_LOOP ( 'NONE', ( #4551, #8820, #11358, #1816 ) ) ;
#16577 = CARTESIAN_POINT ( 'NONE',  ( 79.74463803169643938, 63.93878357801280288, -3.720735635808768649 ) ) ;
#16578 = CARTESIAN_POINT ( 'NONE',  ( 79.74463803169676623, 63.93878357801307999, 3.720735635808746888 ) ) ;
#16580 = ORIENTED_EDGE ( 'NONE', *, *, #25748, .T. ) ;
#16579 = DIRECTION ( 'NONE',  ( -1.000000000000000000, 0.000000000000000000, 0.000000000000000000 ) ) ;
#16581 = ADVANCED_FACE ( 'NONE', ( #4986 ), #39555, .T. ) ;
#16582 = CARTESIAN_POINT ( 'NONE',  ( -72.46964309959683703, 39.11862660440054640, 15.50000000000000000 ) ) ;
#16583 = APPLICATION_CONTEXT ( 'automotive_design' ) ;
#16584 = CARTESIAN_POINT ( 'NONE',  ( 0.9649312406235903694, -32.99179965756316335, 6.868546646838339598 ) ) ;
#16585 = CARTESIAN_POINT ( 'NONE',  ( 3.578684702212876712, -26.72740941926953440, 7.386948897581451234 ) ) ;
#16586 = CARTESIAN_POINT ( 'NONE',  ( 21.85643539959774273, -7.673977846683588844, 14.52234238348545681 ) ) ;
#16587 = VERTEX_POINT ( 'NONE', #17930 ) ;
#16588 = LINE ( 'NONE', #29761, #1847 ) ;
#16589 = AXIS2_PLACEMENT_3D ( 'NONE', #960, #13704, #16378 ) ;
#16590 = CARTESIAN_POINT ( 'NONE',  ( -1.021081023829336187, -31.60797530386227905, 6.895222827070024429 ) ) ;
#16591 = CARTESIAN_POINT ( 'NONE',  ( -0.5635009794871607136, -32.22451875026029455, 7.781480525794719050 ) ) ;
#16592 = CARTESIAN_POINT ( 'NONE',  ( -72.46938654171589178, -1.268490862809277919, -9.881656514212606268 ) ) ;
#16593 = ADVANCED_FACE ( 'NONE', ( #24320 ), #27613, .F. ) ;
#16594 = CYLINDRICAL_SURFACE ( 'NONE', #14898, 7.744449365083023729 ) ;
#16595 = DIRECTION ( 'NONE',  ( 0.000000000000000000, 0.000000000000000000, 1.000000000000000000 ) ) ;
#16596 = CARTESIAN_POINT ( 'NONE',  ( 81.09339258687020902, 63.16289930221481796, 3.352621494407052705 ) ) ;
#16597 = CARTESIAN_POINT ( 'NONE',  ( 84.10013685850573495, 3.017793503712738357, 0.3246723698904760980 ) ) ;
#16598 = CARTESIAN_POINT ( 'NONE',  ( -32.97867591359219119, -26.64985754041175525, 6.800000000000000711 ) ) ;
#16599 = CARTESIAN_POINT ( 'NONE',  ( 2.931137878888503856, -32.84640083007458600, 7.698786668945013290 ) ) ;
#16600 = CARTESIAN_POINT ( 'NONE',  ( -0.4574210171174859507, -32.19744825413003753, 7.695279973900954751 ) ) ;
#16601 = DIRECTION ( 'NONE',  ( -1.000000000000000000, 0.000000000000000000, 0.000000000000000000 ) ) ;
#16602 = CARTESIAN_POINT ( 'NONE',  ( 20.58577122809306204, 5.855186692365746737, -3.419305487539204158 ) ) ;
#16603 = FACE_OUTER_BOUND ( 'NONE', #9615, .T. ) ;
#16604 = DIRECTION ( 'NONE',  ( -0.000000000000000000, -0.000000000000000000, -1.000000000000000000 ) ) ;
#16605 = CARTESIAN_POINT ( 'NONE',  ( 34.13616914347945652, -3.136032219204479610, 5.534172799846977853 ) ) ;
#16606 = EDGE_CURVE ( 'NONE', #1810, #14763, #21242, .T. ) ;
#16607 = DIRECTION ( 'NONE',  ( 1.000000000000000000, 0.000000000000000000, 0.000000000000000000 ) ) ;
#16608 = CARTESIAN_POINT ( 'NONE',  ( 86.64693249831780975, 1.031777503091004800, -5.158387491453222395 ) ) ;
#16610 = DIRECTION ( 'NONE',  ( 1.000000000000000000, 0.000000000000000000, 0.000000000000000000 ) ) ;
#16609 = CARTESIAN_POINT ( 'NONE',  ( 81.21586879471323073, 61.61940358760092806, -2.137206601789636728 ) ) ;
#16611 = CARTESIAN_POINT ( 'NONE',  ( 4.359062294607612742, -27.29364649790398190, 7.678495282201406091 ) ) ;
#16612 =( GEOMETRIC_REPRESENTATION_CONTEXT ( 3 ) GLOBAL_UNCERTAINTY_ASSIGNED_CONTEXT ( ( #9805 ) ) GLOBAL_UNIT_ASSIGNED_CONTEXT ( ( #32556, #16671, #28649 ) ) REPRESENTATION_CONTEXT ( 'NONE', 'WORKASPACE' ) );
#16613 = VERTEX_POINT ( 'NONE', #27409 ) ;
#16614 = CARTESIAN_POINT ( 'NONE',  ( -61.00670947824507806, 24.84364830758654108, -8.800414904976364028 ) ) ;
#16615 = EDGE_LOOP ( 'NONE', ( #39678, #8625, #4634, #38466, #33740 ) ) ;
#16616 = CARTESIAN_POINT ( 'NONE',  ( -80.91065676098010329, -6.597313057213482601, -0.5950503846463383040 ) ) ;
#16617 = ORIENTED_EDGE ( 'NONE', *, *, #2408, .F. ) ;
#16618 = B_SPLINE_CURVE_WITH_KNOTS ( 'NONE', 5,
 ( #39301, #23075, #13987, #29644, #39097, #7814, #20365, #32945 ),
 .UNSPECIFIED., .F., .F.,
 ( 6, 2, 6 ),
 ( 0.000000000000000000, 0.5000000000000000000, 1.000000000000000000 ),
 .UNSPECIFIED. ) ;
#16619 = ORIENTED_EDGE ( 'NONE', *, *, #76, .F. ) ;
#16620 = CARTESIAN_POINT ( 'NONE',  ( 81.04529349509148517, 61.25860024526324565, -1.340350474428863459 ) ) ;
#16621 = EDGE_CURVE ( 'NONE', #32349, #16283, #30805, .T. ) ;
#16622 = CARTESIAN_POINT ( 'NONE',  ( 4.927610109650206738, -30.92457071343696384, 7.013842709614101167 ) ) ;
#16623 = ADVANCED_FACE ( 'NONE', ( #36279 ), #20613, .F. ) ;
#16624 = CARTESIAN_POINT ( 'NONE',  ( 26.09009134676806241, 1.922323258887854269, 4.227532586804973569 ) ) ;
#16626 = ORIENTED_EDGE ( 'NONE', *, *, #3064, .T. ) ;
#16625 = ORIENTED_EDGE ( 'NONE', *, *, #28207, .T. ) ;
#16627 = ADVANCED_FACE ( 'NONE', ( #26813 ), #11339, .T. ) ;
#16628 = AXIS2_PLACEMENT_3D ( 'NONE', #15302, #2572, #21700 ) ;
#16629 = CARTESIAN_POINT ( 'NONE',  ( 5.038969279218838970, -30.21327822487392112, 6.889465824494254598 ) ) ;
#16630 = CARTESIAN_POINT ( 'NONE',  ( 14.73664178711198147, 12.61985148690504133, -2.505541970458011747 ) ) ;
#16631 = DIRECTION ( 'NONE',  ( 1.000000000000000000, -8.921435019309294079E-15, 0.000000000000000000 ) ) ;
#16632 = CARTESIAN_POINT ( 'NONE',  ( 72.42208042952545100, 59.16915255968121556, 3.823636340456165073 ) ) ;
#16633 = EDGE_LOOP ( 'NONE', ( #2027, #37004, #24, #11188 ) ) ;
#16634 = CARTESIAN_POINT ( 'NONE',  ( 22.81500972751208067, 3.448192808966587197, -3.952749550737099327 ) ) ;
#16635 = VERTEX_POINT ( 'NONE', #2117 ) ;
#16636 = CARTESIAN_POINT ( 'NONE',  ( -71.72734076235239797, -0.1676685021849017854, 5.947290612307118529 ) ) ;
#16637 = ORIENTED_EDGE ( 'NONE', *, *, #36071, .F. ) ;
#16638 = CARTESIAN_POINT ( 'NONE',  ( 21.85643539959777826, -5.315239383820637542, 13.63683724657638052 ) ) ;
#16639 = CARTESIAN_POINT ( 'NONE',  ( 19.99661396372949440, 11.93735323785185543, 1.251290237290588149E-12 ) ) ;
#16640 = CARTESIAN_POINT ( 'NONE',  ( 0.3523192157778118339, -32.69126323727760308, 6.997764925645181933 ) ) ;
#16641 = CARTESIAN_POINT ( 'NONE',  ( 81.16407079065473340, 61.30196360636995934, 1.071687152257631004 ) ) ;
#16642 = CARTESIAN_POINT ( 'NONE',  ( 86.36811837411410409, 0.9377611381114191458, -5.884791073222536362 ) ) ;
#16643 = CARTESIAN_POINT ( 'NONE',  ( -1.784963795961492350, -29.52657984859756723, 7.785096263473211486 ) ) ;
#16644 = ORIENTED_EDGE ( 'NONE', *, *, #27420, .F. ) ;
#16645 = VECTOR ( 'NONE', #18591, 1000.000000000000227 ) ;
#16646 = CARTESIAN_POINT ( 'NONE',  ( 33.94823428658630604, -3.200574468876375533, 5.504841020207380531 ) ) ;
#16647 = CARTESIAN_POINT ( 'NONE',  ( 31.54670663170724865, -3.759141947944208084, 4.713116287240913138 ) ) ;
#16648 = CARTESIAN_POINT ( 'NONE',  ( 14.67364265041105753, -5.606975079573447651, -2.496574837622112408 ) ) ;
#16649 = CARTESIAN_POINT ( 'NONE',  ( 36.97956974538411146, -2.956624624668434009, -5.977954231677896857 ) ) ;
#16650 = DIRECTION ( 'NONE',  ( 1.000000000000000000, 0.000000000000000000, 0.000000000000000000 ) ) ;
#16651 = CARTESIAN_POINT ( 'NONE',  ( -74.96765694090700549, -3.041086699640438429, 10.49870045681198683 ) ) ;
#16652 = CARTESIAN_POINT ( 'NONE',  ( -4.890026461918812295, -8.951974136083761024, -2.500000000000000000 ) ) ;
#16653 = ADVANCED_FACE ( 'NONE', ( #39767 ), #24112, .F. ) ;
#16654 = CARTESIAN_POINT ( 'NONE',  ( 5.585000075404096265, -26.15135101585522293, 7.754798119455333705 ) ) ;
#16655 = CIRCLE ( 'NONE', #2893, 0.1000000000000028644 ) ;
#16656 = CARTESIAN_POINT ( 'NONE',  ( 33.44795012684379287, -3.712436240568119494, 5.220878576662950188 ) ) ;
#16657 = ORIENTED_EDGE ( 'NONE', *, *, #20915, .T. ) ;
#16658 = ORIENTED_EDGE ( 'NONE', *, *, #19766, .T. ) ;
#16659 = CARTESIAN_POINT ( 'NONE',  ( 37.10451636438106249, -3.126525554563963194, 5.976203789056629745 ) ) ;
#16660 = CARTESIAN_POINT ( 'NONE',  ( 1.672485556746682533, -33.05866413503350287, 7.781480525794718162 ) ) ;
#16661 = CARTESIAN_POINT ( 'NONE',  ( 2.183653651549320340, -33.03640625185305879, 7.750000000000000888 ) ) ;
#16662 = EDGE_CURVE ( 'NONE', #39861, #33383, #7235, .T. ) ;
#16663 = AXIS2_PLACEMENT_3D ( 'NONE', #5558, #30690, #27584 ) ;
#16664 = ORIENTED_EDGE ( 'NONE', *, *, #21151, .T. ) ;
#16665 = B_SPLINE_CURVE_WITH_KNOTS ( 'NONE', 3,
 ( #17080, #17475, #867, #32362 ),
 .UNSPECIFIED., .F., .F.,
 ( 4, 4 ),
 ( 8.673617379884035472E-19, 6.391136169900847399E-06 ),
 .UNSPECIFIED. ) ;
#16666 = EDGE_CURVE ( 'NONE', #28306, #31466, #7917, .T. ) ;
#16667 = CARTESIAN_POINT ( 'NONE',  ( -64.08758708074094557, 37.43074634368117160, -3.182173495013627562 ) ) ;
#16668 = DIRECTION ( 'NONE',  ( -0.000000000000000000, -0.000000000000000000, 1.000000000000000000 ) ) ;
#16669 = ORIENTED_EDGE ( 'NONE', *, *, #16277, .F. ) ;
#16670 = FACE_OUTER_BOUND ( 'NONE', #30516, .T. ) ;
#16671 =( NAMED_UNIT ( * ) PLANE_ANGLE_UNIT ( ) SI_UNIT ( $, .RADIAN. ) );
#16672 = VERTEX_POINT ( 'NONE', #32202 ) ;
#16673 = EDGE_CURVE ( 'NONE', #36487, #39450, #4002, .T. ) ;
#16674 = CARTESIAN_POINT ( 'NONE',  ( 81.68900298540734184, 61.66555023304466232, -1.322881339814839352 ) ) ;
#16675 = DIRECTION ( 'NONE',  ( -1.000000000000000000, 0.000000000000000000, 0.000000000000000000 ) ) ;
#16676 = ORIENTED_EDGE ( 'NONE', *, *, #20970, .T. ) ;
#16677 = CARTESIAN_POINT ( 'NONE',  ( 76.25423822322979106, 59.84407948384421161, -3.204585025132130394 ) ) ;
#16679 = CARTESIAN_POINT ( 'NONE',  ( 4.394189364466743797, -27.35572347332146848, 7.783750581861601070 ) ) ;
#16678 = CARTESIAN_POINT ( 'NONE',  ( 2.470422062425372545, -26.15568784190358542, 6.890920332093119605 ) ) ;
#16680 = CARTESIAN_POINT ( 'NONE',  ( 21.49033551098300165, 5.616517115020018380, -3.514817270055297094 ) ) ;
#16681 = CARTESIAN_POINT ( 'NONE',  ( 77.48353911088555890, 60.20448024992288083, 2.970791854446974689 ) ) ;
#16682 = B_SPLINE_CURVE_WITH_KNOTS ( 'NONE', 3,
 ( #10728, #23310, #20009, #4386, #13837, #16911, #29492, #21732, #14927, #18214, #6083, #24606, #30806, #34314, #12655, #9156 ),
 .UNSPECIFIED., .F., .F.,
 ( 4, 3, 3, 3, 3, 4 ),
 ( 2.455293198023857654E-05, 3.025503081355709683E-05, 6.050996021720427811E-05, 9.076574948361131121E-05, 0.0001210199690674203720, 0.0001477826154599604504 ),
 .UNSPECIFIED. ) ;
#16683 = CARTESIAN_POINT ( 'NONE',  ( -6.978675913592191193, -26.64985754041175525, 6.700000000000000178 ) ) ;
#16684 = VECTOR ( 'NONE', #13040, 1000.000000000000000 ) ;
#16685 = DIRECTION ( 'NONE',  ( 1.000000000000000000, 0.000000000000000000, 0.000000000000000000 ) ) ;
#16686 = DIRECTION ( 'NONE',  ( 0.7126435865141282910, 0.000000000000000000, 0.7015262779114409541 ) ) ;
#16687 = DIRECTION ( 'NONE',  ( 0.000000000000000000, 0.000000000000000000, 1.000000000000000000 ) ) ;
#16688 = CARTESIAN_POINT ( 'NONE',  ( 82.03714350014182344, 63.99860240201152095, 2.622983904469076144 ) ) ;
#16689 = CARTESIAN_POINT ( 'NONE',  ( -0.07645708395594488782, -32.58535952412007930, 6.894806418505347700 ) ) ;
#16690 = CARTESIAN_POINT ( 'NONE',  ( 26.56136967304951213, 3.021295450130037530, 0.006841891102512360698 ) ) ;
#16691 = CARTESIAN_POINT ( 'NONE',  ( 2.408319516247223735, -26.24444671129270290, 7.757178535559534183 ) ) ;
#16692 = CARTESIAN_POINT ( 'NONE',  ( -70.92837670882238399, -21.78299143689875095, 10.00000000000113154 ) ) ;
#16693 = AXIS2_PLACEMENT_3D ( 'NONE', #8925, #21508, #34086 ) ;
#16694 = LINE ( 'NONE', #19611, #1820 ) ;
#16695 = CARTESIAN_POINT ( 'NONE',  ( 0.7311680052080280490, -26.31100152636673783, 6.920489980334479263 ) ) ;
#16696 = CARTESIAN_POINT ( 'NONE',  ( -24.97867591359219475, -26.64985754041175525, 6.700000000000000178 ) ) ;
#16697 = CARTESIAN_POINT ( 'NONE',  ( 35.04487071626047623, -1.406682813658225673, -5.661182748920821517 ) ) ;
#16698 = AXIS2_PLACEMENT_3D ( 'NONE', #35260, #7029, #19598 ) ;
#16699 = CARTESIAN_POINT ( 'NONE',  ( 1.040749578662133024, -32.90534253841714474, 7.784476445165072533 ) ) ;
#16700 = CARTESIAN_POINT ( 'NONE',  ( -20.44874870218064444, -26.64985754041175525, 6.700000000000000178 ) ) ;
#16701 = CARTESIAN_POINT ( 'NONE',  ( 3.411503134503389933, -32.50797839004665946, 7.756377446753164762 ) ) ;
#16702 = CARTESIAN_POINT ( 'NONE',  ( -63.08758708074093136, 41.04287353446839859, -4.000000000000000000 ) ) ;
#16703 = CARTESIAN_POINT ( 'NONE',  ( -26.44874870218064089, -26.64985754041175525, 6.700000000000000178 ) ) ;
#16704 = DIRECTION ( 'NONE',  ( 0.9848077530122103518, -0.1736481776669172583, -0.000000000000000000 ) ) ;
#16705 = VERTEX_POINT ( 'NONE', #899 ) ;
#16706 = CARTESIAN_POINT ( 'NONE',  ( 20.66011059366096703, 4.228419983037499996, 3.378133128719581268 ) ) ;
#16707 = DIRECTION ( 'NONE',  ( 0.7660444431189857850, -0.6427876096865299260, -0.000000000000000000 ) ) ;
#16708 = CARTESIAN_POINT ( 'NONE',  ( 67.12475893546654504, 58.13278081555189658, -3.997693602769901045 ) ) ;
#16709 = FACE_OUTER_BOUND ( 'NONE', #18834, .T. ) ;
#16710 = ORIENTED_EDGE ( 'NONE', *, *, #10067, .F. ) ;
#16711 = CIRCLE ( 'NONE', #16060, 0.1000000000000028644 ) ;
#16712 = CARTESIAN_POINT ( 'NONE',  ( -61.24591834330252027, -42.37473357531882812, -2.500000000000000000 ) ) ;
#16713 = DIRECTION ( 'NONE',  ( 0.4582725098355735494, -0.8888117386314181578, 0.000000000000000000 ) ) ;
#16714 = CARTESIAN_POINT ( 'NONE',  ( 23.22017056567068494, 3.363622401179964250, 3.779250300422446696 ) ) ;
#16715 = CARTESIAN_POINT ( 'NONE',  ( 0.9049783971971742114, -32.87558106357499810, 6.939395833800440450 ) ) ;
#16716 = CARTESIAN_POINT ( 'NONE',  ( 0.4482788600987206995, -32.83830765075952485, 6.873189335546979528 ) ) ;
#16718 = EDGE_CURVE ( 'NONE', #21616, #35240, #14710, .T. ) ;
#16717 = CARTESIAN_POINT ( 'NONE',  ( -55.39244940828790220, 31.07786128219255062, 1.730094348643131941 ) ) ;
#16719 = ORIENTED_EDGE ( 'NONE', *, *, #31118, .T. ) ;
#16720 = CARTESIAN_POINT ( 'NONE',  ( 22.87850294736509582, 4.337130434239091947, 3.058172268432443275 ) ) ;
#16721 = EDGE_CURVE ( 'NONE', #17641, #14737, #38648, .T. ) ;
#16722 = DIRECTION ( 'NONE',  ( -0.000000000000000000, 1.000000000000000000, -0.000000000000000000 ) ) ;
#16723 = CARTESIAN_POINT ( 'NONE',  ( 81.11573943753921867, 62.50280337846361789, 3.122598816540627542 ) ) ;
#16724 = EDGE_CURVE ( 'NONE', #29197, #27494, #7462, .T. ) ;
#16725 = DIRECTION ( 'NONE',  ( 1.000000000000000000, 0.000000000000000000, 0.000000000000000000 ) ) ;
#16726 = ORIENTED_EDGE ( 'NONE', *, *, #29784, .T. ) ;
#16727 = CARTESIAN_POINT ( 'NONE',  ( 78.15789273364713097, 65.21536350427231810, -2.660685394430948314 ) ) ;
#16729 = CARTESIAN_POINT ( 'NONE',  ( -0.4747269484695719743, -32.18314005917732601, 7.635761828346577573 ) ) ;
#16728 = CARTESIAN_POINT ( 'NONE',  ( 21.98532980874193399, 0.2335280526894900899, 7.692103986081960443 ) ) ;
#16730 = CARTESIAN_POINT ( 'NONE',  ( 81.53866496495169258, 61.91358381440836922, -2.246767365022170893 ) ) ;
#16731 =( BOUNDED_CURVE ( )  B_SPLINE_CURVE ( 3, ( #18379, #27450, #24153, #24566 ),
 .UNSPECIFIED., .F., .T. ) 
 B_SPLINE_CURVE_WITH_KNOTS ( ( 4, 4 ),
 ( 4.886921905584129533, 4.895802057644188743 ),
 .UNSPECIFIED. ) 
 CURVE ( )  GEOMETRIC_REPRESENTATION_ITEM ( )  RATIONAL_B_SPLINE_CURVE ( ( 1.000000000000000000, 0.9999934285857451366, 0.9999934285857451366, 1.000000000000000000 ) ) 
 REPRESENTATION_ITEM ( '' )  );
#16732 = CARTESIAN_POINT ( 'NONE',  ( 78.15789273364713097, 65.21536350427231810, 2.660685394430948314 ) ) ;
#16733 = ORIENTED_EDGE ( 'NONE', *, *, #24147, .T. ) ;
#16734 = LINE ( 'NONE', #10160, #1738 ) ;
#16735 = CARTESIAN_POINT ( 'NONE',  ( 81.96779975749585390, 61.96402392828839822, 1.065376284871803581 ) ) ;
#16737 = ORIENTED_EDGE ( 'NONE', *, *, #4744, .T. ) ;
#16736 = CARTESIAN_POINT ( 'NONE',  ( -63.44067635386505088, 42.93380570789835105, 3.509169995953163035 ) ) ;
#16738 = ADVANCED_FACE ( 'NONE', ( #16709, #29300 ), #13644, .F. ) ;
#16739 = CARTESIAN_POINT ( 'NONE',  ( 22.80834877297060004, -6.429644848144123515, 3.896382617761176892 ) ) ;
#16740 = CARTESIAN_POINT ( 'NONE',  ( -64.20341131561860948, 34.94420666461578406, -4.877756629158676027 ) ) ;
#16741 = ORIENTED_EDGE ( 'NONE', *, *, #23351, .F. ) ;
#16742 = CARTESIAN_POINT ( 'NONE',  ( -81.10044192579809419, -5.650254496098106038, 4.158657536701277913 ) ) ;
#16743 = CARTESIAN_POINT ( 'NONE',  ( -0.8809027425463855643, -31.78283038357269419, 7.695279973900954751 ) ) ;
#16744 = DIRECTION ( 'NONE',  ( 1.000000000000000000, 0.000000000000000000, 0.000000000000000000 ) ) ;
#16745 = VECTOR ( 'NONE', #39020, 1000.000000000000227 ) ;
#16746 = B_SPLINE_CURVE_WITH_KNOTS ( 'NONE', 3,
 ( #18683, #31268, #9835, #6951 ),
 .UNSPECIFIED., .F., .F.,
 ( 4, 4 ),
 ( 8.335636658244670956E-05, 0.008874052763743587799 ),
 .UNSPECIFIED. ) ;
#16747 = DIRECTION ( 'NONE',  ( 0.000000000000000000, 1.000000000000000000, 0.000000000000000000 ) ) ;
#16748 = VERTEX_POINT ( 'NONE', #32600 ) ;
#16749 = CARTESIAN_POINT ( 'NONE',  ( 33.45650472609418102, -3.831704090213303715, -5.091214335412847625 ) ) ;
#16750 = CARTESIAN_POINT ( 'NONE',  ( 30.71467839345701023, -3.288362829192787107, -4.965898286879354195 ) ) ;
#16751 = AXIS2_PLACEMENT_3D ( 'NONE', #10130, #22717, #34887 ) ;
#16752 = CARTESIAN_POINT ( 'NONE',  ( 3.349526715458713610, -32.65705642007926457, 6.865482280155368322 ) ) ;
#16753 = CARTESIAN_POINT ( 'NONE',  ( 5.109224889810624504, -30.36356686813360994, 6.931070083220555844 ) ) ;
#16754 = CYLINDRICAL_SURFACE ( 'NONE', #27832, 0.09010775117053204664 ) ;
#16755 = CARTESIAN_POINT ( 'NONE',  ( -0.7727839574033206205, -27.22657253935856048, 7.386948897581452123 ) ) ;
#16756 = CARTESIAN_POINT ( 'NONE',  ( -40.24874870218063450, -26.64985754041175525, 6.700000000000000178 ) ) ;
#16757 = VECTOR ( 'NONE', #38001, 1000.000000000000000 ) ;
#16758 = CARTESIAN_POINT ( 'NONE',  ( 4.740160921379847458, -31.30480577326951064, 7.750000000000000000 ) ) ;
#16759 = CARTESIAN_POINT ( 'NONE',  ( -1.265720463714046895, -27.71192368072266277, 7.750000000000000888 ) ) ;
#16760 = VERTEX_POINT ( 'NONE', #4398 ) ;
#16761 = VERTEX_POINT ( 'NONE', #29500 ) ;
#16762 = CARTESIAN_POINT ( 'NONE',  ( 66.69400287465482791, 57.94980623640483230, 3.999076693785756031 ) ) ;
#16763 = B_SPLINE_CURVE_WITH_KNOTS ( 'NONE', 3,
 ( #22359, #37972, #16159, #22557 ),
 .UNSPECIFIED., .F., .F.,
 ( 4, 4 ),
 ( 2.168404344971008868E-19, 6.391136169993524662E-06 ),
 .UNSPECIFIED. ) ;
#16764 = CARTESIAN_POINT ( 'NONE',  ( 2.287364877874435987, -26.11950075324752518, 7.744938106820261403 ) ) ;
#16765 = CARTESIAN_POINT ( 'NONE',  ( 84.25787434187677150, 2.991901652185509075, -1.300773176381055940 ) ) ;
#16766 = CARTESIAN_POINT ( 'NONE',  ( -16.44874870218064089, -26.64985754041175525, 6.700000000000000178 ) ) ;
#16767 = ORIENTED_EDGE ( 'NONE', *, *, #2109, .T. ) ;
#16768 = CARTESIAN_POINT ( 'NONE',  ( -81.82309097574839996, 10.46037581310753772, 0.2594491973369116300 ) ) ;
#16769 =( NAMED_UNIT ( * ) SI_UNIT ( $, .STERADIAN. ) SOLID_ANGLE_UNIT ( ) );
#16770 = CARTESIAN_POINT ( 'NONE',  ( -83.92837670882109080, 2.429809908903242999, 12.50000000000000000 ) ) ;
#16771 = CARTESIAN_POINT ( 'NONE',  ( -70.92837670882107659, 15.04836564048558500, 0.000000000000000000 ) ) ;
#16772 = ORIENTED_EDGE ( 'NONE', *, *, #33535, .T. ) ;
#16773 = EDGE_CURVE ( 'NONE', #17495, #11431, #15105, .T. ) ;
#16774 = CARTESIAN_POINT ( 'NONE',  ( -70.92837670882107659, -23.80776546975053520, 10.00000000000000888 ) ) ;
#16775 = AXIS2_PLACEMENT_3D ( 'NONE', #29827, #26749, #11076 ) ;
#16776 = VECTOR ( 'NONE', #10453, 1000.000000000000114 ) ;
#16777 = EDGE_CURVE ( 'NONE', #9686, #25800, #37730, .T. ) ;
#16778 = ORIENTED_EDGE ( 'NONE', *, *, #29344, .T. ) ;
#16779 = CARTESIAN_POINT ( 'NONE',  ( 80.48897389181450990, 62.29924170813984574, -3.301258712451521138 ) ) ;
#16780 = CARTESIAN_POINT ( 'NONE',  ( 79.64740672574815505, 64.24900652125759848, 3.657510014241685425 ) ) ;
#16782 = ORIENTED_EDGE ( 'NONE', *, *, #32161, .T. ) ;
#16781 = CARTESIAN_POINT ( 'NONE',  ( -1.699609906766908818, -29.56993018339339940, 7.222147233343546802 ) ) ;
#16783 = CARTESIAN_POINT ( 'NONE',  ( 26.91783537306902119, 1.348898915238470497, 4.407577238912754325 ) ) ;
#16784 = DIRECTION ( 'NONE',  ( -0.4999999999999918954, -0.8660254037844432595, -0.000000000000000000 ) ) ;
#16785 = CARTESIAN_POINT ( 'NONE',  ( -2.619165735930222727, -32.12635497920775407, 7.695279973900954751 ) ) ;
#16786 = CARTESIAN_POINT ( 'NONE',  ( 21.85643539959776760, 9.535790418011023561, -9.299971273199719946 ) ) ;
#16787 = DIRECTION ( 'NONE',  ( -0.000000000000000000, 0.000000000000000000, 1.000000000000000000 ) ) ;
#16788 = VERTEX_POINT ( 'NONE', #40169 ) ;
#16789 = DIRECTION ( 'NONE',  ( -1.000000000000000000, 0.000000000000000000, -0.000000000000000000 ) ) ;
#16790 = ORIENTED_EDGE ( 'NONE', *, *, #25313, .T. ) ;
#16791 = CARTESIAN_POINT ( 'NONE',  ( -0.5438121010353070828, -32.25394735576643512, 7.762796336881262249 ) ) ;
#16792 = CARTESIAN_POINT ( 'NONE',  ( -74.17935931525508408, -3.991321171111944732, -9.458026139773300756 ) ) ;
#16793 = CARTESIAN_POINT ( 'NONE',  ( -0.02825552051704444470, -26.64216676595851396, 7.670860738520325128 ) ) ;
#16794 = DIRECTION ( 'NONE',  ( -0.000000000000000000, -0.000000000000000000, -1.000000000000000000 ) ) ;
#16795 = CARTESIAN_POINT ( 'NONE',  ( 81.36407395805154863, 61.67455102447422632, 2.043563575549261824 ) ) ;
#16796 = LINE ( 'NONE', #30178, #15027 ) ;
#16797 = CARTESIAN_POINT ( 'NONE',  ( 3.924182654612999421, -26.99799553805268459, 7.785868773668303433 ) ) ;
#16798 = CARTESIAN_POINT ( 'NONE',  ( -1.576080553448099719, -30.80067796904879884, 7.698786668945008849 ) ) ;
#16799 = B_SPLINE_CURVE_WITH_KNOTS ( 'NONE', 3,
 ( #27244, #33653, #27453, #8703, #24362, #21746, #24620, #37380, #40059, #37776, #3250, #28325, #15144, #31425, #21134, #33701, #12259, #15559, #36974, #27703, #40256, #15768, #21549, #31221, #30613, #140, #3041, #12671, #2625, #21956, #8754, #5480, #14942, #15350, #9372, #18023, #30819, #40450, #11838, #2419, #28116, #18636, #21338, #2829, #24833, #33910, #34530, #25246, #5688, #6099, #40669, #12473, #27508, #34329, #24417, #18230, #6303, #25042, #12042, #9174, #5895, #34125, #37174, #18852, #18433, #8959, #31021, #27906, #37576 ),
 .UNSPECIFIED., .F., .F.,
 ( 4, 2, 2, 1, 1, 1, 1, 1, 2, 2, 2, 1, 1, 1, 1, 1, 2, 2, 2, 2, 1, 1, 1, 1, 1, 2, 2, 1, 2, 2, 1, 1, 2, 1, 2, 2, 2, 1, 2, 2, 2, 1, 2, 2, 4 ),
 ( 0.000000000000000000, 0.1250000000000453804, 0.1875000000000680567, 0.2187500000000786871, 0.2343750000000833222, 0.2421875000000850153, 0.2460937500000858480, 0.2480468750000862643, 0.2490234375000858480, 0.2500000000000854317, 0.3750000000001176281, 0.4375000000001337264, 0.4687500000001417755, 0.4843750000001458278, 0.4921875000001487144, 0.4960937500001492695, 0.4980468750001496581, 0.5000000000001499911, 0.6250000000002199352, 0.6875000000002549072, 0.7187500000002723377, 0.7343750000002787770, 0.7421875000002816636, 0.7460937500002862155, 0.7480468750002851053, 0.7490234375002847722, 0.7500000000002845502, 0.7812500000002576828, 0.7968750000002441380, 0.8007812500002396972, 0.8046875000002351452, 0.8125000000002252643, 0.8437500000001855183, 0.8593750000001656453, 0.8671875000001554312, 0.8750000000001451061, 0.8906250000001246780, 0.8984375000001154632, 0.9023437500001109113, 0.9062500000001062483, 0.9218750000000908162, 0.9296875000000820455, 0.9335937500000766054, 0.9375000000000711653, 1.000000000000000000 ),
 .UNSPECIFIED. ) ;
#16800 = DIRECTION ( 'NONE',  ( 0.9848077530122103518, -0.1736481776669172583, -0.000000000000000000 ) ) ;
#16801 = CARTESIAN_POINT ( 'NONE',  ( 33.61621798268036798, -1.223546897810831480, 5.453021846138203621 ) ) ;
#16802 = ADVANCED_FACE ( 'NONE', ( #33613 ), #4984, .F. ) ;
#16803 = AXIS2_PLACEMENT_3D ( 'NONE', #7546, #38427, #7345 ) ;
#16804 = AXIS2_PLACEMENT_3D ( 'NONE', #13043, #28698, #3607 ) ;
#16805 = CARTESIAN_POINT ( 'NONE',  ( -64.08758708074093136, 40.20283945498818667, -3.000000000000000000 ) ) ;
#16806 = LINE ( 'NONE', #16216, #29202 ) ;
#16807 = DIRECTION ( 'NONE',  ( 1.000000000000000000, 0.000000000000000000, 0.000000000000000000 ) ) ;
#16808 =( BOUNDED_CURVE ( )  B_SPLINE_CURVE ( 3, ( #17626, #36384, #24434, #18040 ),
 .UNSPECIFIED., .F., .T. ) 
 B_SPLINE_CURVE_WITH_KNOTS ( ( 4, 4 ),
 ( 1.381924640371167579, 1.570796326794896780 ),
 .UNSPECIFIED. ) 
 CURVE ( )  GEOMETRIC_REPRESENTATION_ITEM ( )  RATIONAL_B_SPLINE_CURVE ( ( 1.000000000000000000, 0.9970294990994144069, 0.9970294990994144069, 1.000000000000000000 ) ) 
 REPRESENTATION_ITEM ( '' )  );
#16809 = CARTESIAN_POINT ( 'NONE',  ( 4.921324086407802056, -26.64985754041175525, 6.700000000000000178 ) ) ;
#16810 = ORIENTED_EDGE ( 'NONE', *, *, #37601, .F. ) ;
#16811 = CARTESIAN_POINT ( 'NONE',  ( 36.14170422902504498, -3.144485308923159028, 5.847185053995919368 ) ) ;
#16812 = AXIS2_PLACEMENT_3D ( 'NONE', #1137, #35318, #7084 ) ;
#16813 = EDGE_CURVE ( 'NONE', #1190, #1835, #2734, .T. ) ;
#16814 = DIRECTION ( 'NONE',  ( 0.000000000000000000, 0.000000000000000000, 1.000000000000000000 ) ) ;
#16815 = CARTESIAN_POINT ( 'NONE',  ( 87.43361094620441065, 0.1481429324132612357, -5.028924837761966415 ) ) ;
#16817 = CARTESIAN_POINT ( 'NONE',  ( -0.5068137670456340782, -26.85363654698906188, 6.875671892026065990 ) ) ;
#16816 = CARTESIAN_POINT ( 'NONE',  ( 79.61290006553410592, 65.30841326124827617, -3.134554000843263299 ) ) ;
#16818 = CARTESIAN_POINT ( 'NONE',  ( -1.246051523623666668, -27.68087481465684263, 6.887547729233689076 ) ) ;
#16819 = CARTESIAN_POINT ( 'NONE',  ( -56.76293260130698570, 30.10808691202729293, 4.002692287617911404 ) ) ;
#16820 = ORIENTED_EDGE ( 'NONE', *, *, #5875, .F. ) ;
#16821 = CARTESIAN_POINT ( 'NONE',  ( 1.277039614466915829, -32.95056463638093192, 7.139196562012274150 ) ) ;
#16822 = CARTESIAN_POINT ( 'NONE',  ( 23.06591706423118637, -8.086835649431872497, -2.500000000000005773 ) ) ;
#16823 = EDGE_LOOP ( 'NONE', ( #10195, #7463, #39364, #32220, #37390 ) ) ;
#16824 = VERTEX_POINT ( 'NONE', #18338 ) ;
#16825 = ADVANCED_FACE ( 'NONE', ( #30510, #11140 ), #14841, .T. ) ;
#16826 = CARTESIAN_POINT ( 'NONE',  ( 81.06761308752984974, 61.31222891353763771, -1.660510093083302108 ) ) ;
#16827 = DIRECTION ( 'NONE',  ( 0.000000000000000000, -0.000000000000000000, -1.000000000000000000 ) ) ;
#16828 = CARTESIAN_POINT ( 'NONE',  ( 80.33017967436602191, 63.51919597486899249, 3.679799701112133725 ) ) ;
#16829 = CARTESIAN_POINT ( 'NONE',  ( 22.09304849718642316, 0.3726161401571594922, 7.354740019033460641 ) ) ;
#16830 = VERTEX_POINT ( 'NONE', #27407 ) ;
#16831 = CARTESIAN_POINT ( 'NONE',  ( -0.05162664538871142295, -32.48376568794560626, 7.785172627573962778 ) ) ;
#16833 = CARTESIAN_POINT ( 'NONE',  ( 85.42670333274200800, 2.402396817435708876, 2.739882088504116631 ) ) ;
#16832 = CARTESIAN_POINT ( 'NONE',  ( -58.95184776849900743, 28.36361089872152519, -6.321022755279361860 ) ) ;
#16834 = CARTESIAN_POINT ( 'NONE',  ( -70.92837670882107659, 15.04836564048558500, 6.406751979251626317 ) ) ;
#16835 = CIRCLE ( 'NONE', #6439, 0.1000000000000028644 ) ;
#16836 = CARTESIAN_POINT ( 'NONE',  ( -64.08758708074407195, 44.09647857431092888, -1.198350469763766579 ) ) ;
#16837 =( NAMED_UNIT ( * ) SI_UNIT ( $, .STERADIAN. ) SOLID_ANGLE_UNIT ( ) );
#16838 = CARTESIAN_POINT ( 'NONE',  ( 21.96956884823482881, 4.963862418377736674, -3.595920138844930669 ) ) ;
#16839 = EDGE_LOOP ( 'NONE', ( #17788, #27158, #10014, #34587 ) ) ;
#16840 = CARTESIAN_POINT ( 'NONE',  ( 78.69038500580363404, 66.05859403932464602, -1.000000000000000000 ) ) ;
#16841 = VERTEX_POINT ( 'NONE', #39553 ) ;
#16842 = EDGE_CURVE ( 'NONE', #23233, #17714, #37825, .T. ) ;
#16843 = CARTESIAN_POINT ( 'NONE',  ( 21.85643539959778536, -8.233350057040109249, -11.92691213149646678 ) ) ;
#16844 = CARTESIAN_POINT ( 'NONE',  ( 21.86257038566819588, 3.862145465818127121, -3.386728275810359623 ) ) ;
#16845 = CARTESIAN_POINT ( 'NONE',  ( -69.08758708074091714, 24.84364830758654108, 8.800414904976364028 ) ) ;
#16846 = CARTESIAN_POINT ( 'NONE',  ( 79.73441168748210828, 65.96538777703865719, 2.410848004515915743 ) ) ;
#16847 = CARTESIAN_POINT ( 'NONE',  ( 85.85116863490735284, 1.861966474136578231, -4.950709030323501736 ) ) ;
#16848 = CARTESIAN_POINT ( 'NONE',  ( -75.45330471031414277, 33.71485196875532608, 12.50000000000000000 ) ) ;
#16849 = ORIENTED_EDGE ( 'NONE', *, *, #8027, .T. ) ;
#16850 = CARTESIAN_POINT ( 'NONE',  ( -78.42754742544201463, -5.260774960203544737, 8.337059064591437973 ) ) ;
#16851 = ORIENTED_EDGE ( 'NONE', *, *, #4310, .T. ) ;
#16852 = CARTESIAN_POINT ( 'NONE',  ( 14.82083291377484358, -6.154340523497400461, 2.519547438029839270 ) ) ;
#16853 = CARTESIAN_POINT ( 'NONE',  ( 32.63305097123843979, -3.795354871036205058, 4.923932146436776236 ) ) ;
#16854 = CARTESIAN_POINT ( 'NONE',  ( 14.64249155491722831, -5.613241577028397877, -2.491712955778045746 ) ) ;
#16855 = CARTESIAN_POINT ( 'NONE',  ( 34.13628169468366735, -3.131472990218530317, -5.534190366183364240 ) ) ;
#16856 = CARTESIAN_POINT ( 'NONE',  ( -0.06469087068677582819, -26.54759843608177761, 7.750000000000000888 ) ) ;
#16857 = CARTESIAN_POINT ( 'NONE',  ( 5.152478333118308385, -28.99279347164636889, 6.894806418505347700 ) ) ;
#16858 = EDGE_CURVE ( 'NONE', #1323, #36841, #39110, .T. ) ;
#16859 = CARTESIAN_POINT ( 'NONE',  ( -24.34874870218063592, -25.49307895267003587, 6.800000000000000711 ) ) ;
#16860 = DIRECTION ( 'NONE',  ( 0.000000000000000000, -1.000000000000000000, -1.147978770867004622E-16 ) ) ;
#16861 = EDGE_CURVE ( 'NONE', #21048, #18658, #23710, .T. ) ;
#16862 = CARTESIAN_POINT ( 'NONE',  ( -1.642747097704066128, -30.18915717881909444, 7.730758795053805699 ) ) ;
#16863 = CARTESIAN_POINT ( 'NONE',  ( 4.983308922979784228, -28.35648716565642857, 7.750000000000000000 ) ) ;
#16864 = ORIENTED_EDGE ( 'NONE', *, *, #27472, .T. ) ;
#16865 = ORIENTED_EDGE ( 'NONE', *, *, #32551, .T. ) ;
#16866 = CARTESIAN_POINT ( 'NONE',  ( 37.21169332916825567, -2.743835684017817744, 6.000896651629099132 ) ) ;
#16867 = CARTESIAN_POINT ( 'NONE',  ( -0.5374033828380346822, -32.26107951187057665, 7.638132480492516585 ) ) ;
#16868 = COLOUR_RGB ( '',0.7921568627450980005, 0.8196078431372548767, 0.9333333333333333481 ) ;
#16869 = CARTESIAN_POINT ( 'NONE',  ( 66.27376694609004915, 57.73522568913436004, -4.000000000000000000 ) ) ;
#16870 = AXIS2_PLACEMENT_3D ( 'NONE', #26790, #13617, #4961 ) ;
#16871 = CARTESIAN_POINT ( 'NONE',  ( 86.88453911838293209, -1.192694612346317573, 5.156246139204053947 ) ) ;
#16872 = AXIS2_PLACEMENT_3D ( 'NONE', #13123, #25682, #10022 ) ;
#16873 = ORIENTED_EDGE ( 'NONE', *, *, #27737, .F. ) ;
#16874 = CARTESIAN_POINT ( 'NONE',  ( 4.914263057417876723, -28.46041651962800501, 6.887041543973313473 ) ) ;
#16875 = EDGE_CURVE ( 'NONE', #22837, #39470, #1355, .T. ) ;
#16876 =( NAMED_UNIT ( * ) PLANE_ANGLE_UNIT ( ) SI_UNIT ( $, .RADIAN. ) );
#16877 = CARTESIAN_POINT ( 'NONE',  ( 1.700390093233090871, -29.56993018339339940, -6.000000000000000000 ) ) ;
#16878 = CARTESIAN_POINT ( 'NONE',  ( 3.860546469805519187, -32.32378646663576660, 6.865482280155369210 ) ) ;
#16879 = ORIENTED_EDGE ( 'NONE', *, *, #10559, .F. ) ;
#16880 = CARTESIAN_POINT ( 'NONE',  ( 80.56094004998607261, 66.12977872868212614, -1.831286414254869266 ) ) ;
#16881 = CARTESIAN_POINT ( 'NONE',  ( 14.66962918947518979, -4.461995682952458964, -2.500000000000003553 ) ) ;
#16882 = ORIENTED_EDGE ( 'NONE', *, *, #27126, .T. ) ;
#16883 = CARTESIAN_POINT ( 'NONE',  ( 75.30130074865812162, 63.36357894040063599, -3.230144225280407344 ) ) ;
#16885 = FACE_OUTER_BOUND ( 'NONE', #2220, .T. ) ;
#16884 = CARTESIAN_POINT ( 'NONE',  ( 2.474049714983521664, -26.15650803111381606, 7.013842709614101167 ) ) ;
#16886 = CARTESIAN_POINT ( 'NONE',  ( -70.42518435975088664, 0.09082038125507381487, 5.980078429000515783 ) ) ;
#16887 = CARTESIAN_POINT ( 'NONE',  ( 77.66280895473884982, 61.33468559051788560, 3.643081266330365331 ) ) ;
#16888 = CARTESIAN_POINT ( 'NONE',  ( 22.72845964424274001, 2.421760147549044895, -4.797409384227349527 ) ) ;
#16889 = PLANE ( 'NONE',  #18176 ) ;
#16890 = EDGE_CURVE ( 'NONE', #19590, #38247, #21978, .T. ) ;
#16891 = AXIS2_PLACEMENT_3D ( 'NONE', #36758, #24198, #17389 ) ;
#16892 = CARTESIAN_POINT ( 'NONE',  ( -30.34874870218063947, -26.64985754041175525, 6.700000000000000178 ) ) ;
#16893 = FACE_OUTER_BOUND ( 'NONE', #25688, .T. ) ;
#16894 = CARTESIAN_POINT ( 'NONE',  ( 1.669512530038368414, -26.07006638945924948, 7.665454363767879364 ) ) ;
#16895 = CARTESIAN_POINT ( 'NONE',  ( 81.66247121191638314, 61.65231731326593234, 1.378120381825652219 ) ) ;
#16896 = CARTESIAN_POINT ( 'NONE',  ( -0.2112746087012261631, -32.50174735455220798, 6.931070083220562061 ) ) ;
#16897 = CARTESIAN_POINT ( 'NONE',  ( 30.37020714367901775, -0.1410433206546675144, -5.583699017444894608 ) ) ;
#16898 = AXIS2_PLACEMENT_3D ( 'NONE', #8104, #11797, #14493 ) ;
#16899 = CARTESIAN_POINT ( 'NONE',  ( 2.330147284786646456, -26.22874769739361511, 7.784838882742139532 ) ) ;
#16900 = AXIS2_PLACEMENT_3D ( 'NONE', #21888, #27646, #3188 ) ;
#16901 = CARTESIAN_POINT ( 'NONE',  ( -36.24874870218063450, -26.64985754041175525, 6.700000000000000178 ) ) ;
#16902 = AXIS2_PLACEMENT_3D ( 'NONE', #17724, #39354, #3104 ) ;
#16903 = DIRECTION ( 'NONE',  ( 0.7660444431189790127, 0.6427876096865381417, 0.000000000000000000 ) ) ;
#16904 = ORIENTED_EDGE ( 'NONE', *, *, #26958, .F. ) ;
#16905 = PLANE ( 'NONE',  #40192 ) ;
#16906 = FACE_OUTER_BOUND ( 'NONE', #13327, .T. ) ;
#16907 = EDGE_CURVE ( 'NONE', #22737, #5985, #33195, .T. ) ;
#16908 = CARTESIAN_POINT ( 'NONE',  ( 31.78482901221541823, -0.3652494130366964464, -5.167189304987498844 ) ) ;
#16909 = DIRECTION ( 'NONE',  ( 0.9267318687906771491, -0.3757233601570964532, 0.000000000000000000 ) ) ;
#16910 = CARTESIAN_POINT ( 'NONE',  ( 4.693750549451069176, -31.38373704560598654, 6.867280401193709416 ) ) ;
#16911 = CARTESIAN_POINT ( 'NONE',  ( -1.799476894543866612, -29.60054653561284965, 7.727461116072927183 ) ) ;
#16912 = CARTESIAN_POINT ( 'NONE',  ( 2.242723711017451382, -32.92639770848892766, 6.894806418505347700 ) ) ;
#16913 = ADVANCED_FACE ( 'NONE', ( #8249 ), #8662, .F. ) ;
#16914 = DIRECTION ( 'NONE',  ( -0.000000000000000000, -0.000000000000000000, 1.000000000000000000 ) ) ;
#16915 = ORIENTED_EDGE ( 'NONE', *, *, #4349, .T. ) ;
#16916 = CARTESIAN_POINT ( 'NONE',  ( 33.44586992423308658, -3.711826566333543909, 5.220901829495124602 ) ) ;
#16917 = CYLINDRICAL_SURFACE ( 'NONE', #25136, 3.399999999999999911 ) ;
#16918 = CARTESIAN_POINT ( 'NONE',  ( 67.36017643331848603, 58.39563743223260417, -3.987264345885670913 ) ) ;
#16919 = CARTESIAN_POINT ( 'NONE',  ( 4.723655388576528225, -27.80644746340955464, 7.638132480492515697 ) ) ;
#16920 = ORIENTED_EDGE ( 'NONE', *, *, #13622, .F. ) ;
#16921 = CYLINDRICAL_SURFACE ( 'NONE', #25943, 0.09010775117052932659 ) ;
#16922 = CARTESIAN_POINT ( 'NONE',  ( 5.067143666762728316, -33.49802700238250708, 7.695279973900954751 ) ) ;
#16923 = CARTESIAN_POINT ( 'NONE',  ( 85.65342632314096250, 0.8846110238782115553, -5.852385830138683076 ) ) ;
#16924 = CARTESIAN_POINT ( 'NONE',  ( 0.9038683196620087568, -32.87531266959080511, 6.949473656533217358 ) ) ;
#16925 =( BOUNDED_CURVE ( )  B_SPLINE_CURVE ( 3, ( #25089, #9417, #38037, #40716 ),
 .UNSPECIFIED., .F., .F. ) 
 B_SPLINE_CURVE_WITH_KNOTS ( ( 4, 4 ),
 ( 1.347909859412852907, 1.534781240595298080 ),
 .UNSPECIFIED. ) 
 CURVE ( )  GEOMETRIC_REPRESENTATION_ITEM ( )  RATIONAL_B_SPLINE_CURVE ( ( 1.000000000000000000, 0.9970920404276226723, 0.9970920404276226723, 1.000000000000000000 ) ) 
 REPRESENTATION_ITEM ( '' )  );
#16926 = AXIS2_PLACEMENT_3D ( 'NONE', #15974, #9800, #16377 ) ;
#16927 = CARTESIAN_POINT ( 'NONE',  ( 3.594851464545667952, -26.62696974998548782, 7.013842709614101167 ) ) ;
#16928 = CIRCLE ( 'NONE', #2512, 0.1000000000000028644 ) ;
#16929 = FACE_OUTER_BOUND ( 'NONE', #9563, .T. ) ;
#16930 = EDGE_LOOP ( 'NONE', ( #32550, #37840 ) ) ;
#16931 = CARTESIAN_POINT ( 'NONE',  ( 22.38745053706796284, 4.913031730865500712, 3.072246906157164670 ) ) ;
#16932 = DIRECTION ( 'NONE',  ( 1.000000000000000000, -6.367278819747329048E-17, 0.000000000000000000 ) ) ;
#16933 = CARTESIAN_POINT ( 'NONE',  ( 17.95234582529949563, -3.169824730388413947, 2.966045911591449702 ) ) ;
#16934 = CARTESIAN_POINT ( 'NONE',  ( 79.99568124201523744, 64.83088095446822763, 3.420541042474579907 ) ) ;
#16935 = LINE ( 'NONE', #17326, #13377 ) ;
#16936 = EDGE_LOOP ( 'NONE', ( #23089, #13782, #29001, #31458 ) ) ;
#16937 = CARTESIAN_POINT ( 'NONE',  ( 78.24346468842466606, 65.07400588416957987, -2.889371261047450457 ) ) ;
#16939 = CARTESIAN_POINT ( 'NONE',  ( -1.656886121102593368, -30.10724210791205380, 6.889465824494254598 ) ) ;
#16938 = CARTESIAN_POINT ( 'NONE',  ( 21.73454763666067890, 0.2393990557980432143, 9.044420270734587319 ) ) ;
#16940 = CARTESIAN_POINT ( 'NONE',  ( 80.71310200138587732, 64.86488640221421065, -3.283621700554756995 ) ) ;
#16941 = CARTESIAN_POINT ( 'NONE',  ( 80.55759259636404579, 61.16327383424329156, 2.033355767895909327 ) ) ;
#16942 = DIRECTION ( 'NONE',  ( -0.8660254037844271613, 0.5000000000000200950, 0.000000000000000000 ) ) ;
#16943 = CARTESIAN_POINT ( 'NONE',  ( 81.96245566837731644, 61.96131850323958901, 1.129532193886028102 ) ) ;
#16945 = VERTEX_POINT ( 'NONE', #15053 ) ;
#16944 = CARTESIAN_POINT ( 'NONE',  ( -71.72837670882105954, -34.30579396504363388, 1.385640646055090519 ) ) ;
#16946 = CIRCLE ( 'NONE', #7754, 12.38600677260393113 ) ;
#16947 = CARTESIAN_POINT ( 'NONE',  ( 28.10206848396558499, 1.736549293047330300, -3.980455106513370200 ) ) ;
#16948 = CARTESIAN_POINT ( 'NONE',  ( -64.29080678322935682, 36.57451004496367375, -5.531098403533436070 ) ) ;
#16949 = ORIENTED_EDGE ( 'NONE', *, *, #10112, .T. ) ;
#16950 = CARTESIAN_POINT ( 'NONE',  ( -73.25244780539486555, -2.789250568390547080, 9.729507352929793740 ) ) ;
#16951 = CARTESIAN_POINT ( 'NONE',  ( 24.74342160786476086, 0.5916730990911962529, -4.777714225875230980 ) ) ;
#16952 = ADVANCED_FACE ( 'NONE', ( #27611 ), #33416, .F. ) ;
#16953 = DIRECTION ( 'NONE',  ( -1.000000000000000000, 0.000000000000000000, 0.000000000000000000 ) ) ;
#16954 = CIRCLE ( 'NONE', #5774, 0.04999999999999991257 ) ;
#16955 = CARTESIAN_POINT ( 'NONE',  ( 24.57142899942570224, 3.461735479277903149, 1.987691357384508528 ) ) ;
#16956 = EDGE_CURVE ( 'NONE', #39349, #10538, #14129, .T. ) ;
#16957 = VERTEX_POINT ( 'NONE', #27205 ) ;
#16958 = CARTESIAN_POINT ( 'NONE',  ( 36.44525044284685578, -1.732523961244382571, -5.730839696777302983 ) ) ;
#16959 = FACE_OUTER_BOUND ( 'NONE', #26658, .T. ) ;
#16960 = CARTESIAN_POINT ( 'NONE',  ( 1.651251297819358754, -26.64985754041175525, 6.700000000000000178 ) ) ;
#16961 = CARTESIAN_POINT ( 'NONE',  ( 5.108889948331447606, -30.36500087965021422, 6.971170733404099984 ) ) ;
#16962 = LINE ( 'NONE', #29538, #5477 ) ;
#16963 = CARTESIAN_POINT ( 'NONE',  ( 30.15929301752064973, -3.700805759990258181, 4.595697454274616511 ) ) ;
#16964 = AXIS2_PLACEMENT_3D ( 'NONE', #14749, #12284, #18878 ) ;
#16965 = EDGE_CURVE ( 'NONE', #25596, #34797, #35760, .T. ) ;
#16966 = DIRECTION ( 'NONE',  ( 0.000000000000000000, 1.000000000000000000, 0.000000000000000000 ) ) ;
#16967 = EDGE_CURVE ( 'NONE', #16635, #9241, #17225, .T. ) ;
#16968 = ORIENTED_EDGE ( 'NONE', *, *, #6880, .T. ) ;
#16969 = EDGE_LOOP ( 'NONE', ( #29156, #253, #38278, #2882 ) ) ;
#16970 = CARTESIAN_POINT ( 'NONE',  ( 66.71166677010936041, 57.90060579507158423, 3.999756211082797996 ) ) ;
#16971 = CARTESIAN_POINT ( 'NONE',  ( 71.10141846075379135, 59.08792130574165924, -3.942344351592514951 ) ) ;
#16972 = CARTESIAN_POINT ( 'NONE',  ( 2.276779695690628547, -26.11771647328293255, 7.724038915126859806 ) ) ;
#16973 = CARTESIAN_POINT ( 'NONE',  ( 84.21365554304541945, 2.879787869890822360, 1.939519519617897592 ) ) ;
#16974 = LINE ( 'NONE', #14692, #28770 ) ;
#16975 = AXIS2_PLACEMENT_3D ( 'NONE', #11466, #24033, #33541 ) ;
#16976 = DIRECTION ( 'NONE',  ( -1.000000000000000000, 0.000000000000000000, 0.000000000000000000 ) ) ;
#16977 = DIRECTION ( 'NONE',  ( 1.000000000000000000, 0.000000000000000000, 0.000000000000000000 ) ) ;
#16978 = DIRECTION ( 'NONE',  ( 0.000000000000000000, -0.6834397476448842434, 0.7300069255418724090 ) ) ;
#16979 = CARTESIAN_POINT ( 'NONE',  ( 1.137856487652708637, -26.12999894468477535, 7.785096263473212375 ) ) ;
#16980 = FACE_OUTER_BOUND ( 'NONE', #33335, .T. ) ;
#16981 = EDGE_LOOP ( 'NONE', ( #22340, #35351, #6680, #14645, #24135 ) ) ;
#16982 = CARTESIAN_POINT ( 'NONE',  ( 80.87649832867062116, 61.25867624111136678, -1.827177995460257387 ) ) ;
#16983 = CARTESIAN_POINT ( 'NONE',  ( 37.13838689045984154, -2.480252515904725730, 5.965224451857021215 ) ) ;
#16984 = CARTESIAN_POINT ( 'NONE',  ( 80.03393078220602774, 63.38059744715243937, 3.720735635808742447 ) ) ;
#16986 = ORIENTED_EDGE ( 'NONE', *, *, #35684, .T. ) ;
#16985 = CARTESIAN_POINT ( 'NONE',  ( -1.275819131918839666, -31.21377956460290548, 6.880147297696980857 ) ) ;
#16987 = CIRCLE ( 'NONE', #3235, 1.000000000000000000 ) ;
#16988 = CARTESIAN_POINT ( 'NONE',  ( -80.92837670882107659, 2.429809908903242555, 12.50000000000000000 ) ) ;
#16989 = FACE_OUTER_BOUND ( 'NONE', #29052, .T. ) ;
#16990 = CARTESIAN_POINT ( 'NONE',  ( -5.316495087772345585, -32.84709638682603838, 2.500000000000000000 ) ) ;
#16991 = ORIENTED_EDGE ( 'NONE', *, *, #2170, .T. ) ;
#16992 = DIRECTION ( 'NONE',  ( 0.000000000000000000, 0.000000000000000000, 1.000000000000000000 ) ) ;
#16993 = CARTESIAN_POINT ( 'NONE',  ( -16.44874870218064089, -25.49307895267003587, 6.700000000000000178 ) ) ;
#16994 = CARTESIAN_POINT ( 'NONE',  ( -72.89992789846300525, 1.434322839394358784, -10.95649126954176467 ) ) ;
#16995 = AXIS2_PLACEMENT_3D ( 'NONE', #30079, #14214, #2092 ) ;
#16996 = CARTESIAN_POINT ( 'NONE',  ( 5.144126537964561763, -28.94488408058296613, 7.640616322432098428 ) ) ;
#16997 = DIRECTION ( 'NONE',  ( 1.000000000000000000, 0.000000000000000000, -0.000000000000000000 ) ) ;
#16998 = CARTESIAN_POINT ( 'NONE',  ( 79.86111789578114895, 65.11834937465495443, 3.286127602909497014 ) ) ;
#16999 = LINE ( 'NONE', #39428, #22921 ) ;
#17000 = FACE_OUTER_BOUND ( 'NONE', #5988, .T. ) ;
#17001 = CARTESIAN_POINT ( 'NONE',  ( -1.278368187136755374, -27.75183824754000028, 7.780491323090174660 ) ) ;
#17002 = CARTESIAN_POINT ( 'NONE',  ( -64.85784325972055342, 34.81586596186931359, -6.466735817496061856 ) ) ;
#17003 = ADVANCED_FACE ( 'NONE', ( #1018 ), #35991, .F. ) ;
#17004 = DIRECTION ( 'NONE',  ( 1.000000000000000000, 0.000000000000000000, 0.000000000000000000 ) ) ;
#17005 = CARTESIAN_POINT ( 'NONE',  ( 17.27255596930787362, 8.732200699463135152, -2.902198115991937222 ) ) ;
#17006 = EDGE_CURVE ( 'NONE', #11338, #7017, #20321, .T. ) ;
#17007 = DIRECTION ( 'NONE',  ( 0.000000000000000000, -1.000000000000000000, 0.000000000000000000 ) ) ;
#17008 = CYLINDRICAL_SURFACE ( 'NONE', #32623, 0.1000000000000028644 ) ;
#17009 = CARTESIAN_POINT ( 'NONE',  ( 69.41850365747683327, 58.24027689931818230, 3.921432738910689331 ) ) ;
#17010 = CARTESIAN_POINT ( 'NONE',  ( 22.92029331350176946, 2.650804407416140318, 3.783664119596848785 ) ) ;
#17011 = CARTESIAN_POINT ( 'NONE',  ( -64.08758708074094557, 43.61223004741322740, -1.152033497945007978 ) ) ;
#17012 = CARTESIAN_POINT ( 'NONE',  ( 88.57583237253618336, -1.134854386742023546, -1.768762308819206375 ) ) ;
#17014 = CARTESIAN_POINT ( 'NONE',  ( -0.4435500636574273292, -26.80341516422506132, 6.870724624169666228 ) ) ;
#17013 = CARTESIAN_POINT ( 'NONE',  ( 79.92454992231405697, 64.78853304740056274, -3.443978770203974360 ) ) ;
#17015 = CARTESIAN_POINT ( 'NONE',  ( -1.242570340174825594, -27.67546881208082965, 7.013842709614101167 ) ) ;
#17016 = CARTESIAN_POINT ( 'NONE',  ( -57.86591918990971095, 28.88504657882484850, 4.653542815086530560 ) ) ;
#17017 = ORIENTED_EDGE ( 'NONE', *, *, #12595, .T. ) ;
#17018 = CARTESIAN_POINT ( 'NONE',  ( 1.062037487868057184, -32.90946697031814949, 6.894806418505346812 ) ) ;
#17019 = CARTESIAN_POINT ( 'NONE',  ( 7.121324086407810228, -24.55319635012989110, 6.700000000000000178 ) ) ;
#17020 = VERTEX_POINT ( 'NONE', #10850 ) ;
#17021 = CARTESIAN_POINT ( 'NONE',  ( -18.87867591359219333, -26.64985754041175525, 6.800000000000000711 ) ) ;
#17023 = ORIENTED_EDGE ( 'NONE', *, *, #19173, .F. ) ;
#17022 = ORIENTED_EDGE ( 'NONE', *, *, #22441, .T. ) ;
#17024 = ORIENTED_EDGE ( 'NONE', *, *, #8449, .F. ) ;
#17025 = CARTESIAN_POINT ( 'NONE',  ( 79.64490966524759585, 64.60885719387546544, -3.518158556798105963 ) ) ;
#17026 = LINE ( 'NONE', #22834, #35221 ) ;
#17027 = CARTESIAN_POINT ( 'NONE',  ( 81.09181894009961411, 61.27555711777438319, 1.268354304253239917 ) ) ;
#17028 = CARTESIAN_POINT ( 'NONE',  ( 23.58901020575210694, 0.9355507091876290593, 5.296862904573749198 ) ) ;
#17029 = ORIENTED_EDGE ( 'NONE', *, *, #31768, .T. ) ;
#17030 = CARTESIAN_POINT ( 'NONE',  ( -0.9352292415849461360, -31.71783863626873767, 6.894806418505345924 ) ) ;
#17031 = CARTESIAN_POINT ( 'NONE',  ( 59.69572451838116933, -0.8894979772356270686, 5.999999999999999112 ) ) ;
#17032 = DIRECTION ( 'NONE',  ( -0.000000000000000000, -0.000000000000000000, 1.000000000000000000 ) ) ;
#17033 = CARTESIAN_POINT ( 'NONE',  ( -64.08758708074093136, 43.38408792958330906, -2.770133712456854802 ) ) ;
#17034 = CARTESIAN_POINT ( 'NONE',  ( 23.42116204356915432, 3.682620607390830969, -3.312496470421961714 ) ) ;
#17035 = ORIENTED_EDGE ( 'NONE', *, *, #36241, .F. ) ;
#17036 = CARTESIAN_POINT ( 'NONE',  ( 5.123750824668761972, -30.29724448404768111, 7.754798119455333705 ) ) ;
#17037 = VECTOR ( 'NONE', #4224, 1000.000000000000000 ) ;
#17038 = CARTESIAN_POINT ( 'NONE',  ( 22.71767909661236118, -4.608197067329504293, -7.212190040765698917 ) ) ;
#17039 = CARTESIAN_POINT ( 'NONE',  ( 18.05491602130007678, 13.75800355181789847, -1.937621434240431872 ) ) ;
#17040 = CARTESIAN_POINT ( 'NONE',  ( 3.340113934647170435, -32.66206629357650115, 7.750000000000000888 ) ) ;
#17041 = ORIENTED_EDGE ( 'NONE', *, *, #39068, .T. ) ;
#17042 = CARTESIAN_POINT ( 'NONE',  ( 0.4844891494406461940, -32.74508134434379514, 6.887041543973317026 ) ) ;
#17043 = CARTESIAN_POINT ( 'NONE',  ( 81.59170830165204791, 62.44397035144425701, 2.684801069578921950 ) ) ;
#17044 = CARTESIAN_POINT ( 'NONE',  ( 88.66616934308579800, -1.912773240965560673, 2.173515562489431563 ) ) ;
#17045 =( BOUNDED_CURVE ( )  B_SPLINE_CURVE ( 3, ( #9732, #29486, #38529, #35279 ),
 .UNSPECIFIED., .F., .T. ) 
 B_SPLINE_CURVE_WITH_KNOTS ( ( 4, 4 ),
 ( 1.347909859412853573, 1.534781240595298746 ),
 .UNSPECIFIED. ) 
 CURVE ( )  GEOMETRIC_REPRESENTATION_ITEM ( )  RATIONAL_B_SPLINE_CURVE ( ( 1.000000000000000000, 0.9970920404276226723, 0.9970920404276226723, 1.000000000000000000 ) ) 
 REPRESENTATION_ITEM ( '' )  );
#17046 = CARTESIAN_POINT ( 'NONE',  ( -0.5103942914760696281, -26.98682223157766202, 7.670860738520326016 ) ) ;
#17047 = VERTEX_POINT ( 'NONE', #16622 ) ;
#17048 = ORIENTED_EDGE ( 'NONE', *, *, #12083, .F. ) ;
#17049 = CARTESIAN_POINT ( 'NONE',  ( 18.23781241676677567, -2.821824372035762529, 3.052849729433298354 ) ) ;
#17050 = CARTESIAN_POINT ( 'NONE',  ( 6.136079629878683050, -27.96984039756584295, 7.635761828346577573 ) ) ;
#17051 = CIRCLE ( 'NONE', #11143, 5.950000000000010836 ) ;
#17052 = CARTESIAN_POINT ( 'NONE',  ( 14.76670373698843441, -5.963909898562598677, -2.511099270873083267 ) ) ;
#17053 = EDGE_CURVE ( 'NONE', #37912, #25803, #35881, .T. ) ;
#17054 = CARTESIAN_POINT ( 'NONE',  ( 33.62697853900108669, -1.233820033134908067, -5.454701291197152635 ) ) ;
#17055 = CARTESIAN_POINT ( 'NONE',  ( -0.3487487021806359722, -26.64985754041175525, 6.700000000000000178 ) ) ;
#17056 = CARTESIAN_POINT ( 'NONE',  ( -1.808702272108716258, -33.43603381987017542, 6.954324564059724878 ) ) ;
#17057 = CARTESIAN_POINT ( 'NONE',  ( 29.67732598669241639, -3.794111227251059315, -4.438748131648309503 ) ) ;
#17058 = CARTESIAN_POINT ( 'NONE',  ( 3.858201203583684791, -26.94241211265677194, 7.695279973900954751 ) ) ;
#17059 = CARTESIAN_POINT ( 'NONE',  ( -70.92837670882107659, -37.87473357531881391, 10.00000000000000888 ) ) ;
#17060 = CARTESIAN_POINT ( 'NONE',  ( 5.002744721522525140, -28.44814603186448565, 7.782861076432730840 ) ) ;
#17061 = EDGE_LOOP ( 'NONE', ( #39945, #18098, #40518, #709 ) ) ;
#17062 = ORIENTED_EDGE ( 'NONE', *, *, #6333, .F. ) ;
#17063 = CARTESIAN_POINT ( 'NONE',  ( 34.14243320110696089, -3.848523200534588184, 5.234472016327581301 ) ) ;
#17064 = CARTESIAN_POINT ( 'NONE',  ( -1.599034431228576247, -30.73774772367137942, 6.894806418505347700 ) ) ;
#17065 = DIRECTION ( 'NONE',  ( 0.000000000000000000, -1.000000000000000000, 0.000000000000000000 ) ) ;
#17066 = CARTESIAN_POINT ( 'NONE',  ( 87.44460083197550659, -1.924926740212006049, 3.742195158538892397 ) ) ;
#17067 = CIRCLE ( 'NONE', #4610, 0.1000000000000028644 ) ;
#17068 = ORIENTED_EDGE ( 'NONE', *, *, #35541, .T. ) ;
#17069 = DIRECTION ( 'NONE',  ( -1.000000000000000000, 0.000000000000000000, 0.000000000000000000 ) ) ;
#17070 = SHAPE_REPRESENTATION_RELATIONSHIP ( 'NONE' , 'NONE' ,  #19830, #22541 ) ;
#17071 = ORIENTED_EDGE ( 'NONE', *, *, #8507, .T. ) ;
#17072 = CARTESIAN_POINT ( 'NONE',  ( 6.143759433280234994, -27.99094048399745205, 7.695279973900954751 ) ) ;
#17073 = EDGE_CURVE ( 'NONE', #1547, #2693, #26323, .T. ) ;
#17075 = DIRECTION ( 'NONE',  ( 0.000000000000000000, -0.000000000000000000, -1.000000000000000000 ) ) ;
#17074 = CARTESIAN_POINT ( 'NONE',  ( 4.822813956501135202, -27.98864294135706032, 6.941203072598473689 ) ) ;
#17076 = ORIENTED_EDGE ( 'NONE', *, *, #18319, .T. ) ;
#17077 = CARTESIAN_POINT ( 'NONE',  ( 23.65048145441440042, 3.304400666319548652, 3.618209137605786552 ) ) ;
#17078 = CARTESIAN_POINT ( 'NONE',  ( 82.29094429576466041, 64.52076745355560661, -1.905332024691357429 ) ) ;
#17079 = AXIS2_PLACEMENT_3D ( 'NONE', #40378, #8886, #31752 ) ;
#17080 = CARTESIAN_POINT ( 'NONE',  ( 4.458039033310292609, -27.41499233908904287, 7.754798119455333705 ) ) ;
#17081 = ORIENTED_EDGE ( 'NONE', *, *, #5532, .F. ) ;
#17082 = B_SPLINE_CURVE_WITH_KNOTS ( 'NONE', 3,
 ( #29153, #10600, #961, #7318, #4454, #19876, #13706, #29551, #16979, #32449, #4247, #25457, #9802, #28750, #560, #13095, #9999, #22582, #6920 ),
 .UNSPECIFIED., .F., .F.,
 ( 4, 3, 3, 3, 3, 3, 4 ),
 ( 0.000000000000000000, 2.546128104244798653E-05, 5.711050680484043828E-05, 8.113074941675955595E-05, 0.0001053129305727074305, 0.0001360598016347138838, 0.0001612931755713711509 ),
 .UNSPECIFIED. ) ;
#17084 = CARTESIAN_POINT ( 'NONE',  ( 4.413844959242510413, -27.38136177617460021, 7.784725160561910329 ) ) ;
#17083 = CARTESIAN_POINT ( 'NONE',  ( 0.08527861205520151366, -0.5999999999999994227, -3.903297362784067470 ) ) ;
#17085 = DIRECTION ( 'NONE',  ( -1.000000000000000000, -0.000000000000000000, -0.000000000000000000 ) ) ;
#17086 = CARTESIAN_POINT ( 'NONE',  ( 75.94307401167466764, 60.53934701228696014, 3.685888554891455282 ) ) ;
#17087 = VERTEX_POINT ( 'NONE', #39254 ) ;
#17088 = CARTESIAN_POINT ( 'NONE',  ( 22.26524600916998153, 2.472677414347903113, -5.130491956431036726 ) ) ;
#17089 = LINE ( 'NONE', #29662, #27024 ) ;
#17090 = EDGE_CURVE ( 'NONE', #32857, #26162, #32903, .T. ) ;
#17091 = CARTESIAN_POINT ( 'NONE',  ( -70.92837670882107659, -60.53509472482660669, -7.538952224936807056 ) ) ;
#17092 = DIRECTION ( 'NONE',  ( -1.000000000000000000, 0.000000000000000000, 0.000000000000000000 ) ) ;
#17093 = CARTESIAN_POINT ( 'NONE',  ( -62.74296742027563312, 35.98356920342448717, 5.167220874066855707 ) ) ;
#17094 = CARTESIAN_POINT ( 'NONE',  ( -0.01837800939314739035, -32.61883756299590686, 7.695279973900954751 ) ) ;
#17095 = CARTESIAN_POINT ( 'NONE',  ( 81.16810052477266879, 61.30343919788879248, 1.037317649801912323 ) ) ;
#17096 = CARTESIAN_POINT ( 'NONE',  ( 85.63852691662546590, 2.164466514264067332, 3.769402685279828358 ) ) ;
#17097 = CARTESIAN_POINT ( 'NONE',  ( 33.80908501075300165, -4.930824710404003497, 3.361253013157701197 ) ) ;
#17098 = CARTESIAN_POINT ( 'NONE',  ( -1.699515553723242700, -29.59554030218403398, 7.652160403243382980 ) ) ;
#17099 = CARTESIAN_POINT ( 'NONE',  ( 3.442434176459446160, -26.65012155745640499, 6.894806418505343260 ) ) ;
#17100 = CARTESIAN_POINT ( 'NONE',  ( -76.89654088401167087, -4.574922981678376743, -9.546023619539889538 ) ) ;
#17101 = ORIENTED_EDGE ( 'NONE', *, *, #816, .F. ) ;
#17102 = LINE ( 'NONE', #4379, #7283 ) ;
#17103 = ADVANCED_BREP_SHAPE_REPRESENTATION ( '', ( #39462, #30744 ), #11005 ) ;
#17104 = PLANE ( 'NONE',  #7857 ) ;
#17105 = EDGE_CURVE ( 'NONE', #17630, #7892, #17026, .T. ) ;
#17106 = CARTESIAN_POINT ( 'NONE',  ( 35.89366792997662969, -2.027922232554310700, -5.808472990748899001 ) ) ;
#17107 = CARTESIAN_POINT ( 'NONE',  ( 0.9924606702189815444, -32.89541365549410301, 7.757178535559533294 ) ) ;
#17108 = CARTESIAN_POINT ( 'NONE',  ( -1.789478617146011086, -29.22571177910124263, 7.501983001166816045 ) ) ;
#17109 = CARTESIAN_POINT ( 'NONE',  ( -14.97867591359219119, -26.64985754041175525, 6.700000000000000178 ) ) ;
#17110 = LINE ( 'NONE', #7659, #20424 ) ;
#17111 = CIRCLE ( 'NONE', #19751, 0.1000000000000028644 ) ;
#17112 = CARTESIAN_POINT ( 'NONE',  ( 4.325508966927646526, -31.73065943505188358, 7.721096864323899744 ) ) ;
#17113 = ORIENTED_EDGE ( 'NONE', *, *, #3762, .F. ) ;
#17114 = CARTESIAN_POINT ( 'NONE',  ( 21.58554998001892855, 4.069564031488925870, 3.350827065184835085 ) ) ;
#17115 = DIRECTION ( 'NONE',  ( -0.000000000000000000, -0.000000000000000000, 1.000000000000000000 ) ) ;
#17116 = CARTESIAN_POINT ( 'NONE',  ( 67.11291460916432072, 58.16531518584054794, -3.996350724342223604 ) ) ;
#17117 = EDGE_CURVE ( 'NONE', #21802, #8630, #35265, .T. ) ;
#17118 = CARTESIAN_POINT ( 'NONE',  ( 4.724705146729046845, -27.80824960587721506, 7.635761828346577573 ) ) ;
#17119 = ORIENTED_EDGE ( 'NONE', *, *, #35408, .T. ) ;
#17120 = DIRECTION ( 'NONE',  ( 0.02975940812527386875, -0.9995570907297058882, 0.000000000000000000 ) ) ;
#17121 = CARTESIAN_POINT ( 'NONE',  ( 86.29622000419868755, -0.2868749532368798372, -5.899445999458320600 ) ) ;
#17122 = CARTESIAN_POINT ( 'NONE',  ( 78.67056111734979140, 66.04450893328514383, 1.166167023198347641 ) ) ;
#17123 = CARTESIAN_POINT ( 'NONE',  ( 0.4906401998943609177, -26.28564864924214461, 7.635761828346577573 ) ) ;
#17124 = CARTESIAN_POINT ( 'NONE',  ( 0.3423729883474129210, -32.79573922743291092, 6.898188844117810525 ) ) ;
#17125 = CARTESIAN_POINT ( 'NONE',  ( -1.699561686978244612, -29.54937652563323169, 7.779495906702013741 ) ) ;
#17126 = ORIENTED_EDGE ( 'NONE', *, *, #10815, .F. ) ;
#17127 = CARTESIAN_POINT ( 'NONE',  ( 22.61751675538066664, 4.606962110408180600, 3.064415097794543463 ) ) ;
#17128 = CARTESIAN_POINT ( 'NONE',  ( -42.34874870218063592, -26.64985754041175525, 6.800000000000000711 ) ) ;
#17129 = CARTESIAN_POINT ( 'NONE',  ( 78.82816376705464734, 65.99584493362826265, 1.862141363775771108 ) ) ;
#17130 = CARTESIAN_POINT ( 'NONE',  ( 21.32955647224502371, -0.9288166341206904875, -4.803821987765101831 ) ) ;
#17131 = ORIENTED_EDGE ( 'NONE', *, *, #9542, .T. ) ;
#17132 = CARTESIAN_POINT ( 'NONE',  ( 79.47877296666170821, 61.98342160143342738, -3.470679136763286543 ) ) ;
#17133 = B_SPLINE_CURVE_WITH_KNOTS ( 'NONE', 3,
 ( #35396, #25906, #16611, #35592, #29787, #1602, #20311, #20116, #32302, #7362 ),
 .UNSPECIFIED., .F., .F.,
 ( 4, 3, 3, 4 ),
 ( 0.0002170292169044786025, 0.0002420761345915961192, 0.0002723302478207003654, 0.0002816811360866758253 ),
 .UNSPECIFIED. ) ;
#17135 = CARTESIAN_POINT ( 'NONE',  ( 14.69558624142723247, -4.492723223190125736, -2.499999999998670841 ) ) ;
#17134 = CARTESIAN_POINT ( 'NONE',  ( 22.61765175499198222, 0.2967575410182891060, 6.491500821813259492 ) ) ;
#17136 = EDGE_CURVE ( 'NONE', #25549, #833, #23426, .T. ) ;
#17137 = EDGE_CURVE ( 'NONE', #37233, #3771, #23230, .T. ) ;
#17138 = CARTESIAN_POINT ( 'NONE',  ( 81.49447160051741434, 61.73183938760860912, -1.953285432042047853 ) ) ;
#17139 = CARTESIAN_POINT ( 'NONE',  ( 79.14505932034367675, 62.66850290118684796, 3.750642650174859760 ) ) ;
#17140 = EDGE_CURVE ( 'NONE', #5954, #40651, #37153, .T. ) ;
#17141 = CARTESIAN_POINT ( 'NONE',  ( -0.9228924694586947419, -27.40696995593466312, 7.730758795053799481 ) ) ;
#17142 = CIRCLE ( 'NONE', #22439, 15.73502530973474478 ) ;
#17143 = CARTESIAN_POINT ( 'NONE',  ( 82.56222392620333039, 63.90769089702598649, 1.153249692834613427 ) ) ;
#17144 = CARTESIAN_POINT ( 'NONE',  ( 91.69672933337632514, -4.640393979863029372, -6.000000000000000888 ) ) ;
#17145 = CARTESIAN_POINT ( 'NONE',  ( 23.92064240948634790, 4.179079982057642972, -0.5982227118658990372 ) ) ;
#17146 = DIRECTION ( 'NONE',  ( -0.000000000000000000, -0.000000000000000000, 1.000000000000000000 ) ) ;
#17147 = ORIENTED_EDGE ( 'NONE', *, *, #15308, .T. ) ;
#17148 = CARTESIAN_POINT ( 'NONE',  ( -79.00905634357600604, -6.586509439605085170, 5.904778360221698108 ) ) ;
#17149 = CARTESIAN_POINT ( 'NONE',  ( 26.73391117787527449, 0.9274956043777666803, -4.382155566154702697 ) ) ;
#17150 = CARTESIAN_POINT ( 'NONE',  ( -62.92837670882106238, 3.729367930467589076, 6.000000000000000000 ) ) ;
#17151 = CARTESIAN_POINT ( 'NONE',  ( 5.160844861227617208, -29.04528478060791485, 6.865554069792297653 ) ) ;
#17152 = ORIENTED_EDGE ( 'NONE', *, *, #33915, .F. ) ;
#17153 = CARTESIAN_POINT ( 'NONE',  ( 20.91779001269123484, 4.579617817846264316, -2.660979186370516114 ) ) ;
#17154 = DIRECTION ( 'NONE',  ( -0.8660254037844415942, 0.4999999999999950040, -0.000000000000000000 ) ) ;
#17155 = CARTESIAN_POINT ( 'NONE',  ( 3.298377662289942336, -32.68384072543286578, 7.009310105710484073 ) ) ;
#17156 = CARTESIAN_POINT ( 'NONE',  ( -1.100009487556019350, -31.66939733285032688, 6.941203072598479018 ) ) ;
#17157 = DIRECTION ( 'NONE',  ( 1.000000000000000000, 0.000000000000000000, 0.000000000000000000 ) ) ;
#17158 = B_SPLINE_CURVE_WITH_KNOTS ( 'NONE', 3,
 ( #14378, #38894, #11082, #30245, #1450, #11487, #2060, #33140, #24050, #4922, #17261, #32939, #35834, #39296, #11280 ),
 .UNSPECIFIED., .F., .F.,
 ( 4, 1, 1, 1, 1, 1, 1, 1, 2, 2, 4 ),
 ( 0.000000000000000000, 0.2499999999992528754, 0.3749999999988793409, 0.4374999999986877164, 0.4687499999985918486, 0.4843749999985348387, 0.4921874999985063615, 0.4960937499984923171, 0.4980468749984970911, 0.4999999999985018651, 1.000000000000000000 ),
 .UNSPECIFIED. ) ;
#17159 = CARTESIAN_POINT ( 'NONE',  ( 2.745177312916512236, -32.80544076198930270, 6.863904403958575706 ) ) ;
#17160 = FACE_OUTER_BOUND ( 'NONE', #18589, .T. ) ;
#17161 = CIRCLE ( 'NONE', #22457, 0.1000000000000028644 ) ;
#17162 = CARTESIAN_POINT ( 'NONE',  ( 1.826114730284481347, -26.07217366336726982, 6.867199677474202346 ) ) ;
#17163 = ORIENTED_EDGE ( 'NONE', *, *, #10112, .F. ) ;
#17164 = ORIENTED_EDGE ( 'NONE', *, *, #16724, .F. ) ;
#17165 = CARTESIAN_POINT ( 'NONE',  ( 66.27376694608996388, 57.73522568913447373, 4.000000000000000000 ) ) ;
#17166 = CARTESIAN_POINT ( 'NONE',  ( 72.50225525176000474, 58.97572275893025306, -3.745173303611597948 ) ) ;
#17167 = ADVANCED_FACE ( 'NONE', ( #1225 ), #3920, .F. ) ;
#17168 = EDGE_LOOP ( 'NONE', ( #37662, #23516, #21296, #26619 ) ) ;
#17169 = CARTESIAN_POINT ( 'NONE',  ( 85.86655237490620607, 0.5075193453549979861, -5.999391133436077439 ) ) ;
#17170 = AXIS2_PLACEMENT_3D ( 'NONE', #38915, #10707, #20185 ) ;
#17171 = CYLINDRICAL_SURFACE ( 'NONE', #25892, 0.1000000000000028644 ) ;
#17172 = CARTESIAN_POINT ( 'NONE',  ( -81.07947155388369254, 30.81399289130168384, -46.17089178453873188 ) ) ;
#17173 = CARTESIAN_POINT ( 'NONE',  ( 2.872971158482682696, -26.27219422606927424, 7.737115613922530777 ) ) ;
#17174 = APPLICATION_PROTOCOL_DEFINITION ( 'draft international standard', 'automotive_design', 1998, #1357 ) ;
#17175 = EDGE_CURVE ( 'NONE', #22380, #17583, #14146, .T. ) ;
#17176 = CARTESIAN_POINT ( 'NONE',  ( 2.270544122507286211, -32.92179816162761341, 7.779495906702013741 ) ) ;
#17177 = CARTESIAN_POINT ( 'NONE',  ( -33.07867591359219972, -26.64985754041175525, 6.700000000000000178 ) ) ;
#17178 = CARTESIAN_POINT ( 'NONE',  ( -1.751114083487925521, -28.98930116072738628, 7.655937882338901268 ) ) ;
#17179 = EDGE_CURVE ( 'NONE', #39825, #38785, #810, .T. ) ;
#17180 = ORIENTED_EDGE ( 'NONE', *, *, #26380, .T. ) ;
#17181 = CARTESIAN_POINT ( 'NONE',  ( 79.59524243168472424, 64.21532580903935639, -3.665158340976947038 ) ) ;
#17182 = CARTESIAN_POINT ( 'NONE',  ( 37.16547997189702812, -2.549274111243842622, 5.977208762129640363 ) ) ;
#17183 = CARTESIAN_POINT ( 'NONE',  ( 79.94486516293738987, 63.68863865526455470, 3.714073935154435624 ) ) ;
#17184 = PLANE ( 'NONE',  #15117 ) ;
#17185 = B_SPLINE_CURVE_WITH_KNOTS ( 'NONE', 3,
 ( #12146, #28005, #9064, #34220 ),
 .UNSPECIFIED., .F., .F.,
 ( 4, 4 ),
 ( 0.000000000000000000, 1.000000000000000000 ),
 .UNSPECIFIED. ) ;
#17186 = ADVANCED_FACE ( 'NONE', ( #25917 ), #35404, .F. ) ;
#17187 = CARTESIAN_POINT ( 'NONE',  ( -28.24874870218063805, -26.64985754041175525, 6.700000000000000178 ) ) ;
#17188 = CARTESIAN_POINT ( 'NONE',  ( 16.43915176107237031, 10.14349373407899790, -2.724152508961429575 ) ) ;
#17189 = CARTESIAN_POINT ( 'NONE',  ( 17.71472783233827641, 13.97198263493282688, 2.499999999999999556 ) ) ;
#17190 = CARTESIAN_POINT ( 'NONE',  ( 21.85643539959775694, 2.022457263371903569, 13.81434276849105558 ) ) ;
#17191 = CARTESIAN_POINT ( 'NONE',  ( -62.86576508122315943, 38.67912974266877058, -7.000000000000000000 ) ) ;
#17192 = ORIENTED_EDGE ( 'NONE', *, *, #28966, .F. ) ;
#17193 = CARTESIAN_POINT ( 'NONE',  ( -71.92837670882106238, -42.87473357531881391, -1.732050807568860318 ) ) ;
#17194 = VERTEX_POINT ( 'NONE', #23035 ) ;
#17195 = CARTESIAN_POINT ( 'NONE',  ( 14.74825476816264391, -5.104108582077598655, 2.500092996181281890 ) ) ;
#17196 = VECTOR ( 'NONE', #22646, 1000.000000000000000 ) ;
#17197 = CARTESIAN_POINT ( 'NONE',  ( -73.13538128175785857, 0.2574294580082270301, -10.93005075941053938 ) ) ;
#17198 = CARTESIAN_POINT ( 'NONE',  ( 1.489942920397620885, -32.96341103692402186, 6.949473656533217358 ) ) ;
#17199 = CARTESIAN_POINT ( 'NONE',  ( 2.433491429741967416, -26.24990572107254394, 6.868387053540520704 ) ) ;
#17200 = CARTESIAN_POINT ( 'NONE',  ( 80.03809576917893764, 64.85583152007151853, 3.406228740995816295 ) ) ;
#17201 = CARTESIAN_POINT ( 'NONE',  ( -71.92837670882107659, -0.7829914368874778541, 5.916079783099617906 ) ) ;
#17202 = CARTESIAN_POINT ( 'NONE',  ( -70.92837670882107659, 28.72470171467712063, 0.000000000000000000 ) ) ;
#17203 = CARTESIAN_POINT ( 'NONE',  ( -2.327064883976697640, -32.63228849572541890, 6.894806418505347700 ) ) ;
#17204 = DIRECTION ( 'NONE',  ( 0.9848077530122083534, -0.1736481776669292765, 0.000000000000000000 ) ) ;
#17205 = CARTESIAN_POINT ( 'NONE',  ( 31.28402977554648601, -0.4023986077216939461, 5.089027472230029048 ) ) ;
#17206 = CARTESIAN_POINT ( 'NONE',  ( 3.963477911421234623, -32.23984282750152630, 7.750000000000001776 ) ) ;
#17207 = CARTESIAN_POINT ( 'NONE',  ( 1.114803370050245102, -33.02060082531637164, 7.646866513072557048 ) ) ;
#17208 = LINE ( 'NONE', #29775, #40456 ) ;
#17209 = DIRECTION ( 'NONE',  ( -0.7660444431189818992, 0.6427876096865345890, 0.000000000000000000 ) ) ;
#17210 = CARTESIAN_POINT ( 'NONE',  ( 68.15116243724637002, 58.05457144382717871, 3.974537232972704892 ) ) ;
#17211 = CARTESIAN_POINT ( 'NONE',  ( 33.46244823565493220, -3.089030447167950832, 5.429022358179501850 ) ) ;
#17212 = CARTESIAN_POINT ( 'NONE',  ( -3.078675913592197944, -26.64985754041175525, 6.800000000000000711 ) ) ;
#17213 = CARTESIAN_POINT ( 'NONE',  ( 87.20660408302002509, 0.2574974038930863407, -5.635807106906071340 ) ) ;
#17215 = CARTESIAN_POINT ( 'NONE',  ( -0.5137931472823115131, -26.85930784658432202, 6.880608371227953768 ) ) ;
#17214 = CARTESIAN_POINT ( 'NONE',  ( 80.45813098276144615, 63.95641783144333203, -3.614389211669655655 ) ) ;
#17216 = CARTESIAN_POINT ( 'NONE',  ( -1.315039247493585250, -27.79308300620435901, 6.894806418505347700 ) ) ;
#17217 = CARTESIAN_POINT ( 'NONE',  ( 2.422160802983875261, -26.14601410332325315, 7.761113333117551250 ) ) ;
#17218 = ORIENTED_EDGE ( 'NONE', *, *, #6829, .T. ) ;
#17219 = CARTESIAN_POINT ( 'NONE',  ( 0.6527267737179240914, -26.33536660093865578, 7.754798119455333705 ) ) ;
#17220 = CARTESIAN_POINT ( 'NONE',  ( 3.739317481034212243, -32.29073431218959911, 7.013842709614101167 ) ) ;
#17221 = VERTEX_POINT ( 'NONE', #19927 ) ;
#17222 = LINE ( 'NONE', #23226, #7714 ) ;
#17223 = EDGE_LOOP ( 'NONE', ( #10834, #39512, #9762, #19637, #38918, #12376, #34353, #1413, #29508, #11957, #8207, #8945, #16129, #23618, #17414, #18876, #14489, #15796, #16471, #3234, #15893, #17152, #29097, #20162, #2680, #35324, #7804, #21519, #20356, #6314, #38336, #9693, #31876, #33438, #6478, #36753, #1451, #7933, #36645, #25215, #11451, #7256, #2445, #31596, #32809, #31469, #19783, #4053, #23550, #7618, #16219, #8066, #20362, #24265, #15259, #19454, #37991, #35025 ) ) ;
#17224 = CARTESIAN_POINT ( 'NONE',  ( 80.17861389908763670, 63.81053541282437180, -3.679799701112256294 ) ) ;
#17225 = LINE ( 'NONE', #13952, #12853 ) ;
#17226 = CARTESIAN_POINT ( 'NONE',  ( 79.39546522070097012, 65.15502244391696252, 3.213872034465147909 ) ) ;
#17227 = CARTESIAN_POINT ( 'NONE',  ( 22.77570511409684073, 0.4895864838293038646, 6.218135402904170661 ) ) ;
#17229 = ORIENTED_EDGE ( 'NONE', *, *, #39407, .F. ) ;
#17228 = CARTESIAN_POINT ( 'NONE',  ( -69.92837670882107659, -0.7829914368874778541, 5.916079783099612577 ) ) ;
#17230 = EDGE_CURVE ( 'NONE', #34912, #1373, #32504, .T. ) ;
#17231 = EDGE_CURVE ( 'NONE', #9551, #30327, #27314, .T. ) ;
#17233 = EDGE_CURVE ( 'NONE', #40311, #23873, #8156, .T. ) ;
#17232 = CARTESIAN_POINT ( 'NONE',  ( -0.09205880772810777490, -32.45907920833084859, 7.768425012602593327 ) ) ;
#17235 = CARTESIAN_POINT ( 'NONE',  ( -54.01549048184568846, -38.28842912540938670, -4.152976064860135708 ) ) ;
#17234 = CARTESIAN_POINT ( 'NONE',  ( 63.05383694556373797, -7.271989087314214117, -6.000000000000000000 ) ) ;
#17236 = LINE ( 'NONE', #38868, #36289 ) ;
#17237 = DIRECTION ( 'NONE',  ( -0.8888117386314180468, -0.4582725098355734938, 0.000000000000000000 ) ) ;
#17238 = CARTESIAN_POINT ( 'NONE',  ( 22.14579855485407123, 4.734495042501529305, -3.551530763287582548 ) ) ;
#17239 = VERTEX_POINT ( 'NONE', #2023 ) ;
#17240 = CARTESIAN_POINT ( 'NONE',  ( -71.54306152300276267, 0.01646366005082695524, 5.969151678864089483 ) ) ;
#17241 = CARTESIAN_POINT ( 'NONE',  ( 22.40835304001176098, 2.012838380346585243, -8.570566085397546274 ) ) ;
#17242 = CARTESIAN_POINT ( 'NONE',  ( 16.70600419673038672, 9.848044529300576500, 2.500000000000113687 ) ) ;
#17243 = ORIENTED_EDGE ( 'NONE', *, *, #39305, .T. ) ;
#17244 = DIRECTION ( 'NONE',  ( -0.000000000000000000, -0.000000000000000000, 1.000000000000000000 ) ) ;
#17245 = CARTESIAN_POINT ( 'NONE',  ( 79.58537830805853730, 65.88021587146288027, 2.518708746844645407 ) ) ;
#17246 = CARTESIAN_POINT ( 'NONE',  ( 85.17963886742116131, 2.035184340541872139, -4.783483324554544502 ) ) ;
#17247 = CARTESIAN_POINT ( 'NONE',  ( -14.44874870218064089, -25.49307895267003587, 6.700000000000000178 ) ) ;
#17248 = ORIENTED_EDGE ( 'NONE', *, *, #24489, .F. ) ;
#17249 = CARTESIAN_POINT ( 'NONE',  ( -70.92837670882107659, 13.87661300689593880, 0.000000000000000000 ) ) ;
#17250 = VERTEX_POINT ( 'NONE', #33313 ) ;
#17251 = CARTESIAN_POINT ( 'NONE',  ( -36.24874870218063450, -25.49307895267003587, 6.800000000000000711 ) ) ;
#17252 = CARTESIAN_POINT ( 'NONE',  ( 17.00616749447241105, -3.062907964995312593, -2.860621751864253159 ) ) ;
#17253 = CARTESIAN_POINT ( 'NONE',  ( 21.25348834460957193, 3.320962670253897908, -3.523518892371187761 ) ) ;
#17254 = DIRECTION ( 'NONE',  ( 1.000000000000000000, -8.959828616340678715E-16, 0.000000000000000000 ) ) ;
#17255 = CARTESIAN_POINT ( 'NONE',  ( -0.9786759135921931918, -26.64985754041175525, 6.800000000000000711 ) ) ;
#17256 = CARTESIAN_POINT ( 'NONE',  ( 29.77376427528636782, -3.774992202640799377, -4.469883408169392780 ) ) ;
#17257 = ORIENTED_EDGE ( 'NONE', *, *, #32930, .T. ) ;
#17258 = CARTESIAN_POINT ( 'NONE',  ( 3.858201203583684791, -26.94241211265676839, 7.693875151218752428 ) ) ;
#17259 = VECTOR ( 'NONE', #23765, 1000.000000000000114 ) ;
#17260 = LINE ( 'NONE', #3949, #35594 ) ;
#17261 = CARTESIAN_POINT ( 'NONE',  ( 31.82986595668942797, -2.965385599430104158, -5.174218409395310303 ) ) ;
#17262 = VERTEX_POINT ( 'NONE', #33933 ) ;
#17263 = ORIENTED_EDGE ( 'NONE', *, *, #12630, .F. ) ;
#17264 = CARTESIAN_POINT ( 'NONE',  ( 36.13284885545721181, -1.530137503075135186, 5.642985908650910432 ) ) ;
#17265 = CARTESIAN_POINT ( 'NONE',  ( -1.629426256325140487, -30.64809085600286664, 6.867199677474202346 ) ) ;
#17266 = CARTESIAN_POINT ( 'NONE',  ( 66.27376694609004915, 57.73522568913436004, -4.000000000000000000 ) ) ;
#17267 = CARTESIAN_POINT ( 'NONE',  ( 87.45314133599802631, -1.935575868345978057, 3.712183661284619962 ) ) ;
#17268 = EDGE_LOOP ( 'NONE', ( #17681, #16222, #4715, #12059 ) ) ;
#17269 = CARTESIAN_POINT ( 'NONE',  ( 5.142064470514565500, -28.93363034780944076, 7.730015791551945625 ) ) ;
#17270 = CARTESIAN_POINT ( 'NONE',  ( -56.24615026952713492, 30.21122693717869367, -1.618048866027542498 ) ) ;
#17271 = AXIS2_PLACEMENT_3D ( 'NONE', #6737, #28558, #37199 ) ;
#17273 = DIRECTION ( 'NONE',  ( 1.000000000000000000, 0.000000000000000000, 0.000000000000000000 ) ) ;
#17272 = CARTESIAN_POINT ( 'NONE',  ( 4.801435222562028926, -27.94711808525471852, 6.875780273367530171 ) ) ;
#17274 = ORIENTED_EDGE ( 'NONE', *, *, #14222, .F. ) ;
#17275 = CARTESIAN_POINT ( 'NONE',  ( 22.33423834887513237, 4.544082872025895448, 3.505951737637754029 ) ) ;
#17276 = CARTESIAN_POINT ( 'NONE',  ( 81.88210331175112344, 61.92077230045136105, -1.461108304022173732 ) ) ;
#17278 = EDGE_CURVE ( 'NONE', #6636, #10306, #11651, .T. ) ;
#17277 = CARTESIAN_POINT ( 'NONE',  ( 14.77222818450456643, -4.461908109758233820, -2.511961494517393145 ) ) ;
#17279 = ORIENTED_EDGE ( 'NONE', *, *, #37581, .T. ) ;
#17280 = B_SPLINE_CURVE_WITH_KNOTS ( 'NONE', 3,
 ( #7145, #4270, #13919, #16402, #35172, #19899, #19507, #29176, #32673, #10819 ),
 .UNSPECIFIED., .F., .F.,
 ( 4, 3, 3, 4 ),
 ( 0.0001585009270395757776, 0.0001815657551981876637, 0.0002118214035944180620, 0.0002170292169044793886 ),
 .UNSPECIFIED. ) ;
#17282 = CARTESIAN_POINT ( 'NONE',  ( 16.23110856389288514, -3.299995616322477954, -2.739655060876247106 ) ) ;
#17281 = DIRECTION ( 'NONE',  ( 0.000000000000000000, 0.000000000000000000, 1.000000000000000000 ) ) ;
#17283 = DIRECTION ( 'NONE',  ( 1.000000000000000000, 0.000000000000000000, 0.000000000000000000 ) ) ;
#17284 = CARTESIAN_POINT ( 'NONE',  ( 75.27909492816711179, 60.48191808705185224, 3.786335567263138469 ) ) ;
#17285 = CIRCLE ( 'NONE', #4165, 0.1000000000000028644 ) ;
#17286 = CARTESIAN_POINT ( 'NONE',  ( 23.31884880910575220, 2.914054986383341816, -4.090107105141986388 ) ) ;
#17287 = CARTESIAN_POINT ( 'NONE',  ( 7.121324086407810228, -26.64985754041175525, 6.700000000000000178 ) ) ;
#17288 = CYLINDRICAL_SURFACE ( 'NONE', #33330, 3.399999999999999911 ) ;
#17289 = DIRECTION ( 'NONE',  ( -0.000000000000000000, -0.000000000000000000, 1.000000000000000000 ) ) ;
#17290 = CARTESIAN_POINT ( 'NONE',  ( -62.78665125536710434, 35.69261095098032399, 5.591393777931260800 ) ) ;
#17291 = CARTESIAN_POINT ( 'NONE',  ( 1.672850645881087894, -26.07003693891804019, 7.655937882338900380 ) ) ;
#17292 = CARTESIAN_POINT ( 'NONE',  ( 79.16788024942142954, 66.21349342525120107, 1.524764441711115914 ) ) ;
#17293 = CARTESIAN_POINT ( 'NONE',  ( 88.13490256179494509, -0.6395810955261213016, -2.488665338685403849 ) ) ;
#17294 = CARTESIAN_POINT ( 'NONE',  ( 32.32438508616473882, -2.203219671913323019, -5.968588774572396893 ) ) ;
#17295 = DIRECTION ( 'NONE',  ( 0.000000000000000000, 0.000000000000000000, 1.000000000000000000 ) ) ;
#17296 = CARTESIAN_POINT ( 'NONE',  ( -71.85035947768736264, -45.91779912024241384, 9.958377439660317521 ) ) ;
#17297 = CARTESIAN_POINT ( 'NONE',  ( -73.32814786518467542, -0.3430638954784143158, -10.90362257782414446 ) ) ;
#17298 = CARTESIAN_POINT ( 'NONE',  ( 0.5983277861368044848, -26.35348481447137203, 6.880147297696980857 ) ) ;
#17299 = AXIS2_PLACEMENT_3D ( 'NONE', #541, #32036, #32240 ) ;
#17300 = AXIS2_PLACEMENT_3D ( 'NONE', #29110, #31800, #10152 ) ;
#17301 = CARTESIAN_POINT ( 'NONE',  ( 0.1024025241762535204, -26.45601964135392592, 7.009310105710488514 ) ) ;
#17302 = CARTESIAN_POINT ( 'NONE',  ( 27.48830597204979398, 1.193411793497110018, -4.496612972767297656 ) ) ;
#17303 = CARTESIAN_POINT ( 'NONE',  ( 5.401390093233090717, -29.44812577374269580, 7.754798119455333705 ) ) ;
#17304 = CARTESIAN_POINT ( 'NONE',  ( 4.976842733950423536, -28.33913446795707358, 7.695279973900954751 ) ) ;
#17305 = CARTESIAN_POINT ( 'NONE',  ( -1.592719143486283517, -28.38440999418950739, 7.756742906098588186 ) ) ;
#17306 = EDGE_CURVE ( 'NONE', #4710, #4303, #16808, .T. ) ;
#17307 = CARTESIAN_POINT ( 'NONE',  ( -71.72837670882105954, -34.30579396504363388, -1.385640646055078307 ) ) ;
#17308 = VERTEX_POINT ( 'NONE', #30633 ) ;
#17309 = CARTESIAN_POINT ( 'NONE',  ( 36.96305683104023387, -3.150446582698992248, 5.966424068676240644 ) ) ;
#17310 = CARTESIAN_POINT ( 'NONE',  ( -70.70332177653823180, 0.1913546399533780362, 6.007821842535422618 ) ) ;
#17311 = CARTESIAN_POINT ( 'NONE',  ( 67.47105843325410035, 58.09313517554802075, -3.997566301760142160 ) ) ;
#17312 = CARTESIAN_POINT ( 'NONE',  ( 3.032804972883730521, -26.33347060717657584, 6.875780273367530171 ) ) ;
#17313 = ADVANCED_FACE ( 'NONE', ( #2222 ), #30205, .F. ) ;
#17314 = ORIENTED_EDGE ( 'NONE', *, *, #24676, .F. ) ;
#17315 = CARTESIAN_POINT ( 'NONE',  ( -1.642550015356792681, -30.60663237321507069, 7.013842709614101167 ) ) ;
#17316 = DIRECTION ( 'NONE',  ( -0.000000000000000000, 1.000000000000000000, -0.000000000000000000 ) ) ;
#17317 = CARTESIAN_POINT ( 'NONE',  ( -60.05933043039491537, 24.84364830758654108, 9.240995299818667519 ) ) ;
#17318 = CARTESIAN_POINT ( 'NONE',  ( 1.057042051752609346, -32.90850936937915350, 6.889465824494256374 ) ) ;
#17319 = CARTESIAN_POINT ( 'NONE',  ( 3.599609112215594209, -26.63003781836791362, 7.006908160621414083 ) ) ;
#17320 = DIRECTION ( 'NONE',  ( -0.8660254037844381525, 0.000000000000000000, 0.5000000000000008882 ) ) ;
#17321 = ORIENTED_EDGE ( 'NONE', *, *, #20115, .T. ) ;
#17322 = CARTESIAN_POINT ( 'NONE',  ( 23.74696602062051554, 3.565733413989425671, 3.171546063783087455 ) ) ;
#17323 = CARTESIAN_POINT ( 'NONE',  ( -71.92837670882107659, -0.7829914368874778541, 9.949874371066204759 ) ) ;
#17325 = AXIS2_PLACEMENT_3D ( 'NONE', #20219, #23523, #4781 ) ;
#17324 = CARTESIAN_POINT ( 'NONE',  ( 79.89688848262225918, 64.77169266163326711, 3.452358620554652813 ) ) ;
#17327 = EDGE_CURVE ( 'NONE', #26935, #19421, #36077, .T. ) ;
#17326 = CARTESIAN_POINT ( 'NONE',  ( -14.87867591359218977, -24.55319635012989110, 6.700000000000000178 ) ) ;
#17328 = ORIENTED_EDGE ( 'NONE', *, *, #29288, .T. ) ;
#17329 = CARTESIAN_POINT ( 'NONE',  ( 78.16578481971130543, 61.75018358139118391, -3.687756614093558039 ) ) ;
#17331 = CARTESIAN_POINT ( 'NONE',  ( 14.76033746053277262, -5.150563244451003442, -2.500007713060570236 ) ) ;
#17330 = CARTESIAN_POINT ( 'NONE',  ( 21.97535319280600064, 0.2262477332863455926, 7.720624099575212895 ) ) ;
#17332 = CARTESIAN_POINT ( 'NONE',  ( 81.53696963055698177, 62.69563756174608926, -2.920975158733595034 ) ) ;
#17333 = CARTESIAN_POINT ( 'NONE',  ( 78.94057287092958575, 63.80484286357250312, 3.729426069516721398 ) ) ;
#17334 = VECTOR ( 'NONE', #6822, 1000.000000000000000 ) ;
#17335 = CARTESIAN_POINT ( 'NONE',  ( 36.28802971627182217, -3.619218337158335075, -5.742874455817792878 ) ) ;
#17336 = CARTESIAN_POINT ( 'NONE',  ( 82.47129118679434612, 63.86074534520110291, 1.718006205139013698 ) ) ;
#17337 = DIRECTION ( 'NONE',  ( -0.000000000000000000, -0.000000000000000000, 1.000000000000000000 ) ) ;
#17338 = CARTESIAN_POINT ( 'NONE',  ( 28.36395155556995817, 1.046816072451675517, -4.961098188302698553 ) ) ;
#17339 = CARTESIAN_POINT ( 'NONE',  ( -63.02437332573797590, 35.53684452423017603, -6.244480380085997595 ) ) ;
#17340 = ORIENTED_EDGE ( 'NONE', *, *, #33850, .T. ) ;
#17341 = CARTESIAN_POINT ( 'NONE',  ( 85.57577930415899914, 1.015208198401525541, 5.782835925834406865 ) ) ;
#17342 = CARTESIAN_POINT ( 'NONE',  ( 21.78506910207827829, 0.2162159629002408934, -8.389536844142153171 ) ) ;
#17343 = EDGE_CURVE ( 'NONE', #29464, #5443, #36788, .T. ) ;
#17344 = CARTESIAN_POINT ( 'NONE',  ( 13.52694889643372278, 17.29870644234688370, -2.500000000000000000 ) ) ;
#17345 = ORIENTED_EDGE ( 'NONE', *, *, #2031, .T. ) ;
#17346 = CARTESIAN_POINT ( 'NONE',  ( 5.173490979662657807, -29.13678236134181887, 6.903112506833891437 ) ) ;
#17347 = CARTESIAN_POINT ( 'NONE',  ( 35.36129965878185999, -3.735671557810035015, -5.554315758203441256 ) ) ;
#17348 = CARTESIAN_POINT ( 'NONE',  ( 5.026281758278582146, -30.27593629695115496, 6.864216812889196717 ) ) ;
#17349 = CARTESIAN_POINT ( 'NONE',  ( 3.284898187062045061, -32.69072080446853334, 6.980586498568963627 ) ) ;
#17350 = CARTESIAN_POINT ( 'NONE',  ( -64.85784325972055342, 34.81586596186931359, -6.466735817496061856 ) ) ;
#17351 = PLANE ( 'NONE',  #12039 ) ;
#17352 = CARTESIAN_POINT ( 'NONE',  ( -66.99872204295122913, 28.48507918597134037, -46.17089178453873188 ) ) ;
#17353 = CARTESIAN_POINT ( 'NONE',  ( 5.094551125703637773, -29.76914366077792451, 6.997764925645186374 ) ) ;
#17354 = CARTESIAN_POINT ( 'NONE',  ( 1.873447534517880264, -26.07421076434662410, 7.009310105710485850 ) ) ;
#17355 = VECTOR ( 'NONE', #6080, 1000.000000000000000 ) ;
#17356 = ORIENTED_EDGE ( 'NONE', *, *, #13870, .F. ) ;
#17357 = EDGE_CURVE ( 'NONE', #19595, #11405, #9684, .T. ) ;
#17358 = ORIENTED_EDGE ( 'NONE', *, *, #25890, .T. ) ;
#17360 = EDGE_CURVE ( 'NONE', #27566, #38693, #14341, .T. ) ;
#17359 = CARTESIAN_POINT ( 'NONE',  ( 66.58940539569050543, 57.77934511969053943, 3.999344142514785538 ) ) ;
#17361 = CARTESIAN_POINT ( 'NONE',  ( 71.03485184658521234, 59.25305893485334963, -3.963404584535439312 ) ) ;
#17362 = EDGE_CURVE ( 'NONE', #10579, #16251, #29292, .T. ) ;
#17363 = AXIS2_PLACEMENT_3D ( 'NONE', #1492, #14025, #20206 ) ;
#17364 = ORIENTED_EDGE ( 'NONE', *, *, #17, .F. ) ;
#17365 = CARTESIAN_POINT ( 'NONE',  ( 87.68748590470411841, -1.878626560869070872, 3.708385665356400906 ) ) ;
#17366 = DIRECTION ( 'NONE',  ( -0.000000000000000000, -0.000000000000000000, 1.000000000000000000 ) ) ;
#17367 = DIRECTION ( 'NONE',  ( -1.000000000000000000, -2.192388006395421260E-15, 0.000000000000000000 ) ) ;
#17368 = APPLICATION_PROTOCOL_DEFINITION ( 'draft international standard', 'automotive_design', 1998, #21603 ) ;
#17369 = FACE_OUTER_BOUND ( 'NONE', #16280, .T. ) ;
#17370 = CARTESIAN_POINT ( 'NONE',  ( 23.76457672120657705, 3.581884546121536061, 3.114801549680321191 ) ) ;
#17371 = CARTESIAN_POINT ( 'NONE',  ( 5.180766528530944548, -29.99759455875544489, 7.134293011406493079 ) ) ;
#17372 = EDGE_CURVE ( 'NONE', #33264, #24867, #9810, .T. ) ;
#17373 = VERTEX_POINT ( 'NONE', #21568 ) ;
#17374 = CARTESIAN_POINT ( 'NONE',  ( 80.23208661909926320, 62.50324886901235999, -3.482780605906225624 ) ) ;
#17375 = FACE_OUTER_BOUND ( 'NONE', #4317, .T. ) ;
#17376 = CARTESIAN_POINT ( 'NONE',  ( 80.63281215842032168, 62.09153919268370458, 3.087291694836661549 ) ) ;
#17377 = CARTESIAN_POINT ( 'NONE',  ( 0.4238093638620683556, -32.72117464255529029, 7.754798119455333705 ) ) ;
#17378 = VECTOR ( 'NONE', #21282, 1000.000000000000114 ) ;
#17379 = CIRCLE ( 'NONE', #6256, 6.000000000000002665 ) ;
#17380 = PLANE ( 'NONE',  #3120 ) ;
#17381 = AXIS2_PLACEMENT_3D ( 'NONE', #3641, #34932, #22965 ) ;
#17382 = CARTESIAN_POINT ( 'NONE',  ( 4.042062268558281879, -27.10485839313172107, 6.939395833800443114 ) ) ;
#17383 = CYLINDRICAL_SURFACE ( 'NONE', #18269, 0.09010775117052950700 ) ;
#17384 = CARTESIAN_POINT ( 'NONE',  ( 21.85643539959775694, 0.6980322203039187601, 15.81276153107902616 ) ) ;
#17385 = ORIENTED_EDGE ( 'NONE', *, *, #12472, .F. ) ;
#17386 = DIRECTION ( 'NONE',  ( -0.000000000000000000, 1.000000000000000000, -0.000000000000000000 ) ) ;
#17387 = CARTESIAN_POINT ( 'NONE',  ( 14.67710233104394923, -4.950387941734374131, 2.499999999999891198 ) ) ;
#17388 = CARTESIAN_POINT ( 'NONE',  ( -76.77055093545936870, 10.78502741370083662, -8.125255635421307687 ) ) ;
#17389 = DIRECTION ( 'NONE',  ( -1.000000000000000000, 0.000000000000000000, 0.000000000000000000 ) ) ;
#17390 = CARTESIAN_POINT ( 'NONE',  ( 1.700390093233090871, -29.56993018339339940, 7.750000000000000888 ) ) ;
#17391 = CARTESIAN_POINT ( 'NONE',  ( 81.30779604900573077, 61.65202803940792364, 2.079311677127710478 ) ) ;
#17392 = CARTESIAN_POINT ( 'NONE',  ( -1.484429692467435391, -30.76027941025985513, 7.730758795053808363 ) ) ;
#17393 =( BOUNDED_CURVE ( )  B_SPLINE_CURVE ( 3, ( #20741, #33329, #9000, #36602 ),
 .UNSPECIFIED., .F., .F. ) 
 B_SPLINE_CURVE_WITH_KNOTS ( ( 4, 4 ),
 ( 1.347909859412854239, 1.534781240595299190 ),
 .UNSPECIFIED. ) 
 CURVE ( )  GEOMETRIC_REPRESENTATION_ITEM ( )  RATIONAL_B_SPLINE_CURVE ( ( 1.000000000000000000, 0.9970920404276226723, 0.9970920404276226723, 1.000000000000000000 ) ) 
 REPRESENTATION_ITEM ( '' )  );
#17394 = CARTESIAN_POINT ( 'NONE',  ( 3.863350320691840700, -26.94664762070162567, 7.730758795053802146 ) ) ;
#17395 = CARTESIAN_POINT ( 'NONE',  ( -1.020414035563122601, -31.60885757119451256, 7.013842709614101167 ) ) ;
#17396 = CARTESIAN_POINT ( 'NONE',  ( -70.42482556194003962, 0.09084953194484755856, 9.988048282181825499 ) ) ;
#17397 = ADVANCED_FACE ( 'NONE', ( #9391 ), #34759, .F. ) ;
#17398 = CARTESIAN_POINT ( 'NONE',  ( -64.16905995053024014, 35.05897458415617507, 4.706112250371591088 ) ) ;
#17399 = EDGE_CURVE ( 'NONE', #826, #7900, #6534, .T. ) ;
#17400 = CARTESIAN_POINT ( 'NONE',  ( 1.107728911050566145, -33.01938716874131075, 7.637894019485640840 ) ) ;
#17401 = CARTESIAN_POINT ( 'NONE',  ( 67.64019463258649978, 58.53452770292938112, 3.982857479566666914 ) ) ;
#17402 = CARTESIAN_POINT ( 'NONE',  ( 33.68138841437632180, -3.186010531076846508, 5.463193268119806767 ) ) ;
#17403 = EDGE_CURVE ( 'NONE', #38693, #31247, #3465, .T. ) ;
#17404 = AXIS2_PLACEMENT_3D ( 'NONE', #37665, #18954, #224 ) ;
#17405 = CARTESIAN_POINT ( 'NONE',  ( 2.262923698813503748, -33.00986142210201990, 7.785096263473211486 ) ) ;
#17406 = VECTOR ( 'NONE', #11495, 1000.000000000000000 ) ;
#17407 = CARTESIAN_POINT ( 'NONE',  ( 85.61973765214487742, 2.185571507920985646, -3.964146163151171187 ) ) ;
#17409 = DIRECTION ( 'NONE',  ( -0.000000000000000000, 1.000000000000000000, -0.000000000000000000 ) ) ;
#17408 = CARTESIAN_POINT ( 'NONE',  ( 80.38808068765766279, 63.91986139366765940, -3.633989118465184021 ) ) ;
#17410 = CARTESIAN_POINT ( 'NONE',  ( -1.638189092752657006, -28.92658214191287769, 6.889465824494254598 ) ) ;
#17411 = CARTESIAN_POINT ( 'NONE',  ( -58.37631287976132199, 28.09510535829622668, 3.265447219236210952 ) ) ;
#17412 = ORIENTED_EDGE ( 'NONE', *, *, #38061, .T. ) ;
#17413 = CARTESIAN_POINT ( 'NONE',  ( -0.6767161412783136987, -32.13885329431887072, 6.895394898881668233 ) ) ;
#17414 = ORIENTED_EDGE ( 'NONE', *, *, #15481, .F. ) ;
#17415 = FACE_OUTER_BOUND ( 'NONE', #37883, .T. ) ;
#17416 = CARTESIAN_POINT ( 'NONE',  ( 81.07747211222714157, 61.58128768033695621, -2.227525437860508273 ) ) ;
#17417 = CARTESIAN_POINT ( 'NONE',  ( -1.523348320565749203, -28.20702496313861474, 7.002103980607166989 ) ) ;
#17418 = CARTESIAN_POINT ( 'NONE',  ( 80.00358288781701788, 64.08847832824501722, 3.683925914261491741 ) ) ;
#17419 = CARTESIAN_POINT ( 'NONE',  ( 23.18011674250855236, 1.027085359276848298, 5.502131735125781908 ) ) ;
#17421 = EDGE_LOOP ( 'NONE', ( #24491, #12628, #22785, #11614 ) ) ;
#17420 = CARTESIAN_POINT ( 'NONE',  ( -59.00110696496997775, 28.68040728033253473, 6.999999999999999112 ) ) ;
#17422 = CARTESIAN_POINT ( 'NONE',  ( -21.07867591359219617, -26.64985754041175525, 6.700000000000000178 ) ) ;
#17424 = CARTESIAN_POINT ( 'NONE',  ( -63.08758708074093136, 38.76906266698303227, -4.000000000000000000 ) ) ;
#17423 = LINE ( 'NONE', #2232, #18641 ) ;
#17425 = CARTESIAN_POINT ( 'NONE',  ( -63.71197174466732349, 35.78007194159061299, -7.175960652854968203 ) ) ;
#17426 = CARTESIAN_POINT ( 'NONE',  ( -36.44874870218064444, -26.64985754041175525, 6.700000000000000178 ) ) ;
#17427 = DIRECTION ( 'NONE',  ( 0.000000000000000000, 0.000000000000000000, 1.000000000000000000 ) ) ;
#17428 = CARTESIAN_POINT ( 'NONE',  ( 21.77142106763977125, 5.727955254944006924, -3.425362973661377985 ) ) ;
#17429 = ORIENTED_EDGE ( 'NONE', *, *, #35988, .F. ) ;
#17430 = CARTESIAN_POINT ( 'NONE',  ( 5.123514540229139769, -30.22567137187272124, 7.785344483711591934 ) ) ;
#17431 = EDGE_CURVE ( 'NONE', #20650, #19304, #36544, .T. ) ;
#17432 = AXIS2_PLACEMENT_3D ( 'NONE', #8548, #20495, #30605 ) ;
#17433 = CARTESIAN_POINT ( 'NONE',  ( 22.80834877297060004, -6.429644848144123515, 3.896382617761176892 ) ) ;
#17434 = AXIS2_PLACEMENT_3D ( 'NONE', #29102, #13443, #26018 ) ;
#17435 = CARTESIAN_POINT ( 'NONE',  ( -72.95330471031414277, 33.71485196875532608, -46.17089178453873188 ) ) ;
#17436 = CARTESIAN_POINT ( 'NONE',  ( 79.64807995744904190, 65.91648781524679634, 2.476693319890303613 ) ) ;
#17437 = CARTESIAN_POINT ( 'NONE',  ( 84.61987491094994596, 3.070148169510762415, -1.277140785624046426 ) ) ;
#17438 = DIRECTION ( 'NONE',  ( -0.4999999999999986122, 0.000000000000000000, 0.8660254037844394848 ) ) ;
#17439 = ORIENTED_EDGE ( 'NONE', *, *, #14666, .F. ) ;
#17440 = CARTESIAN_POINT ( 'NONE',  ( -0.1940712780794633940, -32.51289061680132875, 7.013842709614101167 ) ) ;
#17441 = AXIS2_PLACEMENT_3D ( 'NONE', #24839, #21752, #37386 ) ;
#17442 = DIRECTION ( 'NONE',  ( 1.000000000000000000, 0.000000000000000000, 0.000000000000000000 ) ) ;
#17443 = EDGE_CURVE ( 'NONE', #23822, #13567, #26646, .T. ) ;
#17444 = CARTESIAN_POINT ( 'NONE',  ( 15.28076414829719099, -3.924379092781201450, -2.583448059524448226 ) ) ;
#17445 = CARTESIAN_POINT ( 'NONE',  ( 36.19345537505340360, -2.233535067971714305, -5.855262071939852042 ) ) ;
#17446 = CYLINDRICAL_SURFACE ( 'NONE', #2318, 3.784187430299790211 ) ;
#17447 = CARTESIAN_POINT ( 'NONE',  ( 24.12089549473325789, 0.5573315953133365364, -5.091603771319967109 ) ) ;
#17448 = CARTESIAN_POINT ( 'NONE',  ( -0.4949140130731182752, -26.97364919215634771, 7.756377446753162985 ) ) ;
#17449 = EDGE_LOOP ( 'NONE', ( #7077, #5896, #19940, #14741 ) ) ;
#17450 = CARTESIAN_POINT ( 'NONE',  ( 2.867385692375432171, -32.85781164720339120, 7.781480525794718162 ) ) ;
#17451 = EDGE_CURVE ( 'NONE', #4930, #17020, #8870, .T. ) ;
#17452 = EDGE_CURVE ( 'NONE', #10191, #26363, #25009, .T. ) ;
#17453 = DIRECTION ( 'NONE',  ( 0.000000000000000000, -0.000000000000000000, -1.000000000000000000 ) ) ;
#17454 = EDGE_CURVE ( 'NONE', #18413, #4851, #5308, .T. ) ;
#17455 = CARTESIAN_POINT ( 'NONE',  ( 5.026473753875771777, -28.48304391371080158, 7.761113333116787416 ) ) ;
#17456 = EDGE_LOOP ( 'NONE', ( #4521, #10603, #19950, #34596 ) ) ;
#17457 = EDGE_LOOP ( 'NONE', ( #3220, #34909, #29586, #20058, #15725 ) ) ;
#17458 = CARTESIAN_POINT ( 'NONE',  ( 33.68527224689047017, -3.841537723288600326, 5.136372516007956968 ) ) ;
#17459 = DIRECTION ( 'NONE',  ( 1.000000000000000000, 0.000000000000000000, 0.000000000000000000 ) ) ;
#17460 = CARTESIAN_POINT ( 'NONE',  ( 66.27376694609004915, 57.73522568913436004, -4.000000000000000000 ) ) ;
#17461 = ORIENTED_EDGE ( 'NONE', *, *, #22935, .F. ) ;
#17462 = CARTESIAN_POINT ( 'NONE',  ( 3.442434176459446160, -26.65012155745640499, 6.894806418505343260 ) ) ;
#17463 = ORIENTED_EDGE ( 'NONE', *, *, #2067, .F. ) ;
#17464 = VECTOR ( 'NONE', #134, 1000.000000000000000 ) ;
#17465 = ORIENTED_EDGE ( 'NONE', *, *, #22520, .T. ) ;
#17466 = CARTESIAN_POINT ( 'NONE',  ( -0.1391297599626309944, -34.30339127416094414, 7.013842709614101167 ) ) ;
#17467 = ORIENTED_EDGE ( 'NONE', *, *, #27237, .F. ) ;
#17468 = LINE ( 'NONE', #17072, #34606 ) ;
#17469 = VERTEX_POINT ( 'NONE', #566 ) ;
#17470 = CARTESIAN_POINT ( 'NONE',  ( 4.324299927142673639, -27.40773287891062182, 7.782167645815905033 ) ) ;
#17471 = ORIENTED_EDGE ( 'NONE', *, *, #1751, .T. ) ;
#17472 = CARTESIAN_POINT ( 'NONE',  ( 22.16804255864639117, 4.482405448724880337, 3.705173013356440670 ) ) ;
#17473 = VECTOR ( 'NONE', #4175, 1000.000000000000000 ) ;
#17474 = CARTESIAN_POINT ( 'NONE',  ( 81.94850308769507308, 64.73378216408549690, -2.360008641315554545 ) ) ;
#17475 = CARTESIAN_POINT ( 'NONE',  ( 4.459022997797871035, -27.41600137469124832, 7.753200566781599079 ) ) ;
#17476 = ORIENTED_EDGE ( 'NONE', *, *, #40064, .F. ) ;
#17478 = CARTESIAN_POINT ( 'NONE',  ( 1.081065130916230466, -26.22681238842248064, 7.661510568013099487 ) ) ;
#17477 = CARTESIAN_POINT ( 'NONE',  ( -62.92837670882106238, -39.37473357531882101, 6.000000000000000000 ) ) ;
#17479 = CARTESIAN_POINT ( 'NONE',  ( -1.798349965106823989, -29.47546963991379698, 6.863805608295730387 ) ) ;
#17480 = CARTESIAN_POINT ( 'NONE',  ( 73.81116006253010653, 62.20691382096256206, 3.564124015814260638 ) ) ;
#17481 = CARTESIAN_POINT ( 'NONE',  ( 24.28285221899144375, 2.481502257502904651, -4.080882954547480956 ) ) ;
#17482 = ORIENTED_EDGE ( 'NONE', *, *, #23971, .F. ) ;
#17483 = LINE ( 'NONE', #38719, #35944 ) ;
#17484 = LINE ( 'NONE', #17091, #16213 ) ;
#17485 = DIRECTION ( 'NONE',  ( 1.682730792515357087E-16, -1.000000000000000000, 0.000000000000000000 ) ) ;
#17486 = CARTESIAN_POINT ( 'NONE',  ( 5.198039085808181525, -29.69173459304409946, 7.754798119455333705 ) ) ;
#17487 = CARTESIAN_POINT ( 'NONE',  ( 1.700390093233090871, -29.56993018339339940, 7.800000000000000711 ) ) ;
#17488 = CARTESIAN_POINT ( 'NONE',  ( 81.67793621607884802, 64.59267988934881544, 2.776691787112188337 ) ) ;
#17489 = CARTESIAN_POINT ( 'NONE',  ( 86.52980085923458375, 1.163345319512251841, 5.105528906334227734 ) ) ;
#17490 = CARTESIAN_POINT ( 'NONE',  ( 28.07449379822080004, 1.807001228253011016, 3.913063849393144888 ) ) ;
#17491 = PRODUCT_DEFINITION ( 'UNKNOWN', '', #34732, #6117 ) ;
#17492 = LINE ( 'NONE', #36862, #6316 ) ;
#17493 = CARTESIAN_POINT ( 'NONE',  ( -72.38040341225585905, -46.72818906933961358, 9.894038184624683652 ) ) ;
#17494 = CARTESIAN_POINT ( 'NONE',  ( -72.84815947045233031, 2.429809908903064919, -10.96147798754375202 ) ) ;
#17495 = VERTEX_POINT ( 'NONE', #34553 ) ;
#17496 = CARTESIAN_POINT ( 'NONE',  ( 14.74399611399054955, -5.056622873111205507, 2.496408223985688402 ) ) ;
#17497 = CARTESIAN_POINT ( 'NONE',  ( 0.1007194770999123301, -26.45688377920343015, 7.011627023500184741 ) ) ;
#17498 = CARTESIAN_POINT ( 'NONE',  ( 35.79004886699985377, -3.279176249207559568, -5.792300729934813930 ) ) ;
#17499 = FACE_OUTER_BOUND ( 'NONE', #3601, .T. ) ;
#17500 = CARTESIAN_POINT ( 'NONE',  ( 6.126843302897349020, -31.19539656904077418, 7.635761828346577573 ) ) ;
#17501 = PLANE ( 'NONE',  #1372 ) ;
#17502 = AXIS2_PLACEMENT_3D ( 'NONE', #15692, #69, #2552 ) ;
#17503 = DIRECTION ( 'NONE',  ( 0.000000000000000000, 0.000000000000000000, 1.000000000000000000 ) ) ;
#17504 = ADVANCED_FACE ( 'NONE', ( #37799 ), #25663, .F. ) ;
#17505 = DIRECTION ( 'NONE',  ( 1.000000000000000000, 0.000000000000000000, -0.000000000000000000 ) ) ;
#17506 = EDGE_CURVE ( 'NONE', #32438, #31847, #17525, .T. ) ;
#17507 = ORIENTED_EDGE ( 'NONE', *, *, #4600, .T. ) ;
#17508 = CARTESIAN_POINT ( 'NONE',  ( 34.45373390281926618, -1.156888603319897513, 5.566325156673125996 ) ) ;
#17509 = CARTESIAN_POINT ( 'NONE',  ( -69.92837670882107659, -0.7829914368874777431, 5.928123921495636495 ) ) ;
#17510 = CARTESIAN_POINT ( 'NONE',  ( 67.47898117768387749, 58.07151159967423126, -3.997009152755514272 ) ) ;
#17511 = DIRECTION ( 'NONE',  ( -0.000000000000000000, -0.000000000000000000, 1.000000000000000000 ) ) ;
#17512 = VERTEX_POINT ( 'NONE', #10005 ) ;
#17513 = CARTESIAN_POINT ( 'NONE',  ( -30.87867591359218977, -26.64985754041175525, 6.800000000000000711 ) ) ;
#17514 = CARTESIAN_POINT ( 'NONE',  ( 77.73224247307464907, 65.38057827825358004, 2.040387096976575609 ) ) ;
#17515 = CARTESIAN_POINT ( 'NONE',  ( 0.9770400785565759305, -32.89210785486953625, 6.865312560952602894 ) ) ;
#17516 = CARTESIAN_POINT ( 'NONE',  ( -1.475752358162186084, -28.35661785261500967, 6.889465824494256374 ) ) ;
#17517 = CARTESIAN_POINT ( 'NONE',  ( -1.699475091297747653, -29.53965268324751747, 7.782167645815905033 ) ) ;
#17518 = ORIENTED_EDGE ( 'NONE', *, *, #9092, .T. ) ;
#17519 = CARTESIAN_POINT ( 'NONE',  ( 24.06122720769042900, 3.344954272100802761, 3.221752643096582158 ) ) ;
#17520 = CARTESIAN_POINT ( 'NONE',  ( 81.96245566837727381, 61.96131850323955348, -1.129532193886523261 ) ) ;
#17521 = CARTESIAN_POINT ( 'NONE',  ( 81.04779914310620370, 62.47515088512101755, 3.146509185145925258 ) ) ;
#17522 = AXIS2_PLACEMENT_3D ( 'NONE', #11619, #40050, #36159 ) ;
#17523 = CARTESIAN_POINT ( 'NONE',  ( 14.37770146410593597, -5.023675042449286643, -2.500000000000009326 ) ) ;
#17524 = CARTESIAN_POINT ( 'NONE',  ( 78.50009633871027859, 63.24008633025189852, -3.804514705604310709 ) ) ;
#17525 = B_SPLINE_CURVE_WITH_KNOTS ( 'NONE', 3,
 ( #37594, #15369, #12280, #6732, #6325, #31849, #18873, #31445, #3267, #3869, #28959, #22588, #6928, #13293, #16385, #19490, #762, #32064, #25866 ),
 .UNSPECIFIED., .F., .F.,
 ( 4, 3, 3, 3, 3, 3, 4 ),
 ( 2.168404344971008868E-19, 2.546128104244468310E-05, 5.711050680484036374E-05, 8.113074941675828202E-05, 0.0001053129305727062515, 0.0001360598016347037195, 0.0001612931755713731025 ),
 .UNSPECIFIED. ) ;
#17527 = DIRECTION ( 'NONE',  ( -0.000000000000000000, -0.000000000000000000, 1.000000000000000000 ) ) ;
#17526 = CARTESIAN_POINT ( 'NONE',  ( 25.40522689125253564, 0.6233671799178808204, 4.602606971976870298 ) ) ;
#17528 = AXIS2_PLACEMENT_3D ( 'NONE', #958, #35937, #16976 ) ;
#17529 = CARTESIAN_POINT ( 'NONE',  ( 81.00465555258324457, 64.24153452434936185, -3.375310687856056813 ) ) ;
#17530 = CARTESIAN_POINT ( 'NONE',  ( 77.99157368707381011, 64.87245838797727515, 2.976941560848442858 ) ) ;
#17531 = AXIS2_PLACEMENT_3D ( 'NONE', #39740, #15031, #34771 ) ;
#17532 = ORIENTED_EDGE ( 'NONE', *, *, #32486, .F. ) ;
#17533 = ORIENTED_EDGE ( 'NONE', *, *, #15727, .T. ) ;
#17534 = AXIS2_PLACEMENT_3D ( 'NONE', #32473, #3888, #38631 ) ;
#17535 = B_SPLINE_CURVE_WITH_KNOTS ( 'NONE', 3,
 ( #5154, #29861, #30691, #5559, #14599, #11303, #27376, #36245, #2284, #26976, #18100, #11108, #26780, #8219, #2498, #36850, #39521, #36647, #36054, #33782, #8426, #21210, #30478, #27171, #1675, #2087, #23868, #20790, #8022, #20382, #33385, #14808, #21004, #11712, #17282, #32961, #39115, #39318, #14407, #23679, #24288, #17691, #26575, #10911 ),
 .UNSPECIFIED., .F., .F.,
 ( 4, 1, 1, 2, 2, 1, 1, 1, 1, 1, 1, 1, 1, 2, 2, 1, 1, 1, 1, 1, 1, 2, 2, 1, 1, 1, 1, 1, 2, 2, 1, 1, 1, 4 ),
 ( 0.000000000000000000, 0.2462456440929807477, 0.2481694381874572086, 0.2491313352346954668, 0.2500932322819336973, 0.2539408204708873407, 0.2616359968487950716, 0.2770263496046105334, 0.3078070551162413460, 0.3693684661395030822, 0.4924912881860259994, 0.4963388763749802535, 0.4982626704694577136, 0.4992245675166965269, 0.5001864645639352291, 0.5078816409418428490, 0.5232719936976579778, 0.5540526992092877911, 0.6156141102325467518, 0.7387369322790644510, 0.7464321086569721819, 0.7483559027514491424, 0.7502796968459262139, 0.7541272850348799128, 0.7695176377906951526, 0.8002983433023260762, 0.8618597543255873683, 0.8695549307034944331, 0.8734025188924475769, 0.8753263129869242043, 0.8772501070814008317, 0.8926404598372128518, 0.9234211653488365590, 0.9849825763720841953 ),
 .UNSPECIFIED. ) ;
#17536 = EDGE_CURVE ( 'NONE', #38011, #30864, #35156, .T. ) ;
#17537 = CARTESIAN_POINT ( 'NONE',  ( -0.8255983619643308957, -27.29410358292636118, 7.757178535559533294 ) ) ;
#17538 = CARTESIAN_POINT ( 'NONE',  ( 81.72179206571547638, 61.68197623675726504, 1.214491505233688873 ) ) ;
#17540 = CARTESIAN_POINT ( 'NONE',  ( 82.38753728249152175, 5.816132372599501110, 5.999999999999998224 ) ) ;
#17539 = DIRECTION ( 'NONE',  ( 0.000000000000000000, 0.000000000000000000, 1.000000000000000000 ) ) ;
#17541 = CARTESIAN_POINT ( 'NONE',  ( 23.94338804316802438, 3.829326634665836782, 2.990621344434266415 ) ) ;
#17542 = CARTESIAN_POINT ( 'NONE',  ( -1.767452271763144012, -30.04337931387000893, 6.870724624169667116 ) ) ;
#17543 = CARTESIAN_POINT ( 'NONE',  ( -34.24874870218063450, -26.64985754041175525, 6.700000000000000178 ) ) ;
#17544 = VERTEX_POINT ( 'NONE', #30881 ) ;
#17545 = DIRECTION ( 'NONE',  ( -0.9848077530122069101, -0.1736481776669374644, -0.000000000000000000 ) ) ;
#17546 = CARTESIAN_POINT ( 'NONE',  ( 23.05616258268533159, 0.3493913546029596695, -5.956410236909607470 ) ) ;
#17547 = ADVANCED_FACE ( 'NONE', ( #8413 ), #20987, .F. ) ;
#17548 = CARTESIAN_POINT ( 'NONE',  ( 10.58508780786439374, 19.59913305159139441, -2.500000000000000000 ) ) ;
#17549 = VERTEX_POINT ( 'NONE', #8200 ) ;
#17550 = CARTESIAN_POINT ( 'NONE',  ( 0.9719320429316903320, -25.36088087325603624, 7.635761828346577573 ) ) ;
#17551 = LINE ( 'NONE', #14470, #20999 ) ;
#17552 = CYLINDRICAL_SURFACE ( 'NONE', #36731, 10.00000000000000533 ) ;
#17553 = CARTESIAN_POINT ( 'NONE',  ( 37.18584374690863115, -2.963240108125716699, -5.999995304506872351 ) ) ;
#17554 = DIRECTION ( 'NONE',  ( 0.000000000000000000, -1.000000000000000000, 0.000000000000000000 ) ) ;
#17555 = CARTESIAN_POINT ( 'NONE',  ( 3.340387623678102713, -32.66193850451435310, 6.867199677474201458 ) ) ;
#17556 = CARTESIAN_POINT ( 'NONE',  ( -1.096077277123481686, -31.67463417101835077, 6.989977667959449192 ) ) ;
#17557 = CARTESIAN_POINT ( 'NONE',  ( 1.700390093233090871, -29.56993018339339940, 7.750000000000000888 ) ) ;
#17558 = CARTESIAN_POINT ( 'NONE',  ( -2.716326236424497775, -26.78549066711456916, 6.954324564059724878 ) ) ;
#17559 = CARTESIAN_POINT ( 'NONE',  ( -2.496911308493820147, -30.36501393308138574, 7.695279973900954751 ) ) ;
#17560 = EDGE_CURVE ( 'NONE', #9646, #11704, #10, .T. ) ;
#17561 = VERTEX_POINT ( 'NONE', #5544 ) ;
#17562 = AXIS2_PLACEMENT_3D ( 'NONE', #32652, #13703, #23574 ) ;
#17563 = CARTESIAN_POINT ( 'NONE',  ( 66.27376694608996388, 57.73522568913447373, 4.000000000000000000 ) ) ;
#17564 = CARTESIAN_POINT ( 'NONE',  ( 71.58333764992288195, 61.16654152266917777, -3.647993048544889039 ) ) ;
#17565 = AXIS2_PLACEMENT_3D ( 'NONE', #7532, #7332, #13912 ) ;
#17566 = CARTESIAN_POINT ( 'NONE',  ( 3.977772666037320715, -27.04534534285276592, 7.754798119455333705 ) ) ;
#17567 = VERTEX_POINT ( 'NONE', #8615 ) ;
#17568 = CARTESIAN_POINT ( 'NONE',  ( 86.38407091574619301, -0.4420343715668084150, 5.843987706619403255 ) ) ;
#17569 = CARTESIAN_POINT ( 'NONE',  ( 0.1449207719380061765, -26.54659038131189774, 6.876076431790004939 ) ) ;
#17570 = CARTESIAN_POINT ( 'NONE',  ( 3.055600241130194572, -26.45169019916221131, 6.979335674598005745 ) ) ;
#17571 = CARTESIAN_POINT ( 'NONE',  ( -0.8610712181068592708, -27.18477818879997088, 6.998987538705433664 ) ) ;
#17572 = CONTEXT_DEPENDENT_SHAPE_REPRESENTATION ( #25808, #38800 ) ;
#17573 = DIRECTION ( 'NONE',  ( -0.9848077530122092416, 0.1736481776669241694, -0.000000000000000000 ) ) ;
#17574 = DIRECTION ( 'NONE',  ( 1.000000000000000000, 0.000000000000000000, 0.000000000000000000 ) ) ;
#17575 = CARTESIAN_POINT ( 'NONE',  ( 5.200390093233090205, -29.56993018339339940, 7.620413589471895399 ) ) ;
#17576 = ORIENTED_EDGE ( 'NONE', *, *, #31764, .T. ) ;
#17577 = CARTESIAN_POINT ( 'NONE',  ( 79.89038670178254620, 63.31421865134938542, -3.734652355492745102 ) ) ;
#17578 = VECTOR ( 'NONE', #34155, 1000.000000000000000 ) ;
#17579 = CARTESIAN_POINT ( 'NONE',  ( 17.55902072822312832, 11.95912221219358607, -2.500000000000012434 ) ) ;
#17580 = ADVANCED_FACE ( 'NONE', ( #27361 ), #27765, .T. ) ;
#17581 = CARTESIAN_POINT ( 'NONE',  ( 80.12334914806359620, 63.07862483458217895, 3.671038198312436496 ) ) ;
#17583 = VERTEX_POINT ( 'NONE', #36834 ) ;
#17582 = CARTESIAN_POINT ( 'NONE',  ( 0.02512807029999888919, -32.53672186615392548, 7.257242401810563237 ) ) ;
#17584 = AXIS2_PLACEMENT_3D ( 'NONE', #31457, #16992, #26086 ) ;
#17585 = DIRECTION ( 'NONE',  ( 1.000000000000000000, 0.000000000000000000, 0.000000000000000000 ) ) ;
#17586 = DIRECTION ( 'NONE',  ( -0.000000000000000000, -0.000000000000000000, -1.000000000000000000 ) ) ;
#17587 = EDGE_CURVE ( 'NONE', #12705, #29312, #17671, .T. ) ;
#17588 = CARTESIAN_POINT ( 'NONE',  ( 21.85643539959774273, 11.92045248574714300, 0.01447246376323708950 ) ) ;
#17589 = AXIS2_PLACEMENT_3D ( 'NONE', #26399, #10721, #35871 ) ;
#17590 = EDGE_LOOP ( 'NONE', ( #27635, #22047, #39702, #34126, #16248 ) ) ;
#17591 = CARTESIAN_POINT ( 'NONE',  ( -80.17799140349276854, 10.47773439577431631, 6.111419866882078722 ) ) ;
#17592 = EDGE_CURVE ( 'NONE', #8931, #4265, #5631, .T. ) ;
#17593 = CARTESIAN_POINT ( 'NONE',  ( 14.63786011423607114, -4.769655762138079069, 2.500000000000003109 ) ) ;
#17594 = CARTESIAN_POINT ( 'NONE',  ( -79.46433441440639456, 10.38016200751361851, -7.169073381784508925 ) ) ;
#17595 = CARTESIAN_POINT ( 'NONE',  ( 1.535796139241240255, -32.96595391691614196, 6.876076431790004939 ) ) ;
#17596 = CARTESIAN_POINT ( 'NONE',  ( 2.354198823195432055, -26.23337563047396870, 6.880147297696980857 ) ) ;
#17597 = CARTESIAN_POINT ( 'NONE',  ( 78.90480995596031732, 66.05426212177788159, 1.786209778413370586 ) ) ;
#17598 = CARTESIAN_POINT ( 'NONE',  ( -1.532840524546014160, -30.62170260317305903, 7.759451378593097637 ) ) ;
#17599 = LINE ( 'NONE', #36163, #32562 ) ;
#17600 = DIRECTION ( 'NONE',  ( 0.000000000000000000, 0.000000000000000000, 1.000000000000000000 ) ) ;
#17601 = CARTESIAN_POINT ( 'NONE',  ( 0.6746755240984175783, -26.22359730851838933, 6.998987538705434552 ) ) ;
#17602 = ADVANCED_BREP_SHAPE_REPRESENTATION ( '', ( #12327, #30744 ), #15591 ) ;
#17603 = CARTESIAN_POINT ( 'NONE',  ( 4.428600589446192615, -27.37744993431208940, 6.867280401193706751 ) ) ;
#17604 = CARTESIAN_POINT ( 'NONE',  ( 87.91080083688075320, -0.3878594015929205940, 3.341311120819375979 ) ) ;
#17605 = CARTESIAN_POINT ( 'NONE',  ( -9.078675913592196167, -26.64985754041175525, 6.700000000000000178 ) ) ;
#17606 = EDGE_CURVE ( 'NONE', #26569, #22022, #4216, .T. ) ;
#17607 = ORIENTED_EDGE ( 'NONE', *, *, #33161, .F. ) ;
#17608 = AXIS2_PLACEMENT_3D ( 'NONE', #26834, #36306, #36111 ) ;
#17609 = CARTESIAN_POINT ( 'NONE',  ( 67.99537475662653208, 58.47140781303536983, 3.994255761866590149 ) ) ;
#17610 = CARTESIAN_POINT ( 'NONE',  ( 36.98008712529284026, -2.957219606516312993, 5.978034981325530239 ) ) ;
#17611 = ORIENTED_EDGE ( 'NONE', *, *, #6055, .T. ) ;
#17612 = CARTESIAN_POINT ( 'NONE',  ( -71.92837670882106238, -42.87473357531881391, -1.732050807568860318 ) ) ;
#17613 = CARTESIAN_POINT ( 'NONE',  ( 88.63860240521751166, -1.205360666695063365, 1.162049942889349818 ) ) ;
#17615 = CARTESIAN_POINT ( 'NONE',  ( 32.83291512613813268, -0.9452453669511491352, -5.330768491123616393 ) ) ;
#17614 = CARTESIAN_POINT ( 'NONE',  ( -71.19005252498740788, -21.75701227484909950, 5.995519781525873171 ) ) ;
#17616 = DIRECTION ( 'NONE',  ( -0.6427876096865327016, -0.7660444431189835646, -0.000000000000000000 ) ) ;
#17617 = CARTESIAN_POINT ( 'NONE',  ( -1.608892841364319759, -28.78974341809173509, 7.006423389747791219 ) ) ;
#17618 = CARTESIAN_POINT ( 'NONE',  ( 2.348307190418675638, -26.14505435796186461, 7.785096263473211486 ) ) ;
#17619 = CARTESIAN_POINT ( 'NONE',  ( -0.5782875761460892772, -32.22655866202281061, 6.887161170156908874 ) ) ;
#17620 = AXIS2_PLACEMENT_3D ( 'NONE', #11380, #15300, #14475 ) ;
#17621 = EDGE_CURVE ( 'NONE', #12163, #7910, #4947, .T. ) ;
#17622 = ORIENTED_EDGE ( 'NONE', *, *, #6144, .F. ) ;
#17623 = CARTESIAN_POINT ( 'NONE',  ( -71.83651116356016075, -21.21610000639230975, 5.943034864274126861 ) ) ;
#17624 = ORIENTED_EDGE ( 'NONE', *, *, #15363, .T. ) ;
#17625 = CARTESIAN_POINT ( 'NONE',  ( 80.94504091708289195, 61.55080574620870237, -2.311104455577556394 ) ) ;
#17626 = CARTESIAN_POINT ( 'NONE',  ( -1.639146693691649892, -28.93157757802832819, 6.894806418505346812 ) ) ;
#17627 = CARTESIAN_POINT ( 'NONE',  ( 80.97304215327375232, 61.92799980795010839, 2.787474064117264838 ) ) ;
#17628 = CARTESIAN_POINT ( 'NONE',  ( 24.08422046648111348, 0.7197875013252986731, 5.070242109043855194 ) ) ;
#17630 = VERTEX_POINT ( 'NONE', #26959 ) ;
#17629 = CARTESIAN_POINT ( 'NONE',  ( 4.732935735574231195, -27.83999033440608883, 7.778495531946297170 ) ) ;
#17631 = CARTESIAN_POINT ( 'NONE',  ( 73.62310697524999625, 61.12246817794784448, -3.899931323576832920 ) ) ;
#17632 = DIRECTION ( 'NONE',  ( 1.000000000000000000, 0.000000000000000000, 0.000000000000000000 ) ) ;
#17633 = VECTOR ( 'NONE', #31164, 1000.000000000000000 ) ;
#17634 =( BOUNDED_CURVE ( )  B_SPLINE_CURVE ( 3, ( #31052, #8589, #39471, #39893 ),
 .UNSPECIFIED., .F., .F. ) 
 B_SPLINE_CURVE_WITH_KNOTS ( ( 4, 4 ),
 ( 1.347909859412853795, 1.396263401595463360 ),
 .UNSPECIFIED. ) 
 CURVE ( )  GEOMETRIC_REPRESENTATION_ITEM ( )  RATIONAL_B_SPLINE_CURVE ( ( 1.000000000000000000, 0.9998051707368829089, 0.9998051707368829089, 1.000000000000000000 ) ) 
 REPRESENTATION_ITEM ( '' )  );
#17636 = CARTESIAN_POINT ( 'NONE',  ( 3.554700302571109916, -26.60177950712765593, 7.754798119455333705 ) ) ;
#17635 = CARTESIAN_POINT ( 'NONE',  ( 36.10284116201629701, 0.9159659085930716982, 5.999999999999999112 ) ) ;
#17637 = FACE_OUTER_BOUND ( 'NONE', #27157, .T. ) ;
#17638 = ADVANCED_FACE ( 'NONE', ( #5138 ), #15461, .T. ) ;
#17639 = FACE_OUTER_BOUND ( 'NONE', #15281, .T. ) ;
#17640 = CARTESIAN_POINT ( 'NONE',  ( 22.30947672616612110, 4.711638434871365355, -3.402558136683496048 ) ) ;
#17641 = VERTEX_POINT ( 'NONE', #20564 ) ;
#17642 = FACE_OUTER_BOUND ( 'NONE', #30979, .T. ) ;
#17643 = EDGE_CURVE ( 'NONE', #23554, #25871, #20036, .T. ) ;
#17644 = ORIENTED_EDGE ( 'NONE', *, *, #1049, .F. ) ;
#17645 = CARTESIAN_POINT ( 'NONE',  ( 22.32070839933769690, 6.022037317923602195, -2.674548383380369376 ) ) ;
#17646 = CARTESIAN_POINT ( 'NONE',  ( -0.9695225508750403565, -31.83301800158153227, 7.749999999999998224 ) ) ;
#17647 = ORIENTED_EDGE ( 'NONE', *, *, #36071, .T. ) ;
#17648 = CARTESIAN_POINT ( 'NONE',  ( -8.878675913592189772, -26.64985754041175525, 6.700000000000000178 ) ) ;
#17649 = CARTESIAN_POINT ( 'NONE',  ( 81.16342859510598373, 63.93697670171856373, 3.375310687858766645 ) ) ;
#17650 = CARTESIAN_POINT ( 'NONE',  ( 87.06807637922989329, 0.009568187950425697044, -5.830412620327568796 ) ) ;
#17651 = CARTESIAN_POINT ( 'NONE',  ( 2.778259044425222868, -32.89982485500929954, 7.750000000000000888 ) ) ;
#17652 = VERTEX_POINT ( 'NONE', #17462 ) ;
#17653 = FACE_OUTER_BOUND ( 'NONE', #5546, .T. ) ;
#17654 = CARTESIAN_POINT ( 'NONE',  ( 5.056857618328627346, -29.02759656560906976, 6.894806418505346812 ) ) ;
#17655 = CARTESIAN_POINT ( 'NONE',  ( 17.05035514590630186, -3.238823860988104375, -2.847664724424037175 ) ) ;
#17656 = CARTESIAN_POINT ( 'NONE',  ( 21.25246063494507709, 3.318379548260936396, -3.523358493422822146 ) ) ;
#17657 = DIRECTION ( 'NONE',  ( 1.000000000000000000, 0.000000000000000000, -0.000000000000000000 ) ) ;
#17658 = CARTESIAN_POINT ( 'NONE',  ( 26.23190562806670201, 1.330159553823745400, -4.349047677718131055 ) ) ;
#17659 = CARTESIAN_POINT ( 'NONE',  ( 30.19012588776831052, -3.695353065752804866, -4.605591824749690311 ) ) ;
#17660 = VERTEX_POINT ( 'NONE', #14584 ) ;
#17661 = CARTESIAN_POINT ( 'NONE',  ( 33.68739442648515592, -3.100371856129508163, 5.464130651605732858 ) ) ;
#17662 = CARTESIAN_POINT ( 'NONE',  ( -1.211329843465634326, -27.81438207803897456, 6.880147297696979969 ) ) ;
#17663 = AXIS2_PLACEMENT_3D ( 'NONE', #27535, #12288, #31048 ) ;
#17664 = ORIENTED_EDGE ( 'NONE', *, *, #57, .T. ) ;
#17665 = ORIENTED_EDGE ( 'NONE', *, *, #38813, .F. ) ;
#17666 = CARTESIAN_POINT ( 'NONE',  ( 34.14266073545298497, -3.850829098075486456, 5.232169337272932985 ) ) ;
#17667 = CARTESIAN_POINT ( 'NONE',  ( -6.878675913592188884, -24.55319635012989110, 6.700000000000000178 ) ) ;
#17668 = CARTESIAN_POINT ( 'NONE',  ( 27.25263714637349466, -3.363254830459760925, -4.292962941291143864 ) ) ;
#17669 = CARTESIAN_POINT ( 'NONE',  ( -70.95330471031414277, 33.71485196875532608, 21.52833696633422988 ) ) ;
#17670 = ORIENTED_EDGE ( 'NONE', *, *, #35777, .F. ) ;
#17671 = LINE ( 'NONE', #11901, #17406 ) ;
#17672 = ORIENTED_EDGE ( 'NONE', *, *, #4112, .F. ) ;
#17673 = ORIENTED_EDGE ( 'NONE', *, *, #40496, .F. ) ;
#17674 = DIRECTION ( 'NONE',  ( 1.000000000000000000, 0.000000000000000000, 0.000000000000000000 ) ) ;
#17675 = CARTESIAN_POINT ( 'NONE',  ( -20.87867591359218977, -24.55319635012989110, 6.700000000000000178 ) ) ;
#17676 = CARTESIAN_POINT ( 'NONE',  ( 80.94990806105060699, 62.43782317439323037, -3.178394274514594997 ) ) ;
#17677 = CARTESIAN_POINT ( 'NONE',  ( 14.75054140592678920, -5.115303881675558273, 2.500062186397897790 ) ) ;
#17678 = ORIENTED_EDGE ( 'NONE', *, *, #37782, .T. ) ;
#17680 = CARTESIAN_POINT ( 'NONE',  ( -70.92837670882107659, -65.19654454972992141, 0.000000000000000000 ) ) ;
#17679 = CARTESIAN_POINT ( 'NONE',  ( 4.822972847261124407, -27.98895676671407173, 6.951256099901587326 ) ) ;
#17681 = ORIENTED_EDGE ( 'NONE', *, *, #28547, .F. ) ;
#17682 = ADVANCED_FACE ( 'NONE', ( #30054 ), #36428, .F. ) ;
#17683 = CARTESIAN_POINT ( 'NONE',  ( 22.98309003772910231, 3.680112614338335586, 3.663265023080902960 ) ) ;
#17684 = CARTESIAN_POINT ( 'NONE',  ( 82.01669802222831152, 64.37834105533548268, -2.512558077908312537 ) ) ;
#17685 = VECTOR ( 'NONE', #13225, 1000.000000000000000 ) ;
#17686 = EDGE_CURVE ( 'NONE', #5705, #13694, #3017, .T. ) ;
#17687 = DIRECTION ( 'NONE',  ( 0.3420201433256662704, 0.9396926207859093161, -0.000000000000000000 ) ) ;
#17688 = VERTEX_POINT ( 'NONE', #36630 ) ;
#17689 = PRODUCT_DEFINITION_SHAPE ( 'NONE', 'NONE',  #15152 ) ;
#17691 = CARTESIAN_POINT ( 'NONE',  ( 15.19171747855076937, -3.846800078502829567, -2.577432944240219292 ) ) ;
#17690 = LINE ( 'NONE', #24077, #10127 ) ;
#17692 = FACE_BOUND ( 'NONE', #12581, .T. ) ;
#17693 = CARTESIAN_POINT ( 'NONE',  ( 75.40715271138134312, 60.19559828969859439, 3.661998389317127511 ) ) ;
#17694 = CARTESIAN_POINT ( 'NONE',  ( 23.48117969904087232, 2.411688234495183103, -4.382658167535084637 ) ) ;
#17695 = ADVANCED_FACE ( 'NONE', ( #3706 ), #37234, .F. ) ;
#17696 = CYLINDRICAL_SURFACE ( 'NONE', #38535, 0.1000000000000028644 ) ;
#17697 = EDGE_CURVE ( 'NONE', #24389, #8458, #13501, .T. ) ;
#17698 = AXIS2_PLACEMENT_3D ( 'NONE', #32179, #13821, #16686 ) ;
#17699 = CARTESIAN_POINT ( 'NONE',  ( -2.217539137252236614, -26.10432465486971054, 7.013842709614101167 ) ) ;
#17700 = CARTESIAN_POINT ( 'NONE',  ( -1.250824363190944588, -27.88163718980674233, 7.635761828346577573 ) ) ;
#17701 = CARTESIAN_POINT ( 'NONE',  ( 81.68772813446398118, 64.20773789716577085, 2.952528780688829624 ) ) ;
#17702 = CARTESIAN_POINT ( 'NONE',  ( 86.96272348114096928, 0.6770660828398197273, -5.145113290124521122 ) ) ;
#17703 = CARTESIAN_POINT ( 'NONE',  ( 33.42314280165584961, -3.731500252021894948, -5.214789010484834897 ) ) ;
#17704 = CARTESIAN_POINT ( 'NONE',  ( 2.868207633511080434, -32.86935470785505231, 6.894806418505347700 ) ) ;
#17705 = CARTESIAN_POINT ( 'NONE',  ( 14.72985901586098834, -5.055727223184880437, 2.496285957478483919 ) ) ;
#17706 = CARTESIAN_POINT ( 'NONE',  ( 5.916497905674401814, -30.25835747790444330, 7.695279973900954751 ) ) ;
#17707 = CARTESIAN_POINT ( 'NONE',  ( 36.49090136167231435, -2.266358383019391187, -5.901685711910262810 ) ) ;
#17708 = CARTESIAN_POINT ( 'NONE',  ( -0.8241947473075555974, -27.29254761058917822, 7.754798119455333705 ) ) ;
#17709 = CARTESIAN_POINT ( 'NONE',  ( -9.078675913592196167, -26.64985754041175525, 6.700000000000000178 ) ) ;
#17710 = DIRECTION ( 'NONE',  ( 1.000000000000000000, 0.000000000000000000, 0.000000000000000000 ) ) ;
#17712 = VECTOR ( 'NONE', #40714, 1000.000000000000000 ) ;
#17711 = CARTESIAN_POINT ( 'NONE',  ( -2.248748702180634940, -25.49307895267003587, 6.700000000000000178 ) ) ;
#17713 = CARTESIAN_POINT ( 'NONE',  ( -12.34874870218063947, -25.49307895267003587, 6.700000000000000178 ) ) ;
#17714 = VERTEX_POINT ( 'NONE', #19323 ) ;
#17715 = CARTESIAN_POINT ( 'NONE',  ( 33.45644231954936032, -3.829387444398935969, 5.093826274657804021 ) ) ;
#17716 = DIRECTION ( 'NONE',  ( -0.000000000000000000, 1.000000000000000000, -0.000000000000000000 ) ) ;
#17717 = LINE ( 'NONE', #11739, #13249 ) ;
#17718 = CARTESIAN_POINT ( 'NONE',  ( -9.796229648729232409, -33.54387950140292673, 2.500000000000000000 ) ) ;
#17719 = ORIENTED_EDGE ( 'NONE', *, *, #1016, .F. ) ;
#17720 = DIRECTION ( 'NONE',  ( -0.000000000000000000, 0.000000000000000000, 1.000000000000000000 ) ) ;
#17721 = VECTOR ( 'NONE', #22565, 1000.000000000000114 ) ;
#17722 = CARTESIAN_POINT ( 'NONE',  ( 3.839274798992386550, -32.21287782106406183, 7.785172627573962778 ) ) ;
#17723 = CARTESIAN_POINT ( 'NONE',  ( 85.76276611814323303, 0.6947132229710382134, -5.930772436601586151 ) ) ;
#17724 = CARTESIAN_POINT ( 'NONE',  ( -80.92837670882107659, 2.429809908903242555, 15.50000000000000000 ) ) ;
#17725 = CARTESIAN_POINT ( 'NONE',  ( -1.699178655868960552, -29.51577928193538369, 7.785387725071490905 ) ) ;
#17726 = CARTESIAN_POINT ( 'NONE',  ( -1.321941654078521378, -31.33501114731328130, 7.749999999999999112 ) ) ;
#17727 = ORIENTED_EDGE ( 'NONE', *, *, #20824, .F. ) ;
#17728 = CARTESIAN_POINT ( 'NONE',  ( 21.71529350491948662, 6.299837801999743192, 3.203318375066928514 ) ) ;
#17729 = CARTESIAN_POINT ( 'NONE',  ( 81.35706873939176376, 65.93413826765579699, -1.000000000000000000 ) ) ;
#17730 = CARTESIAN_POINT ( 'NONE',  ( 80.41878079785790590, 63.93588341273047604, 3.625945587094184130 ) ) ;
#17731 = CARTESIAN_POINT ( 'NONE',  ( -0.09771614006683670972, -32.45555212220796193, 6.864276522220859711 ) ) ;
#17732 = ORIENTED_EDGE ( 'NONE', *, *, #3489, .F. ) ;
#17733 = CARTESIAN_POINT ( 'NONE',  ( 78.55649010480105687, 62.41317512920502963, -3.780406938340844736 ) ) ;
#17735 = CARTESIAN_POINT ( 'NONE',  ( 2.255912809263124874, -26.21562030886189731, 7.680992449362118890 ) ) ;
#17734 = CARTESIAN_POINT ( 'NONE',  ( 24.12314213337219471, 0.4937462159112996907, 5.095090315528720382 ) ) ;
#17736 = CARTESIAN_POINT ( 'NONE',  ( 79.18807306865505780, 66.05665914930281701, -1.983726836935526761 ) ) ;
#17737 = DIRECTION ( 'NONE',  ( 0.000000000000000000, 0.000000000000000000, 1.000000000000000000 ) ) ;
#17738 = CARTESIAN_POINT ( 'NONE',  ( 79.99044059672593221, 61.67469478680249750, 3.091829831932955575 ) ) ;
#17739 = EDGE_LOOP ( 'NONE', ( #21770, #28097, #29564, #15323 ) ) ;
#17740 = ORIENTED_EDGE ( 'NONE', *, *, #9159, .F. ) ;
#17741 = EDGE_CURVE ( 'NONE', #19582, #32758, #16228, .T. ) ;
#17742 = CIRCLE ( 'NONE', #38, 2.999999999999998668 ) ;
#17743 = EDGE_CURVE ( 'NONE', #24264, #15530, #881, .T. ) ;
#17744 = CARTESIAN_POINT ( 'NONE',  ( 36.40251230580387443, -3.583875492086917358, -5.773602733574922929 ) ) ;
#17745 = EDGE_CURVE ( 'NONE', #7170, #33227, #25101, .T. ) ;
#17746 = ORIENTED_EDGE ( 'NONE', *, *, #11125, .F. ) ;
#17747 = CARTESIAN_POINT ( 'NONE',  ( 79.32563386639218095, 66.29995228605849888, 1.174937739208267606 ) ) ;
#17749 = CARTESIAN_POINT ( 'NONE',  ( 14.69558838330753936, -3.003688195628454238, -6.000000000000000888 ) ) ;
#17748 = CARTESIAN_POINT ( 'NONE',  ( 4.326629237392442207, -31.88355676469063837, 6.865554069792296765 ) ) ;
#17750 = CARTESIAN_POINT ( 'NONE',  ( 29.35164812155991854, -2.438811642646435018, -5.575705495130315548 ) ) ;
#17751 = ORIENTED_EDGE ( 'NONE', *, *, #38760, .T. ) ;
#17752 = CARTESIAN_POINT ( 'NONE',  ( -80.88307586610955013, -6.600601063053268547, 1.034001549581234691 ) ) ;
#17753 = CARTESIAN_POINT ( 'NONE',  ( 23.05858422394668494, 0.3510769165348703313, -5.953811706270123238 ) ) ;
#17754 = CYLINDRICAL_SURFACE ( 'NONE', #5093, 15.73502530973474478 ) ;
#17755 = ORIENTED_EDGE ( 'NONE', *, *, #38021, .T. ) ;
#17756 = CARTESIAN_POINT ( 'NONE',  ( 4.995237956833183723, -30.75059844998224179, 7.750000000000001776 ) ) ;
#17757 = CARTESIAN_POINT ( 'NONE',  ( 5.170673138964259508, -29.11471587363884339, 6.880828092187099010 ) ) ;
#17758 = AXIS2_PLACEMENT_3D ( 'NONE', #35285, #26209, #4770 ) ;
#17759 = CARTESIAN_POINT ( 'NONE',  ( -72.12675090261940625, -48.04006991943428062, 9.928906425387692636 ) ) ;
#17760 = CARTESIAN_POINT ( 'NONE',  ( 25.73262918993416903, 2.635805330050151163, -3.523857060088606552 ) ) ;
#17761 = CARTESIAN_POINT ( 'NONE',  ( 30.86448711380490906, -3.396658003756702016, -4.948646710216845435 ) ) ;
#17762 = CARTESIAN_POINT ( 'NONE',  ( -60.75950795826495465, 23.17721540975219341, 12.50000000000000000 ) ) ;
#17763 = CARTESIAN_POINT ( 'NONE',  ( -73.16330946177717465, -60.53509472482659959, -3.871017079619738510 ) ) ;
#17764 = CARTESIAN_POINT ( 'NONE',  ( -72.42837670882107659, -47.31363652731821645, 5.809475019311128641 ) ) ;
#17765 = FACE_OUTER_BOUND ( 'NONE', #30486, .T. ) ;
#17766 = CARTESIAN_POINT ( 'NONE',  ( 1.905780558339014386, -26.16908768638748839, 7.386948897581449458 ) ) ;
#17767 = DIRECTION ( 'NONE',  ( 1.000000000000000000, 0.000000000000000000, 0.000000000000000000 ) ) ;
#17768 = CARTESIAN_POINT ( 'NONE',  ( 2.850561110411099275, -26.37038230420113649, 7.635761828346577573 ) ) ;
#17769 = CARTESIAN_POINT ( 'NONE',  ( 23.61768953064343179, 2.039297767802271899, -4.577865503187037888 ) ) ;
#17770 = VERTEX_POINT ( 'NONE', #31688 ) ;
#17771 = ORIENTED_EDGE ( 'NONE', *, *, #19410, .F. ) ;
#17772 = CARTESIAN_POINT ( 'NONE',  ( 66.57962043698374544, 57.80678959376348303, 3.999745625240549440 ) ) ;
#17773 = CARTESIAN_POINT ( 'NONE',  ( 69.50581201620700256, 59.72791825745761685, -3.883859131414829413 ) ) ;
#17774 = AXIS2_PLACEMENT_3D ( 'NONE', #4391, #38741, #14028 ) ;
#17775 = ORIENTED_EDGE ( 'NONE', *, *, #33482, .F. ) ;
#17776 = CARTESIAN_POINT ( 'NONE',  ( -1.078675913592196167, -26.64985754041175525, 6.700000000000000178 ) ) ;
#17777 = LINE ( 'NONE', #39609, #40328 ) ;
#17778 = CARTESIAN_POINT ( 'NONE',  ( -0.2487487021806331078, -26.64985754041175525, 6.700000000000000178 ) ) ;
#17779 = PRODUCT_DEFINITION_SHAPE ( 'NONE', 'NONE',  #32149 ) ;
#17780 = CARTESIAN_POINT ( 'NONE',  ( -0.8574700402111025133, -27.18092379207987719, 6.921725064902947366 ) ) ;
#17781 = ITEM_DEFINED_TRANSFORMATION ( 'NONE', 'NONE', #16926,  #30744 ) ;
#17782 = CARTESIAN_POINT ( 'NONE',  ( -34.44874870218064444, -26.64985754041175525, 6.700000000000000178 ) ) ;
#17783 = ORIENTED_EDGE ( 'NONE', *, *, #36814, .T. ) ;
#17784 = CARTESIAN_POINT ( 'NONE',  ( -1.749609906766908640, -29.56993018339339940, 7.750000000000000888 ) ) ;
#17785 = CARTESIAN_POINT ( 'NONE',  ( -6.878675913592188884, -26.64985754041175525, 6.800000000000000711 ) ) ;
#17786 = CARTESIAN_POINT ( 'NONE',  ( 22.26369084603574322, -3.082934178409861392, 3.582914324214749868 ) ) ;
#17787 = VECTOR ( 'NONE', #3305, 1000.000000000000114 ) ;
#17788 = ORIENTED_EDGE ( 'NONE', *, *, #35018, .T. ) ;
#17789 = CARTESIAN_POINT ( 'NONE',  ( 79.04765299714190974, 64.87162515256788708, -3.322373183921396578 ) ) ;
#17790 = CARTESIAN_POINT ( 'NONE',  ( 2.431875535358183793, -26.14722233025152676, 7.750000000000000888 ) ) ;
#17791 = B_SPLINE_CURVE_WITH_KNOTS ( 'NONE', 3,
 ( #6129, #15992, #31657, #28561, #369, #12904, #22397, #2655, #15174, #27732 ),
 .UNSPECIFIED., .F., .F.,
 ( 4, 3, 3, 4 ),
 ( 0.0002170292169044748620, 0.0002420761345916006457, 0.0002723302478207037807, 0.0002816811360866676396 ),
 .UNSPECIFIED. ) ;
#17792 = CARTESIAN_POINT ( 'NONE',  ( 81.67965074903506206, 61.82017115420519104, -1.781440269582274416 ) ) ;
#17793 = CARTESIAN_POINT ( 'NONE',  ( 80.80054865964804378, 61.51733283104051964, 2.392122129321804902 ) ) ;
#17794 = FACE_OUTER_BOUND ( 'NONE', #8223, .T. ) ;
#17795 = ADVANCED_FACE ( 'NONE', ( #3504 ), #16026, .T. ) ;
#17796 = CARTESIAN_POINT ( 'NONE',  ( 14.77315594796849574, 13.19392823276453441, -2.500000000000005773 ) ) ;
#17797 = CARTESIAN_POINT ( 'NONE',  ( 18.06312555530757180, 13.66100638925423638, 2.499999999999999112 ) ) ;
#17798 = CARTESIAN_POINT ( 'NONE',  ( 21.85643539959776049, -3.417000210761661272, 14.19984240075801374 ) ) ;
#17799 = ORIENTED_EDGE ( 'NONE', *, *, #1204, .F. ) ;
#17800 = CARTESIAN_POINT ( 'NONE',  ( -81.60310545337347321, 10.48532311983779231, 2.459591873363855985 ) ) ;
#17801 = CIRCLE ( 'NONE', #13888, 5.681288188914806803 ) ;
#17802 = CARTESIAN_POINT ( 'NONE',  ( 14.69558626228978149, -4.492521580652499402, 2.500000000002278622 ) ) ;
#17803 = CARTESIAN_POINT ( 'NONE',  ( -73.75202015018511759, 8.355648094992089270, -9.596423266730763402 ) ) ;
#17804 = CARTESIAN_POINT ( 'NONE',  ( 0.01209709964644558461, -32.52114463981743597, 7.635761828346577573 ) ) ;
#17805 = CARTESIAN_POINT ( 'NONE',  ( 34.79254740251967348, -3.836931395608193185, -5.375521320436218886 ) ) ;
#17806 = CARTESIAN_POINT ( 'NONE',  ( -1.740944944166762820, -30.15835019865512834, 7.778495531946297170 ) ) ;
#17807 = CARTESIAN_POINT ( 'NONE',  ( 14.69386405977045840, 12.90286227655693985, 2.499730877609119606 ) ) ;
#17808 = DIRECTION ( 'NONE',  ( -0.000000000000000000, -1.000000000000000000, -0.000000000000000000 ) ) ;
#17809 = VECTOR ( 'NONE', #4517, 1000.000000000000000 ) ;
#17810 = CARTESIAN_POINT ( 'NONE',  ( 0.6636879034114320230, -26.22699007480350986, 7.013842709614101167 ) ) ;
#17811 = FACE_OUTER_BOUND ( 'NONE', #31715, .T. ) ;
#17812 = CARTESIAN_POINT ( 'NONE',  ( 0.05705130999228511662, -26.47997509747052192, 7.754798119455333705 ) ) ;
#17813 = AXIS2_PLACEMENT_3D ( 'NONE', #5798, #8865, #14632 ) ;
#17814 = CARTESIAN_POINT ( 'NONE',  ( -0.4456138174198727153, -26.93275873432113343, 6.892063359921933419 ) ) ;
#17815 = PLANE ( 'NONE',  #6308 ) ;
#17816 = ORIENTED_EDGE ( 'NONE', *, *, #2166, .T. ) ;
#17817 = B_SPLINE_CURVE_WITH_KNOTS ( 'NONE', 3,
 ( #13484, #26059, #34938, #10395, #9991, #29339 ),
 .UNSPECIFIED., .F., .F.,
 ( 4, 2, 4 ),
 ( 0.001562288773108196386, 0.004630526322482777721, 0.007698763871857358838 ),
 .UNSPECIFIED. ) ;
#17818 = CARTESIAN_POINT ( 'NONE',  ( 67.80923286766689273, 58.07768331974902765, 3.990378031984522789 ) ) ;
#17819 = EDGE_CURVE ( 'NONE', #37746, #24052, #8195, .T. ) ;
#17820 = LINE ( 'NONE', #17612, #26678 ) ;
#17821 = CARTESIAN_POINT ( 'NONE',  ( 84.70654116317179216, 2.970325471579660981, -2.062712134826208299 ) ) ;
#17823 = CARTESIAN_POINT ( 'NONE',  ( 1.096693473209699121, -26.22395493079927320, 7.635761828346577573 ) ) ;
#17822 = CARTESIAN_POINT ( 'NONE',  ( 32.22946493318451644, -2.099509172777830557, 5.989391533279509794 ) ) ;
#17824 = CARTESIAN_POINT ( 'NONE',  ( -1.624037871885951390, -28.85698716789056206, 6.863904403958575706 ) ) ;
#17825 = CARTESIAN_POINT ( 'NONE',  ( 85.69091256600084705, 1.101904404422226147, 5.757845717007028519 ) ) ;
#17826 = DIRECTION ( 'NONE',  ( -0.000000000000000000, -0.000000000000000000, 1.000000000000000000 ) ) ;
#17827 = EDGE_LOOP ( 'NONE', ( #498, #7458, #11051, #27676, #38455 ) ) ;
#17828 = CARTESIAN_POINT ( 'NONE',  ( -70.40039547503687345, -21.63944369480664776, 5.989611775372475577 ) ) ;
#17829 = EDGE_CURVE ( 'NONE', #21972, #2270, #4978, .T. ) ;
#17830 = ORIENTED_EDGE ( 'NONE', *, *, #40093, .F. ) ;
#17831 = CARTESIAN_POINT ( 'NONE',  ( 79.73288524454797255, 64.30401648905855438, -3.644176963625960664 ) ) ;
#17832 = DIRECTION ( 'NONE',  ( -0.000000000000000000, -0.000000000000000000, 1.000000000000000000 ) ) ;
#17833 = CARTESIAN_POINT ( 'NONE',  ( 81.09158065085932776, 61.31869227828926938, 1.634613895560438124 ) ) ;
#17834 = CARTESIAN_POINT ( 'NONE',  ( 27.32771548703534137, 1.129468208573155552, 4.470271327343472656 ) ) ;
#17836 = ORIENTED_EDGE ( 'NONE', *, *, #5642, .T. ) ;
#17835 = CYLINDRICAL_SURFACE ( 'NONE', #1332, 0.09010775117052864658 ) ;
#17837 = CARTESIAN_POINT ( 'NONE',  ( 74.36844136632052482, 60.98005461696732254, -3.924711207976818717 ) ) ;
#17838 = VECTOR ( 'NONE', #19743, 1000.000000000000000 ) ;
#17839 = CARTESIAN_POINT ( 'NONE',  ( -70.79777098150788106, -21.78301052427940832, 6.000000000000010658 ) ) ;
#17840 = EDGE_CURVE ( 'NONE', #33660, #3598, #29000, .T. ) ;
#17842 = LINE ( 'NONE', #26922, #1927 ) ;
#17841 = CARTESIAN_POINT ( 'NONE',  ( 66.41194937274630661, -13.65448019739280028, 6.000000000000001776 ) ) ;
#17843 = CARTESIAN_POINT ( 'NONE',  ( 3.817924346030161509, -32.35669330361569962, 7.013842709614101167 ) ) ;
#17844 = CYLINDRICAL_SURFACE ( 'NONE', #511, 0.1000000000000028644 ) ;
#17845 = CARTESIAN_POINT ( 'NONE',  ( -1.587491370576900040, -30.73692578253573160, 7.781480525794717273 ) ) ;
#17846 = CARTESIAN_POINT ( 'NONE',  ( 22.65020874192035549, 4.493281994308780725, -3.164719311941372570 ) ) ;
#17847 = ORIENTED_EDGE ( 'NONE', *, *, #29714, .F. ) ;
#17848 = CARTESIAN_POINT ( 'NONE',  ( 5.100363281305461349, -29.55642757665872722, 7.635761828346577573 ) ) ;
#17849 = CARTESIAN_POINT ( 'NONE',  ( 23.98959816390508593, 3.209834647534565377, 4.521976212143768770 ) ) ;
#17850 = CARTESIAN_POINT ( 'NONE',  ( 21.86951112228127769, 3.097095171887178644, -3.923778634572244073 ) ) ;
#17851 = DIRECTION ( 'NONE',  ( 0.000000000000000000, 1.000000000000000000, 0.000000000000000000 ) ) ;
#17852 = CARTESIAN_POINT ( 'NONE',  ( -2.348748702180637693, -26.64985754041175525, 6.700000000000000178 ) ) ;
#17853 = CARTESIAN_POINT ( 'NONE',  ( 80.25728969398844015, 65.34460247849791870, 3.089171411838283809 ) ) ;
#17854 = CARTESIAN_POINT ( 'NONE',  ( 84.57490107788032674, 3.121871263001978924, -0.4841835102440271710 ) ) ;
#17855 = DIRECTION ( 'NONE',  ( 0.8831583674550994578, -0.4690749385695672791, 0.000000000000000000 ) ) ;
#17856 = ORIENTED_EDGE ( 'NONE', *, *, #13948, .F. ) ;
#17857 = CARTESIAN_POINT ( 'NONE',  ( -1.578737010731859902, -28.64489982150178449, 7.505001789837627335 ) ) ;
#17858 = ADVANCED_FACE ( 'NONE', ( #10049 ), #32110, .F. ) ;
#17859 = LINE ( 'NONE', #30440, #12478 ) ;
#17860 = CARTESIAN_POINT ( 'NONE',  ( 14.85674990071718682, -5.934158909055215148, -2.520779269183912596 ) ) ;
#17861 = CARTESIAN_POINT ( 'NONE',  ( 4.791866717558907141, -27.92896270571450756, 7.751599049952199394 ) ) ;
#17862 = DIRECTION ( 'NONE',  ( -0.7394003126383911217, -0.1303762246624254051, -0.6605219282605404585 ) ) ;
#17863 = CARTESIAN_POINT ( 'NONE',  ( 23.60906662612009299, 0.4468475687248973927, -5.506013801080326786 ) ) ;
#17864 = CARTESIAN_POINT ( 'NONE',  ( -0.4155616643037752800, -26.90858688352082595, 7.778050822775633755 ) ) ;
#17865 = VERTEX_POINT ( 'NONE', #22630 ) ;
#17866 = CARTESIAN_POINT ( 'NONE',  ( 29.09901106016964434, 0.3518894619724439732, 4.748002456818146477 ) ) ;
#17867 = CARTESIAN_POINT ( 'NONE',  ( 85.17388679999480416, 2.686372346413934409, 1.032998165733738816 ) ) ;
#17868 = ORIENTED_EDGE ( 'NONE', *, *, #1157, .F. ) ;
#17869 = EDGE_LOOP ( 'NONE', ( #20856, #14187, #14391, #16446 ) ) ;
#17871 = CARTESIAN_POINT ( 'NONE',  ( 35.22132403397331757, -1.046696322805372503, 5.410263585848889001 ) ) ;
#17870 = CARTESIAN_POINT ( 'NONE',  ( 81.02128870047407361, 63.12856183665077481, -3.380792992375200701 ) ) ;
#17872 = CARTESIAN_POINT ( 'NONE',  ( 26.17872147609876876, -2.762083417368125016, 4.292220639753399958 ) ) ;
#17873 = ADVANCED_FACE ( 'NONE', ( #25707 ), #1220, .F. ) ;
#17874 = ADVANCED_FACE ( 'NONE', ( #1412 ), #26118, .F. ) ;
#17875 = CARTESIAN_POINT ( 'NONE',  ( 17.87230948671713193, -3.179145971208983568, -2.954519006336920217 ) ) ;
#17876 = AXIS2_PLACEMENT_3D ( 'NONE', #12573, #21449, #34025 ) ;
#17877 = CARTESIAN_POINT ( 'NONE',  ( 1.751251297819361730, -26.64985754041175525, 6.700000000000000178 ) ) ;
#17878 = VERTEX_POINT ( 'NONE', #38853 ) ;
#17879 = ADVANCED_FACE ( 'NONE', ( #35198 ), #38445, .F. ) ;
#17880 = CARTESIAN_POINT ( 'NONE',  ( 8.290806648384990041, 0.000000000000000000, 6.000000000000000000 ) ) ;
#17881 = VERTEX_POINT ( 'NONE', #17220 ) ;
#17882 = EDGE_LOOP ( 'NONE', ( #21980, #16741, #6132, #12234 ) ) ;
#17883 = LINE ( 'NONE', #152, #22700 ) ;
#17884 = CARTESIAN_POINT ( 'NONE',  ( 81.02339296473685692, 62.20010510126473235, -2.956864960647744844 ) ) ;
#17885 =( BOUNDED_CURVE ( )  B_SPLINE_CURVE ( 3, ( #33022, #22954, #10969, #7288 ),
 .UNSPECIFIED., .F., .T. ) 
 B_SPLINE_CURVE_WITH_KNOTS ( ( 4, 4 ),
 ( 4.708531083176467291, 4.895802057644188743 ),
 .UNSPECIFIED. ) 
 CURVE ( )  GEOMETRIC_REPRESENTATION_ITEM ( )  RATIONAL_B_SPLINE_CURVE ( ( 1.000000000000000000, 0.9970795998553221295, 0.9970795998553221295, 1.000000000000000000 ) ) 
 REPRESENTATION_ITEM ( '' )  );
#17886 = LINE ( 'NONE', #24280, #20774 ) ;
#17887 = EDGE_LOOP ( 'NONE', ( #16879, #13492, #25966, #15649 ) ) ;
#17889 = CARTESIAN_POINT ( 'NONE',  ( 4.284140121002783630, -27.35989946098248637, 7.721096864323904185 ) ) ;
#17888 = CARTESIAN_POINT ( 'NONE',  ( 4.814300635272573459, -27.97194261433657658, 7.009310105710484073 ) ) ;
#17890 = ORIENTED_EDGE ( 'NONE', *, *, #10159, .T. ) ;
#17891 = CARTESIAN_POINT ( 'NONE',  ( 22.56545177997091756, 3.994598255509013374, 3.706573800970350607 ) ) ;
#17892 = CARTESIAN_POINT ( 'NONE',  ( 82.10888692569052694, 64.42619117010471541, -2.360008641315554545 ) ) ;
#17893 = CYLINDRICAL_SURFACE ( 'NONE', #945, 2.681419499219045655 ) ;
#17894 = VERTEX_POINT ( 'NONE', #10646 ) ;
#17895 = EDGE_CURVE ( 'NONE', #4105, #38156, #31791, .T. ) ;
#17897 = CARTESIAN_POINT ( 'NONE',  ( 1.074608721727911664, -26.22801491291194864, 7.693875151218754205 ) ) ;
#17896 = CARTESIAN_POINT ( 'NONE',  ( 0.08686669100723981574, -26.57716756243731382, 7.774064877406531515 ) ) ;
#17898 = CARTESIAN_POINT ( 'NONE',  ( -80.92837670882107659, 2.429809908903242555, 12.50000000000000000 ) ) ;
#17899 = CARTESIAN_POINT ( 'NONE',  ( 75.87451422959399849, 60.69085731309660758, 3.756674307851894490 ) ) ;
#17900 = VERTEX_POINT ( 'NONE', #38651 ) ;
#17901 = CARTESIAN_POINT ( 'NONE',  ( 22.42500037023215498, 3.508167257036367559, -4.192016948695993506 ) ) ;
#17902 = CARTESIAN_POINT ( 'NONE',  ( 4.421194222029321885, -27.53100279559231112, 7.013842709614101167 ) ) ;
#17903 = CARTESIAN_POINT ( 'NONE',  ( -73.07498068578524908, 39.58105274722134226, -9.800414904976365804 ) ) ;
#17904 = ORIENTED_EDGE ( 'NONE', *, *, #9059, .T. ) ;
#17905 = LINE ( 'NONE', #14609, #8310 ) ;
#17906 = CARTESIAN_POINT ( 'NONE',  ( 81.89445579901088479, 62.31310441928819444, 2.222430037835991801 ) ) ;
#17907 = CARTESIAN_POINT ( 'NONE',  ( 85.39749695915146788, 2.435202802470831873, -2.633776547657810774 ) ) ;
#17908 = CARTESIAN_POINT ( 'NONE',  ( 5.130566331936590174, -30.26557237595616812, 6.864665094830451508 ) ) ;
#17909 = DIRECTION ( 'NONE',  ( 0.8660254037844449249, -0.4999999999999888423, -0.000000000000000000 ) ) ;
#17910 = CIRCLE ( 'NONE', #19260, 0.1000000000000028644 ) ;
#17911 = CARTESIAN_POINT ( 'NONE',  ( 2.760057193591220148, -32.90566183273490708, 6.875780273367530171 ) ) ;
#17912 = EDGE_CURVE ( 'NONE', #21175, #25652, #13944, .T. ) ;
#17913 = LINE ( 'NONE', #37061, #25750 ) ;
#17914 = CARTESIAN_POINT ( 'NONE',  ( 0.09894228122565373873, -26.45779829264445482, 7.013842709614101167 ) ) ;
#17915 = CARTESIAN_POINT ( 'NONE',  ( 22.92222552203326913, 2.655818790012281827, -3.783965687468869188 ) ) ;
#17916 = CARTESIAN_POINT ( 'NONE',  ( 5.100363281305461349, -29.55642757665872722, 7.635761828346577573 ) ) ;
#17917 = LINE ( 'NONE', #2307, #31217 ) ;
#17918 = CARTESIAN_POINT ( 'NONE',  ( -17.27251170661583402, 0.7293679304675921848, 6.000000000000000000 ) ) ;
#17919 = ADVANCED_FACE ( 'NONE', ( #3914 ), #29792, .F. ) ;
#17920 = DIRECTION ( 'NONE',  ( -0.000000000000000000, -1.000000000000000000, -0.000000000000000000 ) ) ;
#17921 = CARTESIAN_POINT ( 'NONE',  ( 3.495976636161775009, -32.58216173033495977, 7.255881584735162981 ) ) ;
#17922 = EDGE_CURVE ( 'NONE', #13813, #5244, #10249, .T. ) ;
#17923 = VERTEX_POINT ( 'NONE', #35399 ) ;
#17924 = CARTESIAN_POINT ( 'NONE',  ( 25.66379520857860896, 2.554708175624311295, 3.769253407694455937 ) ) ;
#17925 = CARTESIAN_POINT ( 'NONE',  ( -71.54962422038506986, 0.008394241410477492477, 3.968280824155049125 ) ) ;
#17926 = CARTESIAN_POINT ( 'NONE',  ( 67.02763120020985355, 57.94366503926806899, -3.998791315154376136 ) ) ;
#17927 = EDGE_CURVE ( 'NONE', #38693, #28971, #2666, .T. ) ;
#17928 = CARTESIAN_POINT ( 'NONE',  ( -58.99872204295123623, 28.48507918597136523, -6.834244957304557389 ) ) ;
#17929 = ORIENTED_EDGE ( 'NONE', *, *, #36087, .F. ) ;
#17930 = CARTESIAN_POINT ( 'NONE',  ( 4.722721840544713778, -27.80484921947353527, 7.750000000000000888 ) ) ;
#17931 = CARTESIAN_POINT ( 'NONE',  ( 86.36844116871179722, -0.4091080490822271987, -5.842633456154400662 ) ) ;
#17932 = DIRECTION ( 'NONE',  ( -0.000000000000000000, -1.000000000000000000, -0.000000000000000000 ) ) ;
#17933 = CARTESIAN_POINT ( 'NONE',  ( 1.037538140294150812, -32.90470487196093785, 6.874555630061442102 ) ) ;
#17934 = CARTESIAN_POINT ( 'NONE',  ( -38.34874870218063592, -26.64985754041175525, 6.700000000000000178 ) ) ;
#17935 = LINE ( 'NONE', #21661, #33949 ) ;
#17936 = AXIS2_PLACEMENT_3D ( 'NONE', #36004, #23819, #13767 ) ;
#17937 = DIRECTION ( 'NONE',  ( 8.398074759113475787E-17, -1.000000000000000000, 0.000000000000000000 ) ) ;
#17938 = ORIENTED_EDGE ( 'NONE', *, *, #11586, .T. ) ;
#17939 = CARTESIAN_POINT ( 'NONE',  ( 24.37389473963558828, 3.149138647862574025, 3.338671700856682634 ) ) ;
#17940 = CARTESIAN_POINT ( 'NONE',  ( 82.35470118046110599, 62.54510421749741056, -1.000000000000000000 ) ) ;
#17941 = CARTESIAN_POINT ( 'NONE',  ( 80.38808068765764858, 63.91986139366765940, 3.633989118465185797 ) ) ;
#17942 = CARTESIAN_POINT ( 'NONE',  ( 22.35187765366807255, 4.908147690922692874, -3.032796251420805334 ) ) ;
#17943 = EDGE_LOOP ( 'NONE', ( #37953, #28553, #26013, #3052 ) ) ;
#17944 = CARTESIAN_POINT ( 'NONE',  ( 78.66234234182429930, 62.19549841187283334, -3.710351296122902820 ) ) ;
#17946 = CARTESIAN_POINT ( 'NONE',  ( 14.75311975069267767, -5.145954708339309569, -2.499999999999999556 ) ) ;
#17945 = CARTESIAN_POINT ( 'NONE',  ( 21.73414723497777601, 0.2237007742282378919, 9.085389038113099502 ) ) ;
#17947 = CARTESIAN_POINT ( 'NONE',  ( 81.45253739226865264, 61.71286443377192654, -1.983726836935522542 ) ) ;
#17948 = CARTESIAN_POINT ( 'NONE',  ( 78.81457101317378999, 64.04164361847183784, 3.641957811749153784 ) ) ;
#17949 = VECTOR ( 'NONE', #24990, 1000.000000000000000 ) ;
#17950 = CARTESIAN_POINT ( 'NONE',  ( -0.8394110418630301718, -27.30951073800569162, 7.774064877406532403 ) ) ;
#17951 = ORIENTED_EDGE ( 'NONE', *, *, #22649, .F. ) ;
#17952 = CARTESIAN_POINT ( 'NONE',  ( 82.50731566719309740, 63.18365725368109764, 1.509105202934762024 ) ) ;
#17955 = VERTEX_POINT ( 'NONE', #10447 ) ;
#17954 = CARTESIAN_POINT ( 'NONE',  ( 14.69558838330753936, 10.99631180437154399, 5.999999999999998224 ) ) ;
#17953 = FACE_OUTER_BOUND ( 'NONE', #3307, .T. ) ;
#17956 = CARTESIAN_POINT ( 'NONE',  ( 27.87470673840761037, 2.608020033772324275, -0.5247038454205935620 ) ) ;
#17957 = CARTESIAN_POINT ( 'NONE',  ( -24.87867591359218977, -26.64985754041175525, 6.700000000000000178 ) ) ;
#17958 = CARTESIAN_POINT ( 'NONE',  ( 5.651251297819362307, -26.64985754041175525, 6.800000000000000711 ) ) ;
#17959 = CARTESIAN_POINT ( 'NONE',  ( -1.583399485992929234, -33.56764205940365997, 7.695279973900954751 ) ) ;
#17960 = CIRCLE ( 'NONE', #5485, 1.000000000000000666 ) ;
#17961 = DIRECTION ( 'NONE',  ( 1.000000000000000000, 1.165409145176969993E-16, 0.000000000000000000 ) ) ;
#17962 = EDGE_CURVE ( 'NONE', #33357, #9291, #13620, .T. ) ;
#17963 = DIRECTION ( 'NONE',  ( -0.2744342186262705430, -0.9616058754224562355, 0.000000000000000000 ) ) ;
#17964 = CARTESIAN_POINT ( 'NONE',  ( 5.172631060824327776, -29.12999534392161038, 6.895394898881670009 ) ) ;
#17965 = CARTESIAN_POINT ( 'NONE',  ( -0.1940712780794633940, -32.51289061680132875, 7.013842709614101167 ) ) ;
#17966 = CARTESIAN_POINT ( 'NONE',  ( 35.72922540656550439, -1.306583851340389568, -5.539915139646041098 ) ) ;
#17967 = CARTESIAN_POINT ( 'NONE',  ( 3.371584782127380553, -26.60899745902780111, 7.670860738520336675 ) ) ;
#17968 = CARTESIAN_POINT ( 'NONE',  ( 1.145397458645855071, -32.92432777161535284, 7.692469944509197077 ) ) ;
#17969 = CARTESIAN_POINT ( 'NONE',  ( 5.046365345827218185, -28.96623356337001809, 7.635761828346577573 ) ) ;
#17970 = DIRECTION ( 'NONE',  ( -0.000000000000000000, 0.000000000000000000, 1.000000000000000000 ) ) ;
#17971 = CARTESIAN_POINT ( 'NONE',  ( 2.669612181258177674, -32.82885884042005387, 6.920489980334475710 ) ) ;
#17972 = CARTESIAN_POINT ( 'NONE',  ( 5.099918824123694350, -29.62653767273290484, 6.887041543973313473 ) ) ;
#17973 = CARTESIAN_POINT ( 'NONE',  ( 5.051054751933684805, -30.14703185982037681, 7.635761828346577573 ) ) ;
#17974 = B_SPLINE_CURVE_WITH_KNOTS ( 'NONE', 3,
 ( #33171, #39528, #27178, #29866 ),
 .UNSPECIFIED., .F., .F.,
 ( 4, 4 ),
 ( -0.001266773094470111972, 0.007521117280178637142 ),
 .UNSPECIFIED. ) ;
#17975 = CARTESIAN_POINT ( 'NONE',  ( 14.74770783127116225, -5.101789873208831594, -2.500101740053638721 ) ) ;
#17976 = CARTESIAN_POINT ( 'NONE',  ( 24.65075606035322409, 2.451163913605999500, -4.035534303674817913 ) ) ;
#17977 = CARTESIAN_POINT ( 'NONE',  ( 2.204354934003065480, -33.03347235908793067, 6.863784140767622333 ) ) ;
#17978 = ORIENTED_EDGE ( 'NONE', *, *, #10083, .F. ) ;
#17979 = CARTESIAN_POINT ( 'NONE',  ( 66.57766344320866381, 57.81227849924184881, 3.999802976169922974 ) ) ;
#17980 = CARTESIAN_POINT ( 'NONE',  ( 68.95366548541680629, 59.44408286695458798, -3.907754234428187257 ) ) ;
#17981 = EDGE_CURVE ( 'NONE', #19029, #5035, #35732, .T. ) ;
#17982 = EDGE_CURVE ( 'NONE', #4809, #4541, #33262, .T. ) ;
#17983 = AXIS2_PLACEMENT_3D ( 'NONE', #16322, #37340, #19223 ) ;
#17984 = ORIENTED_EDGE ( 'NONE', *, *, #32563, .F. ) ;
#17985 = LINE ( 'NONE', #18190, #1578 ) ;
#17986 = EDGE_CURVE ( 'NONE', #218, #40623, #36940, .T. ) ;
#17987 = CARTESIAN_POINT ( 'NONE',  ( 0.1594620532245137889, -26.53915374751568734, 6.887945620086119547 ) ) ;
#17988 = CARTESIAN_POINT ( 'NONE',  ( -20.44874870218064444, -26.64985754041175525, 6.800000000000000711 ) ) ;
#17990 = CARTESIAN_POINT ( 'NONE',  ( 1.233316054836066877, -26.20214888389141095, 6.863904403958575706 ) ) ;
#17989 = DIRECTION ( 'NONE',  ( -0.000000000000000000, 0.000000000000000000, 1.000000000000000000 ) ) ;
#17991 = PRODUCT_CONTEXT ( 'NONE', #12393, 'mechanical' ) ;
#17992 = CARTESIAN_POINT ( 'NONE',  ( 6.089801904741589667, -27.84269339272794852, 7.754798119455333705 ) ) ;
#17993 = ORIENTED_EDGE ( 'NONE', *, *, #4554, .T. ) ;
#17994 = DIRECTION ( 'NONE',  ( -1.000000000000000000, 0.000000000000000000, 0.000000000000000000 ) ) ;
#17995 =( NAMED_UNIT ( * ) SI_UNIT ( $, .STERADIAN. ) SOLID_ANGLE_UNIT ( ) );
#17996 = AXIS2_PLACEMENT_3D ( 'NONE', #29894, #30109, #32803 ) ;
#17997 = ORIENTED_EDGE ( 'NONE', *, *, #6257, .F. ) ;
#17998 = CARTESIAN_POINT ( 'NONE',  ( 78.47662320409183678, 65.68507013823818852, -2.197205184446134218 ) ) ;
#17999 = EDGE_CURVE ( 'NONE', #37105, #33136, #40226, .T. ) ;
#18000 = CARTESIAN_POINT ( 'NONE',  ( 15.45142779812353595, 8.160990771695352919, -3.484307217422537128 ) ) ;
#18001 = CARTESIAN_POINT ( 'NONE',  ( 79.40575531231831974, 66.18134094231184861, -1.781440269582275970 ) ) ;
#18002 = CARTESIAN_POINT ( 'NONE',  ( 79.22323586724850486, 64.66701280635210480, 3.467090974304451123 ) ) ;
#18003 = PLANE ( 'NONE',  #23833 ) ;
#18004 = CARTESIAN_POINT ( 'NONE',  ( 18.51121960923875420, 13.22484341366685179, 2.500000000000000000 ) ) ;
#18005 = CARTESIAN_POINT ( 'NONE',  ( 21.85643539959778536, -8.233350057040109249, -11.92691213149646678 ) ) ;
#18006 = VERTEX_POINT ( 'NONE', #31184 ) ;
#18007 = CARTESIAN_POINT ( 'NONE',  ( -80.33892546431293624, 10.54035603179613645, 3.406678657042826686 ) ) ;
#18008 = CARTESIAN_POINT ( 'NONE',  ( 2.140846989427893643, -33.04210496623404225, 7.013842709614101167 ) ) ;
#18009 = FACE_OUTER_BOUND ( 'NONE', #1615, .T. ) ;
#18010 = AXIS2_PLACEMENT_3D ( 'NONE', #37077, #2529, #1914 ) ;
#18011 = VECTOR ( 'NONE', #10380, 1000.000000000000000 ) ;
#18012 = CARTESIAN_POINT ( 'NONE',  ( -74.59285101708645982, 9.286242826285279861, -9.309355451202566911 ) ) ;
#18013 = CARTESIAN_POINT ( 'NONE',  ( -20.97867591359219475, -24.55319635012989110, 6.700000000000000178 ) ) ;
#18014 = CARTESIAN_POINT ( 'NONE',  ( -10.24874870218063450, -26.64985754041175525, 6.800000000000000711 ) ) ;
#18015 = CARTESIAN_POINT ( 'NONE',  ( -1.744286257805016227, -30.18979420120317769, 7.756742906098588186 ) ) ;
#18016 = CARTESIAN_POINT ( 'NONE',  ( 14.77394331808939754, 12.30091350227530178, 2.512229182593968879 ) ) ;
#18017 = LINE ( 'NONE', #36559, #24725 ) ;
#18018 = CARTESIAN_POINT ( 'NONE',  ( 0.6222294206236387293, -26.24011383383516360, 6.867199677474202346 ) ) ;
#18019 = CARTESIAN_POINT ( 'NONE',  ( 5.063156877882684093, -29.06813385812045425, 7.778050822775631978 ) ) ;
#18020 = VECTOR ( 'NONE', #331, 1000.000000000000000 ) ;
#18021 = CARTESIAN_POINT ( 'NONE',  ( -70.66492681425577871, 0.2167243893765767038, 4.000000000152813762 ) ) ;
#18022 = PLANE ( 'NONE',  #20626 ) ;
#18023 = CARTESIAN_POINT ( 'NONE',  ( 24.72039900981634020, 2.638341910851478289, -3.924397643197742980 ) ) ;
#18024 = CIRCLE ( 'NONE', #308, 0.1000000000000028644 ) ;
#18025 = ORIENTED_EDGE ( 'NONE', *, *, #5584, .F. ) ;
#18026 = CARTESIAN_POINT ( 'NONE',  ( 67.73962338513339887, 58.26590004628993569, 3.997461085607390885 ) ) ;
#18027 = CARTESIAN_POINT ( 'NONE',  ( 36.14556864329624375, -3.195503675045440417, 5.847788189304162998 ) ) ;
#18028 = ADVANCED_FACE ( 'NONE', ( #3005 ), #28077, .F. ) ;
#18029 = CARTESIAN_POINT ( 'NONE',  ( 88.07792789432249947, -1.225918755007668226, 4.438991276806098618 ) ) ;
#18030 = EDGE_CURVE ( 'NONE', #1346, #19329, #24032, .T. ) ;
#18031 = DIRECTION ( 'NONE',  ( 0.000000000000000000, 0.000000000000000000, 1.000000000000000000 ) ) ;
#18032 = EDGE_LOOP ( 'NONE', ( #19867, #8379, #37046, #39277 ) ) ;
#18033 = CARTESIAN_POINT ( 'NONE',  ( -30.97867591359219119, -24.55319635012989110, 6.700000000000000178 ) ) ;
#18034 = FACE_OUTER_BOUND ( 'NONE', #13963, .T. ) ;
#18035 = CARTESIAN_POINT ( 'NONE',  ( -0.6886162980804276801, -32.12779031683759712, 6.921725064902948255 ) ) ;
#18036 = ORIENTED_EDGE ( 'NONE', *, *, #38628, .F. ) ;
#18037 = DIRECTION ( 'NONE',  ( 0.000000000000000000, 0.000000000000000000, 1.000000000000000000 ) ) ;
#18038 = ORIENTED_EDGE ( 'NONE', *, *, #25014, .F. ) ;
#18039 = CARTESIAN_POINT ( 'NONE',  ( 79.43051736299561583, 64.82585401503283151, -3.419027627190938556 ) ) ;
#18040 = CARTESIAN_POINT ( 'NONE',  ( -1.699609906766908818, -29.56993018339339940, 7.620413589471895399 ) ) ;
#18041 = CARTESIAN_POINT ( 'NONE',  ( 79.20065834867811816, 65.31285345095548678, 3.018898740118463486 ) ) ;
#18042 = CARTESIAN_POINT ( 'NONE',  ( 23.11977184038386568, 0.3886633077729012564, 5.889684842570323653 ) ) ;
#18044 = VERTEX_POINT ( 'NONE', #38148 ) ;
#18043 = CARTESIAN_POINT ( 'NONE',  ( -63.99293516169446150, 35.89893413629672381, 7.506047544094577084 ) ) ;
#18045 = CIRCLE ( 'NONE', #40415, 0.1000000000000028644 ) ;
#18046 = CARTESIAN_POINT ( 'NONE',  ( 73.75428705932469597, 62.33035115498116596, -3.485789274173696661 ) ) ;
#18047 = CARTESIAN_POINT ( 'NONE',  ( 3.336167888981159013, -32.55058882503006146, 6.874555630061441214 ) ) ;
#18049 = CARTESIAN_POINT ( 'NONE',  ( 24.31117675895931640, -6.336924832510081096, 2.705487332722515070 ) ) ;
#18048 = CARTESIAN_POINT ( 'NONE',  ( -70.92837670882107659, -48.61702805680358352, 10.00000000000000888 ) ) ;
#18050 = DIRECTION ( 'NONE',  ( 1.000000000000000000, 0.000000000000000000, 0.000000000000000000 ) ) ;
#18051 = CARTESIAN_POINT ( 'NONE',  ( -71.92837670882107659, 28.72470171467712063, 5.916079783099620570 ) ) ;
#18052 = CARTESIAN_POINT ( 'NONE',  ( 81.62248346935344046, 65.70993096190733240, 1.000000000000000000 ) ) ;
#18053 = EDGE_CURVE ( 'NONE', #4540, #20545, #707, .T. ) ;
#18054 = CARTESIAN_POINT ( 'NONE',  ( 22.40957643201438998, 4.835774058222286342, -3.128480170401936711 ) ) ;
#18055 = ORIENTED_EDGE ( 'NONE', *, *, #30608, .F. ) ;
#18056 = CARTESIAN_POINT ( 'NONE',  ( 25.43482567069144906, -3.911874351919522041, 4.043259094187231284 ) ) ;
#18057 = CARTESIAN_POINT ( 'NONE',  ( 3.074471320773512595, -32.79634853659045746, 7.139344958878411695 ) ) ;
#18058 = CARTESIAN_POINT ( 'NONE',  ( 1.084888741049048200, -33.00974195381812848, 7.773839561854631874 ) ) ;
#18059 = CARTESIAN_POINT ( 'NONE',  ( 81.41366110773391540, 61.69541933536105915, 2.011547652603478564 ) ) ;
#18060 = CARTESIAN_POINT ( 'NONE',  ( 87.47045099524558509, -1.608924759093422807, 4.367130927193085377 ) ) ;
#18061 = LINE ( 'NONE', #24661, #11476 ) ;
#18062 = EDGE_LOOP ( 'NONE', ( #15642, #10589, #15874, #10204, #4898 ) ) ;
#18063 = CARTESIAN_POINT ( 'NONE',  ( 24.75839165839662925, 3.019244830385916956, -3.350409272483306111 ) ) ;
#18064 = B_SPLINE_CURVE_WITH_KNOTS ( 'NONE', 3,
 ( #24768, #9112, #24977, #12609, #21687, #34265, #25176, #28052, #6239, #40601, #9308, #31362 ),
 .UNSPECIFIED., .F., .F.,
 ( 4, 2, 2, 2, 2, 4 ),
 ( 1.734723475976807094E-18, 0.0007700302096414094822, 0.001155045314462114494, 0.001540060419282819181, 0.002310090628924224218, 0.003080120838565629255 ),
 .UNSPECIFIED. ) ;
#18065 = EDGE_CURVE ( 'NONE', #23718, #40022, #25445, .T. ) ;
#18066 = VECTOR ( 'NONE', #31067, 1000.000000000000114 ) ;
#18067 = VECTOR ( 'NONE', #33739, 1000.000000000000000 ) ;
#18068 = LINE ( 'NONE', #31471, #17712 ) ;
#18069 = CARTESIAN_POINT ( 'NONE',  ( 14.71635582635168049, -5.056528932363767659, -2.496255067347275869 ) ) ;
#18070 = CARTESIAN_POINT ( 'NONE',  ( 34.33124084974205914, -1.490659953222954082, -5.564618457436417920 ) ) ;
#18071 = CARTESIAN_POINT ( 'NONE',  ( 2.455443087130759761, -25.36557027936252950, 7.635761828346577573 ) ) ;
#18072 = AXIS2_PLACEMENT_3D ( 'NONE', #14279, #26848, #11180 ) ;
#18073 = CARTESIAN_POINT ( 'NONE',  ( 1.894216096139698768, -26.17545946167590998, 6.903372536218456368 ) ) ;
#18074 = ORIENTED_EDGE ( 'NONE', *, *, #31418, .F. ) ;
#18075 = CARTESIAN_POINT ( 'NONE',  ( 33.46294586609511867, -3.082559428606642893, 5.429100025444929756 ) ) ;
#18076 = CARTESIAN_POINT ( 'NONE',  ( 0.000000000000000000, 10.37661300689600097, 6.000000000000000000 ) ) ;
#18077 = EDGE_CURVE ( 'NONE', #18814, #27830, #3210, .T. ) ;
#18078 = ORIENTED_EDGE ( 'NONE', *, *, #31863, .T. ) ;
#18079 = ORIENTED_EDGE ( 'NONE', *, *, #26217, .F. ) ;
#18081 = CARTESIAN_POINT ( 'NONE',  ( 36.88836814539537556, -3.352193696304970771, 5.910347166897455651 ) ) ;
#18080 = CARTESIAN_POINT ( 'NONE',  ( 81.14908696703564317, 61.29647948322620010, -1.137963815189213079 ) ) ;
#18082 = CARTESIAN_POINT ( 'NONE',  ( 26.14529050879839289, -2.760665599016054905, 4.287002928775177857 ) ) ;
#18083 = CARTESIAN_POINT ( 'NONE',  ( 3.467144142116896255, -32.59128420613762245, 7.643192810543821381 ) ) ;
#18084 = CARTESIAN_POINT ( 'NONE',  ( 4.769070051701195467, -31.05032170149767978, 7.505001789837629111 ) ) ;
#18085 = ORIENTED_EDGE ( 'NONE', *, *, #25757, .T. ) ;
#18086 = ORIENTED_EDGE ( 'NONE', *, *, #20360, .F. ) ;
#18087 = VERTEX_POINT ( 'NONE', #37947 ) ;
#18088 = DIRECTION ( 'NONE',  ( -0.9999026450364576490, -0.01395351027862084224, 0.000000000000000000 ) ) ;
#18089 = CARTESIAN_POINT ( 'NONE',  ( 80.11713744326790732, 64.15277314745162585, -3.661914029440275886 ) ) ;
#18090 = CARTESIAN_POINT ( 'NONE',  ( -59.07422214908517333, 27.36241337473656543, -4.461357708502241337 ) ) ;
#18092 = CARTESIAN_POINT ( 'NONE',  ( 14.74962925723615825, 13.05063958598015184, 2.500338280337064845 ) ) ;
#18091 = CARTESIAN_POINT ( 'NONE',  ( 24.30393741781215411, 2.735322053734381864, 3.908150415328090599 ) ) ;
#18093 = ORIENTED_EDGE ( 'NONE', *, *, #33744, .F. ) ;
#18094 = CARTESIAN_POINT ( 'NONE',  ( 82.22574661183148237, 63.03983423078044268, -2.217414436011609702 ) ) ;
#18095 = VECTOR ( 'NONE', #16416, 1000.000000000000000 ) ;
#18096 = AXIS2_PLACEMENT_3D ( 'NONE', #31649, #19282, #25463 ) ;
#18097 = CARTESIAN_POINT ( 'NONE',  ( 14.77500326541903952, -5.175625724643098557, -2.499997102511863911 ) ) ;
#18098 = ORIENTED_EDGE ( 'NONE', *, *, #36948, .T. ) ;
#18100 = CARTESIAN_POINT ( 'NONE',  ( 25.54817441638135023, -2.736180225144035028, -4.193808521246229049 ) ) ;
#18099 = DIRECTION ( 'NONE',  ( 0.000000000000000000, 0.000000000000000000, 1.000000000000000000 ) ) ;
#18101 = CARTESIAN_POINT ( 'NONE',  ( -1.796599816117110171, -29.42480412128576717, 6.875780273367531059 ) ) ;
#18102 = CARTESIAN_POINT ( 'NONE',  ( 74.35309583984513893, 59.45637312398173435, 3.556895493431092348 ) ) ;
#18103 = CARTESIAN_POINT ( 'NONE',  ( 21.85572174241494636, 3.841057816001869796, -4.459226767376585521 ) ) ;
#18104 = CARTESIAN_POINT ( 'NONE',  ( 4.812521983982041895, -27.96848237138598137, 7.013842709614101167 ) ) ;
#18105 = CARTESIAN_POINT ( 'NONE',  ( 21.85643539959775694, 2.564233178479530917, 15.28924334870111146 ) ) ;
#18106 = PLANE ( 'NONE',  #14414 ) ;
#18107 = ORIENTED_EDGE ( 'NONE', *, *, #23161, .T. ) ;
#18108 = CYLINDRICAL_SURFACE ( 'NONE', #24101, 0.09010775117053039518 ) ;
#18109 = CARTESIAN_POINT ( 'NONE',  ( 81.65405438441128183, 61.80769279848060194, 1.809109834152203833 ) ) ;
#18110 = CARTESIAN_POINT ( 'NONE',  ( 87.10205511408864254, 0.5205621796347451591, 5.292648712017772539 ) ) ;
#18111 = DIRECTION ( 'NONE',  ( -3.491481338843133750E-15, 1.000000000000000000, -0.000000000000000000 ) ) ;
#18112 = EDGE_CURVE ( 'NONE', #39610, #30637, #22102, .T. ) ;
#18113 = FACE_OUTER_BOUND ( 'NONE', #21728, .T. ) ;
#18114 = EDGE_CURVE ( 'NONE', #26363, #2075, #27333, .T. ) ;
#18115 = CARTESIAN_POINT ( 'NONE',  ( 2.715450815169567100, -32.91950506007766819, 6.941203072598474577 ) ) ;
#18116 = DIRECTION ( 'NONE',  ( 0.4582725098355734938, -0.8888117386314180468, 0.000000000000000000 ) ) ;
#18117 = CARTESIAN_POINT ( 'NONE',  ( 28.67087680535204797, -4.024283280459782119, 4.110896467804376009 ) ) ;
#18118 = CARTESIAN_POINT ( 'NONE',  ( 36.19525661438556341, -2.229558765483345528, -5.855543198900774016 ) ) ;
#18119 = CARTESIAN_POINT ( 'NONE',  ( 0.5160167997142889318, -32.86344804452599533, 7.635761828346576685 ) ) ;
#18120 = CARTESIAN_POINT ( 'NONE',  ( 4.631402061531082026, -31.48282785863527167, 6.971170733404096431 ) ) ;
#18121 = DIRECTION ( 'NONE',  ( 0.000000000000000000, 0.000000000000000000, 1.000000000000000000 ) ) ;
#18122 = CARTESIAN_POINT ( 'NONE',  ( 1.577180237285443098, -33.06768434091362963, 7.753200566781576875 ) ) ;
#18123 = VECTOR ( 'NONE', #31214, 1000.000000000000000 ) ;
#18124 = CARTESIAN_POINT ( 'NONE',  ( -70.01240559167840161, -45.92514165124313763, 5.930240575752830701 ) ) ;
#18125 = VECTOR ( 'NONE', #32305, 1000.000000000000000 ) ;
#18126 = EDGE_CURVE ( 'NONE', #38094, #38896, #30849, .T. ) ;
#18127 = EDGE_LOOP ( 'NONE', ( #5249, #23639, #1063, #11687 ) ) ;
#18128 = CARTESIAN_POINT ( 'NONE',  ( 36.98735379331689899, -2.280088017890153473, 5.924094764607088948 ) ) ;
#18129 =( BOUNDED_SURFACE ( )  B_SPLINE_SURFACE ( 3, 2, ( 
 ( #10476, #15700, #31563 ),
 ( #78, #37707, #12810 ),
 ( #13573, #22097, #3186 ),
 ( #6036, #28252, #19949 ) ),
 .UNSPECIFIED., .F., .F., .T. ) 
 B_SPLINE_SURFACE_WITH_KNOTS ( ( 4, 4 ),
 ( 3, 3 ),
 ( 0.1160236983739658390, 0.1317050650460910299 ),
 ( 0.1027166521410490529, 1.000000000000000000 ),
 .UNSPECIFIED. ) 
 GEOMETRIC_REPRESENTATION_ITEM ( )  RATIONAL_B_SPLINE_SURFACE ( (
 ( 0.9864974513313498061, 0.9342728350895400657, 1.000000000000000000),
 ( 0.9864974513313498061, 0.9342728350895400657, 1.000000000000000000),
 ( 0.9864974513313498061, 0.9342728350895399547, 1.000000000000000000),
 ( 0.9864974513313498061, 0.9342728350895399547, 1.000000000000000000) ) ) 
 REPRESENTATION_ITEM ( '' )  SURFACE ( )  );
#18130 = CARTESIAN_POINT ( 'NONE',  ( -71.70854571598145810, -0.1474806467180565794, 3.949606264851800663 ) ) ;
#18131 = CARTESIAN_POINT ( 'NONE',  ( 67.05223802139354916, 57.87567627276845883, -3.996315564296191614 ) ) ;
#18132 = DIRECTION ( 'NONE',  ( 0.000000000000000000, -0.7508067542896647018, 0.6605219282605379050 ) ) ;
#18133 = CIRCLE ( 'NONE', #32633, 79.54614097552274643 ) ;
#18134 = B_SPLINE_CURVE_WITH_KNOTS ( 'NONE', 3,
 ( #26939, #23642, #32734, #14564, #4529, #36611, #8182, #23452, #20754, #4912 ),
 .UNSPECIFIED., .F., .F.,
 ( 4, 2, 2, 2, 4 ),
 ( 0.000000000000000000, 0.2500000000000000000, 0.5000000000000000000, 0.7500000000000000000, 1.000000000000000000 ),
 .UNSPECIFIED. ) ;
#18135 = DIRECTION ( 'NONE',  ( 0.6427876096865369204, -0.7660444431189800119, 0.000000000000000000 ) ) ;
#18136 = ORIENTED_EDGE ( 'NONE', *, *, #9092, .F. ) ;
#18137 = DIRECTION ( 'NONE',  ( -0.000000000000000000, 1.000000000000000000, -0.000000000000000000 ) ) ;
#18138 = DIRECTION ( 'NONE',  ( 0.000000000000000000, 1.000000000000000000, 0.000000000000000000 ) ) ;
#18139 = CARTESIAN_POINT ( 'NONE',  ( -70.92837670882140344, -21.78291075931342391, 6.000000000000002665 ) ) ;
#18140 = CARTESIAN_POINT ( 'NONE',  ( -79.15689149791292323, 11.46365244476452361, 5.697679923243769373 ) ) ;
#18141 = ORIENTED_EDGE ( 'NONE', *, *, #3218, .F. ) ;
#18142 = CYLINDRICAL_SURFACE ( 'NONE', #26670, 6.781342077912186461 ) ;
#18143 = DIRECTION ( 'NONE',  ( 0.000000000000000000, 1.000000000000000000, 0.000000000000000000 ) ) ;
#18144 = EDGE_LOOP ( 'NONE', ( #17993, #22211, #31456, #36934, #11397 ) ) ;
#18145 = CARTESIAN_POINT ( 'NONE',  ( 21.72385588348585372, 6.222764755813646076, 3.231099798339156948 ) ) ;
#18146 = CARTESIAN_POINT ( 'NONE',  ( 82.26973386304365476, 64.90130211351629441, -1.165579324820864571 ) ) ;
#18147 = LINE ( 'NONE', #11960, #26158 ) ;
#18148 = CARTESIAN_POINT ( 'NONE',  ( 79.82480777417542583, 64.72726844050397688, 3.473545878414594945 ) ) ;
#18149 = CARTESIAN_POINT ( 'NONE',  ( -0.1401643189945547263, -32.42867603148304312, 6.876076431790004051 ) ) ;
#18150 = ORIENTED_EDGE ( 'NONE', *, *, #30697, .F. ) ;
#18151 = CARTESIAN_POINT ( 'NONE',  ( 77.74023705119593330, 64.68384637002907311, -3.042889847487472377 ) ) ;
#18152 = APPLICATION_CONTEXT ( 'automotive_design' ) ;
#18154 = DIRECTION ( 'NONE',  ( 0.000000000000000000, -1.000000000000000000, 0.000000000000000000 ) ) ;
#18153 = CARTESIAN_POINT ( 'NONE',  ( 25.40382443007142399, 0.6807430875769404643, 4.599443498573071665 ) ) ;
#18155 = CARTESIAN_POINT ( 'NONE',  ( 79.52751932687164071, 65.84655314362404965, -2.556731990913035268 ) ) ;
#18156 = CARTESIAN_POINT ( 'NONE',  ( 76.19453532209956848, 64.30418437363988460, 2.661196496273629641 ) ) ;
#18157 = ORIENTED_EDGE ( 'NONE', *, *, #32300, .T. ) ;
#18158 = CYLINDRICAL_SURFACE ( 'NONE', #6989, 0.1000000000000028644 ) ;
#18159 = CARTESIAN_POINT ( 'NONE',  ( 82.20671311902191292, 64.86843738523491254, 1.633153239554254732 ) ) ;
#18161 = CARTESIAN_POINT ( 'NONE',  ( -1.695633640289647914, -29.40533622940153791, 6.876076431790004939 ) ) ;
#18160 = CYLINDRICAL_SURFACE ( 'NONE', #33624, 1.500000000000001332 ) ;
#18162 = CARTESIAN_POINT ( 'NONE',  ( 32.63594197759655913, -2.548278591510585667, -5.894033951951210604 ) ) ;
#18163 = VECTOR ( 'NONE', #11198, 1000.000000000000114 ) ;
#18164 = ADVANCED_FACE ( 'NONE', ( #30112 ), #10947, .F. ) ;
#18165 = CARTESIAN_POINT ( 'NONE',  ( -1.774602633087123627, -29.98757303562673826, 6.951256099901590879 ) ) ;
#18166 = DIRECTION ( 'NONE',  ( 1.000000000000000000, 0.000000000000000000, 0.000000000000000000 ) ) ;
#18167 = CARTESIAN_POINT ( 'NONE',  ( 1.662469596549258855, -33.06973143922542135, 6.887161170156904433 ) ) ;
#18168 = VECTOR ( 'NONE', #10820, 1000.000000000000000 ) ;
#18169 = EDGE_CURVE ( 'NONE', #13356, #9646, #28872, .T. ) ;
#18170 = DIRECTION ( 'NONE',  ( -0.000000000000000000, -0.000000000000000000, 1.000000000000000000 ) ) ;
#18171 = LINE ( 'NONE', #36919, #6656 ) ;
#18172 = CARTESIAN_POINT ( 'NONE',  ( 0.5198276744376743030, -32.86481647987437782, 7.640616322432098428 ) ) ;
#18173 = DIRECTION ( 'NONE',  ( 0.000000000000000000, 0.000000000000000000, 1.000000000000000000 ) ) ;
#18174 = CARTESIAN_POINT ( 'NONE',  ( 36.98740879322385666, -2.280155673325318766, -5.924112469671126036 ) ) ;
#18175 = DIRECTION ( 'NONE',  ( 0.000000000000000000, 0.000000000000000000, 1.000000000000000000 ) ) ;
#18176 = AXIS2_PLACEMENT_3D ( 'NONE', #13819, #38919, #36058 ) ;
#18177 = CARTESIAN_POINT ( 'NONE',  ( -67.14418927852128149, 15.04836564048558500, 0.000000000000000000 ) ) ;
#18178 = CARTESIAN_POINT ( 'NONE',  ( -0.08065709997537935660, -26.55697965350343281, 7.697032948437506406 ) ) ;
#18179 = LINE ( 'NONE', #12419, #17949 ) ;
#18180 = CARTESIAN_POINT ( 'NONE',  ( 1.967410481810895506, -33.06655284499420588, 7.501983001166817822 ) ) ;
#18181 = CARTESIAN_POINT ( 'NONE',  ( 5.099787579797017578, -29.63441947184663405, 6.880147297696980857 ) ) ;
#18182 = LINE ( 'NONE', #30974, #37277 ) ;
#18183 = CYLINDRICAL_SURFACE ( 'NONE', #25706, 0.1000000000000028644 ) ;
#18184 = CARTESIAN_POINT ( 'NONE',  ( 22.00903206384833055, 1.428713110540158038, -6.428340196499899406 ) ) ;
#18185 = ORIENTED_EDGE ( 'NONE', *, *, #2596, .F. ) ;
#18186 = DIRECTION ( 'NONE',  ( -0.9396926207859104263, 0.3420201433256631063, -0.000000000000000000 ) ) ;
#18187 = CARTESIAN_POINT ( 'NONE',  ( 69.92361841086972163, 58.66916198470556765, -3.954846139149859052 ) ) ;
#18188 = AXIS2_PLACEMENT_3D ( 'NONE', #17934, #5601, #37083 ) ;
#18189 = EDGE_LOOP ( 'NONE', ( #37760, #17740, #18395, #19878 ) ) ;
#18190 = CARTESIAN_POINT ( 'NONE',  ( -33.07867591359219972, -26.64985754041175525, 6.800000000000000711 ) ) ;
#18191 = DIRECTION ( 'NONE',  ( 1.000000000000000000, 0.000000000000000000, -0.000000000000000000 ) ) ;
#18192 = CARTESIAN_POINT ( 'NONE',  ( 69.97231107847817100, 58.54512925548123548, 3.931953536312681852 ) ) ;
#18193 = CARTESIAN_POINT ( 'NONE',  ( 2.941320696289306813, -26.40447741350430633, 6.870716933885664623 ) ) ;
#18194 = CARTESIAN_POINT ( 'NONE',  ( 4.899719713945094313, -30.72072342401420997, 7.756377446753166538 ) ) ;
#18195 = AXIS2_PLACEMENT_3D ( 'NONE', #24151, #15295, #33752 ) ;
#18196 = ITEM_DEFINED_TRANSFORMATION ( 'NONE', 'NONE', #6433,  #30744 ) ;
#18197 = AXIS2_PLACEMENT_3D ( 'NONE', #17390, #14932, #14515 ) ;
#18198 = DIRECTION ( 'NONE',  ( 0.8831583674550981256, -0.4690749385695702767, 0.000000000000000000 ) ) ;
#18199 = EDGE_LOOP ( 'NONE', ( #18668, #21376, #27477, #3498 ) ) ;
#18200 = CARTESIAN_POINT ( 'NONE',  ( 24.08037749381573178, 3.357674872353649587, 3.169849549870835226 ) ) ;
#18201 = ORIENTED_EDGE ( 'NONE', *, *, #11406, .T. ) ;
#18202 = CARTESIAN_POINT ( 'NONE',  ( 80.79577214038279465, 61.23497056275883921, -1.884339924308600311 ) ) ;
#18203 = CARTESIAN_POINT ( 'NONE',  ( -12.99139449055068241, 13.37661300689600097, 6.000000000000000000 ) ) ;
#18204 = CARTESIAN_POINT ( 'NONE',  ( 81.76017987128373932, 63.49575590176120699, -2.919551171211517637 ) ) ;
#18205 = CARTESIAN_POINT ( 'NONE',  ( 78.63268743221328805, 65.61080103085718918, 2.414331286641656860 ) ) ;
#18206 = EDGE_CURVE ( 'NONE', #29262, #12828, #36283, .T. ) ;
#18207 = B_SPLINE_CURVE_WITH_KNOTS ( 'NONE', 3,
 ( #1394, #10229, #991, #1585, #10626, #22812, #35382, #20102, #26496, #20296 ),
 .UNSPECIFIED., .F., .F.,
 ( 4, 3, 3, 4 ),
 ( 8.673617379884035472E-19, 3.025570593003174677E-05, 6.051145698344189566E-05, 6.468151674593709615E-05 ),
 .UNSPECIFIED. ) ;
#18208 = CARTESIAN_POINT ( 'NONE',  ( -30.44874870218064089, -26.64985754041175525, 6.700000000000000178 ) ) ;
#18209 = EDGE_CURVE ( 'NONE', #2951, #35983, #29506, .T. ) ;
#18210 = CARTESIAN_POINT ( 'NONE',  ( 2.860566172189516809, -32.76586376621662566, 7.769368695748487319 ) ) ;
#18211 = CARTESIAN_POINT ( 'NONE',  ( 22.68001568621454567, -4.050230952900990111, -7.789969220879865652 ) ) ;
#18212 = ORIENTED_EDGE ( 'NONE', *, *, #38628, .T. ) ;
#18213 = FACE_OUTER_BOUND ( 'NONE', #39574, .T. ) ;
#18214 = CARTESIAN_POINT ( 'NONE',  ( -1.799428607678825287, -29.60555406228417041, 7.687540746915169976 ) ) ;
#18215 = ADVANCED_FACE ( 'NONE', ( #33205 ), #13853, .F. ) ;
#18216 = ADVANCED_FACE ( 'NONE', ( #32807 ), #4595, .F. ) ;
#18217 = CARTESIAN_POINT ( 'NONE',  ( -79.02496048640330173, 11.44822657882088457, -5.882923361518916927 ) ) ;
#18218 = DIRECTION ( 'NONE',  ( 1.000000000000000000, 0.000000000000000000, 0.000000000000000000 ) ) ;
#18219 = CARTESIAN_POINT ( 'NONE',  ( 36.44626315252003224, -1.730720475607963271, -5.729706151067262887 ) ) ;
#18220 = CARTESIAN_POINT ( 'NONE',  ( 3.739317481034212243, -32.29073431218959911, 7.013842709614101167 ) ) ;
#18221 = CARTESIAN_POINT ( 'NONE',  ( 3.977772666037320715, -27.04534534285276592, 7.754798119455333705 ) ) ;
#18222 = DIRECTION ( 'NONE',  ( -0.000000000000000000, -0.000000000000000000, 1.000000000000000000 ) ) ;
#18223 = CARTESIAN_POINT ( 'NONE',  ( 4.323735235430704371, -31.73281258077615519, 7.661510568013093270 ) ) ;
#18224 =( GEOMETRIC_REPRESENTATION_CONTEXT ( 3 ) GLOBAL_UNCERTAINTY_ASSIGNED_CONTEXT ( ( #13100 ) ) GLOBAL_UNIT_ASSIGNED_CONTEXT ( ( #32951, #16876, #32356 ) ) REPRESENTATION_CONTEXT ( 'NONE', 'WORKASPACE' ) );
#18225 = CARTESIAN_POINT ( 'NONE',  ( -8.878675913592189772, -24.55319635012989110, 6.700000000000000178 ) ) ;
#18226 = CIRCLE ( 'NONE', #20198, 0.1000000000000028644 ) ;
#18227 = AXIS2_PLACEMENT_3D ( 'NONE', #24425, #18443, #8970 ) ;
#18228 = CARTESIAN_POINT ( 'NONE',  ( 18.34140839124202316, 13.39279901796001049, -2.500000000000000000 ) ) ;
#18229 = CARTESIAN_POINT ( 'NONE',  ( 37.20163862818894529, -2.760798311994886678, -5.998390365511268918 ) ) ;
#18230 = CARTESIAN_POINT ( 'NONE',  ( 24.43632265556720284, 2.958562433187153395, -3.677099187153833437 ) ) ;
#18231 = VERTEX_POINT ( 'NONE', #2535 ) ;
#18232 = CARTESIAN_POINT ( 'NONE',  ( 67.16623404331231484, 58.01883467879599721, 3.998868826385353348 ) ) ;
#18233 = CARTESIAN_POINT ( 'NONE',  ( 33.66569764252319885, -3.445949192026814600, 5.444075323708291059 ) ) ;
#18234 = CARTESIAN_POINT ( 'NONE',  ( -1.649885511253406545, -30.14934551598626911, 7.775108481317161591 ) ) ;
#18235 = CARTESIAN_POINT ( 'NONE',  ( 2.320254111042885370, -33.01460653443150761, 7.756742906098588186 ) ) ;
#18236 = CARTESIAN_POINT ( 'NONE',  ( 84.60690941119878516, 3.085063967761199066, 1.108375916024202379 ) ) ;
#18238 = CARTESIAN_POINT ( 'NONE',  ( 4.850511272190507484, -30.84932285044435218, 6.863904403958575706 ) ) ;
#18237 = CARTESIAN_POINT ( 'NONE',  ( -0.6444488087166562185, -32.16833941288422238, 7.750000000000000888 ) ) ;
#18239 = ORIENTED_EDGE ( 'NONE', *, *, #29119, .F. ) ;
#18240 = DIRECTION ( 'NONE',  ( -1.000000000000000000, -1.165409145176970240E-16, 0.000000000000000000 ) ) ;
#18241 = DIRECTION ( 'NONE',  ( 0.000000000000000000, 0.000000000000000000, 1.000000000000000000 ) ) ;
#18242 = ORIENTED_EDGE ( 'NONE', *, *, #27188, .T. ) ;
#18243 = CARTESIAN_POINT ( 'NONE',  ( -70.08069538478937943, -21.32521480519122647, 5.952073100432614616 ) ) ;
#18244 = CIRCLE ( 'NONE', #36019, 24.28220113893567245 ) ;
#18245 = ORIENTED_EDGE ( 'NONE', *, *, #15191, .T. ) ;
#18246 = CARTESIAN_POINT ( 'NONE',  ( 81.00792578075066785, 61.24501526813143215, -1.386845825021845835 ) ) ;
#18247 = PRODUCT_DEFINITION_FORMATION_WITH_SPECIFIED_SOURCE ( 'ANY', '', #101, .NOT_KNOWN. ) ;
#18248 = CARTESIAN_POINT ( 'NONE',  ( -1.522997566795316615, -28.20618826020304226, 6.906857269533148269 ) ) ;
#18249 = CIRCLE ( 'NONE', #37337, 12.80480339192541628 ) ;
#18250 = CARTESIAN_POINT ( 'NONE',  ( 78.96452808758097319, 65.70328965153828449, 2.526545245021019515 ) ) ;
#18252 = ORIENTED_EDGE ( 'NONE', *, *, #31035, .F. ) ;
#18251 = CARTESIAN_POINT ( 'NONE',  ( -1.343674119598266214, -31.08441801232856605, 6.949473656533214694 ) ) ;
#18253 = CARTESIAN_POINT ( 'NONE',  ( 73.91602183453733232, 60.46016365699546924, -3.923277237800833817 ) ) ;
#18254 = CARTESIAN_POINT ( 'NONE',  ( -6.248748702180631831, -26.64985754041175525, 6.700000000000000178 ) ) ;
#18255 = CARTESIAN_POINT ( 'NONE',  ( 4.927406398964075507, -30.92505592019657001, 6.895394898881661128 ) ) ;
#18256 = CARTESIAN_POINT ( 'NONE',  ( -1.183594904732484521, -27.76919811496597745, 7.759451378593095860 ) ) ;
#18257 = FACE_OUTER_BOUND ( 'NONE', #22578, .T. ) ;
#18258 = CARTESIAN_POINT ( 'NONE',  ( 22.89983194485769502, 4.229321078703802250, -3.183991982619256422 ) ) ;
#18259 = ORIENTED_EDGE ( 'NONE', *, *, #19865, .F. ) ;
#18260 = CARTESIAN_POINT ( 'NONE',  ( -14.97867591359219119, -26.64985754041175525, 6.700000000000000178 ) ) ;
#18261 = ADVANCED_FACE ( 'NONE', ( #6011 ), #18142, .T. ) ;
#18262 = EDGE_CURVE ( 'NONE', #6408, #22775, #14834, .T. ) ;
#18263 = DIRECTION ( 'NONE',  ( -0.9999026450364576490, -0.01395351027862084224, 0.000000000000000000 ) ) ;
#18264 = CARTESIAN_POINT ( 'NONE',  ( 4.977259614314325731, -28.34024264869372445, 7.678495282201406091 ) ) ;
#18265 = CARTESIAN_POINT ( 'NONE',  ( 81.15996319168235118, 61.30045982539699168, 1.094381639753812863 ) ) ;
#18266 = CARTESIAN_POINT ( 'NONE',  ( 85.39947451146549895, 1.536583868559685762, 5.410284084896357371 ) ) ;
#18267 = CARTESIAN_POINT ( 'NONE',  ( 16.43736497953263864, 10.14549375742940640, 2.723904612540104075 ) ) ;
#18268 = ORIENTED_EDGE ( 'NONE', *, *, #13628, .F. ) ;
#18269 = AXIS2_PLACEMENT_3D ( 'NONE', #39419, #23774, #36351 ) ;
#18270 = PLANE ( 'NONE',  #8903 ) ;
#18271 = DIRECTION ( 'NONE',  ( 0.4690749385695654472, 0.8831583674551005680, -0.000000000000000000 ) ) ;
#18272 = AXIS2_PLACEMENT_3D ( 'NONE', #38034, #22411, #13128 ) ;
#18273 = CARTESIAN_POINT ( 'NONE',  ( 4.082517674496584981, -27.00565348427343082, 6.903112506833890549 ) ) ;
#18274 = CARTESIAN_POINT ( 'NONE',  ( 14.68480434038803928, -5.054507705527442774, -2.495523734227267365 ) ) ;
#18275 = CARTESIAN_POINT ( 'NONE',  ( -54.01549048184568846, -30.38627270959228710, 4.800000000000000711 ) ) ;
#18276 = DIRECTION ( 'NONE',  ( 1.000000000000000000, -0.000000000000000000, 0.000000000000000000 ) ) ;
#18277 = CARTESIAN_POINT ( 'NONE',  ( -0.4765361063777948658, -26.95821406652526164, 7.775108481317161591 ) ) ;
#18278 = EDGE_LOOP ( 'NONE', ( #33574, #38268, #21850, #6970 ) ) ;
#18279 = CARTESIAN_POINT ( 'NONE',  ( 37.04537786116272713, -2.801074063609814147, 5.988225179720371827 ) ) ;
#18280 = AXIS2_PLACEMENT_3D ( 'NONE', #19997, #28670, #13412 ) ;
#18281 = CARTESIAN_POINT ( 'NONE',  ( 5.121324086407808451, -26.64985754041175525, 6.700000000000000178 ) ) ;
#18282 = CARTESIAN_POINT ( 'NONE',  ( 86.13511395365257783, 1.606676384832600224, -4.558527568769633831 ) ) ;
#18283 = ORIENTED_EDGE ( 'NONE', *, *, #33249, .F. ) ;
#18284 = ORIENTED_EDGE ( 'NONE', *, *, #1888, .F. ) ;
#18286 = CARTESIAN_POINT ( 'NONE',  ( 36.13391060751988704, -1.528180889880398352, 5.641554834256164774 ) ) ;
#18285 = CARTESIAN_POINT ( 'NONE',  ( 80.10206815703587324, 64.89240018571257451, -3.380792992375218908 ) ) ;
#18287 = CARTESIAN_POINT ( 'NONE',  ( 18.12002341025573315, -2.855556945250876666, 3.034465906229363963 ) ) ;
#18288 = CARTESIAN_POINT ( 'NONE',  ( 1.230319205269136518, -26.20258206353872765, 7.754798119455333705 ) ) ;
#18289 = DIRECTION ( 'NONE',  ( 1.000000000000000000, 0.000000000000000000, 0.000000000000000000 ) ) ;
#18290 = EDGE_LOOP ( 'NONE', ( #35419, #8861 ) ) ;
#18291 = CARTESIAN_POINT ( 'NONE',  ( -1.743346351498375801, -30.19497628620385754, 7.640616322432101981 ) ) ;
#18292 = EDGE_LOOP ( 'NONE', ( #19971, #32360, #9251, #28273 ) ) ;
#18293 = ORIENTED_EDGE ( 'NONE', *, *, #30942, .T. ) ;
#18294 = CARTESIAN_POINT ( 'NONE',  ( 5.897691494960017877, -28.77484643370537754, 7.695279973900954751 ) ) ;
#18295 = CARTESIAN_POINT ( 'NONE',  ( 80.72665634072043872, 62.99526239489093626, -3.473545878414585175 ) ) ;
#18296 = AXIS2_PLACEMENT_3D ( 'NONE', #10375, #35320, #10162 ) ;
#18297 = DIRECTION ( 'NONE',  ( 1.000000000000000000, 0.000000000000000000, 0.000000000000000000 ) ) ;
#18298 = ORIENTED_EDGE ( 'NONE', *, *, #30031, .T. ) ;
#18300 = CARTESIAN_POINT ( 'NONE',  ( 32.12397651727874148, 0.2264795177381662139, 4.744950101384926455 ) ) ;
#18299 = CARTESIAN_POINT ( 'NONE',  ( 21.84524191181414210, 2.598441008144188213, 5.474373194479982274 ) ) ;
#18301 = ORIENTED_EDGE ( 'NONE', *, *, #4293, .T. ) ;
#18302 = CARTESIAN_POINT ( 'NONE',  ( 79.25820086742456283, 66.26332994521369812, -1.378120381825871599 ) ) ;
#18303 = CARTESIAN_POINT ( 'NONE',  ( -58.99872204295125755, 28.26327478256369119, 6.631997745856873294 ) ) ;
#18304 = ORIENTED_EDGE ( 'NONE', *, *, #4450, .T. ) ;
#18306 = FACE_OUTER_BOUND ( 'NONE', #28015, .T. ) ;
#18305 = CARTESIAN_POINT ( 'NONE',  ( 4.315404545797473013, -33.85565925846036350, 7.754798119455333705 ) ) ;
#18307 = CARTESIAN_POINT ( 'NONE',  ( 5.772750116865767112, -28.06626866760150563, 7.013842709614101167 ) ) ;
#18308 = CARTESIAN_POINT ( 'NONE',  ( 73.01418189060618147, 60.96508932706621664, 3.894134109168990499 ) ) ;
#18309 = CARTESIAN_POINT ( 'NONE',  ( 24.20993443650717936, 2.833309178738531386, -3.852635856680939774 ) ) ;
#18310 = CARTESIAN_POINT ( 'NONE',  ( 0.5037982502477859059, -26.38745190989316214, 7.693875151218754205 ) ) ;
#18311 = AXIS2_PLACEMENT_3D ( 'NONE', #743, #9791, #22371 ) ;
#18312 = CARTESIAN_POINT ( 'NONE',  ( 21.85643539959778181, 2.105182337828026995, -13.78739850581801996 ) ) ;
#18314 = ADVANCED_FACE ( 'NONE', ( #11749 ), #27618, .F. ) ;
#18313 = CARTESIAN_POINT ( 'NONE',  ( -58.49085810542278807, 30.53062561304904676, -5.010110517852434775 ) ) ;
#18315 = VERTEX_POINT ( 'NONE', #33620 ) ;
#18316 = CARTESIAN_POINT ( 'NONE',  ( 80.65441534633353626, 65.56043466500607053, 2.771525467261984232 ) ) ;
#18317 = CARTESIAN_POINT ( 'NONE',  ( 88.63860240521751166, -1.205360666695063365, 1.162049942889349818 ) ) ;
#18318 = DIRECTION ( 'NONE',  ( 1.000000000000000000, -0.000000000000000000, 0.000000000000000000 ) ) ;
#18319 = EDGE_CURVE ( 'NONE', #29803, #17239, #1700, .T. ) ;
#18320 = CARTESIAN_POINT ( 'NONE',  ( 2.751297001641176632, -32.90844469663947791, 6.880828092187096345 ) ) ;
#18321 = CARTESIAN_POINT ( 'NONE',  ( 15.59010151301636604, -3.705400104462427624, 2.635672183462121954 ) ) ;
#18322 = CARTESIAN_POINT ( 'NONE',  ( 21.58863023475808873, 7.202558683720228672, -2.923977588977705544 ) ) ;
#18323 = AXIS2_PLACEMENT_3D ( 'NONE', #9246, #24704, #21621 ) ;
#18324 = CARTESIAN_POINT ( 'NONE',  ( 20.42702919835091535, 3.672993461847502417, -3.394529954607447220 ) ) ;
#18325 = CARTESIAN_POINT ( 'NONE',  ( -1.583891440918162585, -30.77968007673214146, 7.635761828346579350 ) ) ;
#18326 = CARTESIAN_POINT ( 'NONE',  ( 4.641243193987799387, -31.46766203338331636, 7.009310105710484073 ) ) ;
#18327 = CARTESIAN_POINT ( 'NONE',  ( 4.899937972425366439, -30.72010120057137073, 7.635761828346577573 ) ) ;
#18328 = CARTESIAN_POINT ( 'NONE',  ( -74.03402466285142225, 19.33157623370700051, -8.800414904976364028 ) ) ;
#18329 = CARTESIAN_POINT ( 'NONE',  ( 1.513399906207050449, -32.96478432900200062, 7.013842709614101167 ) ) ;
#18330 = ORIENTED_EDGE ( 'NONE', *, *, #29195, .T. ) ;
#18331 = CARTESIAN_POINT ( 'NONE',  ( 37.17917179609320755, -2.754412960886113204, 6.000950219249740591 ) ) ;
#18332 = CARTESIAN_POINT ( 'NONE',  ( -70.92661119047551210, 0.2232129446074198609, 4.001025162589364470 ) ) ;
#18333 = ORIENTED_EDGE ( 'NONE', *, *, #7540, .T. ) ;
#18334 = EDGE_CURVE ( 'NONE', #10306, #11412, #21248, .T. ) ;
#18335 = CARTESIAN_POINT ( 'NONE',  ( 67.01778322055632486, 57.97087264248310134, -3.999241514195644775 ) ) ;
#18336 = DIRECTION ( 'NONE',  ( -0.000000000000000000, -0.000000000000000000, -1.000000000000000000 ) ) ;
#18337 = VECTOR ( 'NONE', #26447, 1000.000000000000000 ) ;
#18338 = CARTESIAN_POINT ( 'NONE',  ( 0.01209709964644558461, -32.52114463981743597, 7.635761828346577573 ) ) ;
#18339 = VERTEX_POINT ( 'NONE', #27414 ) ;
#18340 = CARTESIAN_POINT ( 'NONE',  ( 4.269670580072574495, -31.94665014585129725, 7.013842709614101167 ) ) ;
#18341 = LINE ( 'NONE', #21455, #31189 ) ;
#18342 = CARTESIAN_POINT ( 'NONE',  ( -30.44874870218064089, -26.64985754041175525, 6.700000000000000178 ) ) ;
#18343 = B_SPLINE_SURFACE_WITH_KNOTS ( 'NONE', 3, 1, ( 
 ( #17509, #29497 ),
 ( #4395, #30103 ),
 ( #26606, #11334 ),
 ( #26807, #23315 ),
 ( #24107, #14433 ),
 ( #27004, #39550 ),
 ( #4775, #30298 ),
 ( #11137, #2112 ),
 ( #14628, #32598 ),
 ( #1306, #23708 ),
 ( #26412, #39143 ),
 ( #38941, #23518 ),
 ( #17310, #1704 ),
 ( #14235, #27609 ),
 ( #3150, #18332 ),
 ( #40166, #36671 ),
 ( #34428, #11947 ),
 ( #8454, #21038 ),
 ( #11737, #27807 ),
 ( #15255, #14837 ),
 ( #31124, #17925 ),
 ( #9274, #8659 ),
 ( #2314, #18130 ),
 ( #21651, #15455 ),
 ( #30508, #9075 ),
 ( #39967, #21852 ),
 ( #40563, #33611 ),
 ( #21236, #37283 ),
 ( #30924, #5385 ),
 ( #27404, #2731 ),
 ( #36879, #24315 ) ),
 .UNSPECIFIED., .F., .F., .F.,
 ( 4, 3, 3, 3, 3, 3, 3, 3, 3, 3, 4 ),
 ( 2, 2 ),
 ( 0.000000000000000000, 0.1064040534484947675, 0.2127447817800691698, 0.3200334471358571298, 0.4279895727010789019, 0.5349334657245100599, 0.6407861787064421666, 0.7471238984184978005, 0.8547834834472670673, 0.9625789755878069176, 1.000000000000000000 ),
 ( 0.000000000000000000, 1.000000000000000000 ),
 .UNSPECIFIED. ) ;
#18344 = ORIENTED_EDGE ( 'NONE', *, *, #21958, .T. ) ;
#18345 = CARTESIAN_POINT ( 'NONE',  ( 8.290806648384990041, 0.000000000000000000, -2.500000000000000000 ) ) ;
#18346 = DIRECTION ( 'NONE',  ( 0.7541618601367554575, 0.000000000000000000, -0.6566885781822834334 ) ) ;
#18347 = EDGE_LOOP ( 'NONE', ( #12278, #25536, #6974, #33585 ) ) ;
#18348 = CARTESIAN_POINT ( 'NONE',  ( 24.65197495220076007, 2.989504840433797828, 3.507439046191596521 ) ) ;
#18349 = CARTESIAN_POINT ( 'NONE',  ( 82.59411735159429213, 63.56171878218356852, -1.145133701562419226 ) ) ;
#18350 = DIRECTION ( 'NONE',  ( -0.000000000000000000, -0.000000000000000000, -1.000000000000000000 ) ) ;
#18351 = ADVANCED_FACE ( 'NONE', ( #30517 ), #40174, .T. ) ;
#18352 = CARTESIAN_POINT ( 'NONE',  ( 79.98933190693155382, 64.46315002137730232, 3.592474444481858153 ) ) ;
#18353 = AXIS2_PLACEMENT_3D ( 'NONE', #6176, #37857, #15425 ) ;
#18354 = CARTESIAN_POINT ( 'NONE',  ( -0.08877474292672410394, -32.46112373979092069, 6.864651958020304257 ) ) ;
#18355 = VERTEX_POINT ( 'NONE', #30935 ) ;
#18356 = CARTESIAN_POINT ( 'NONE',  ( 77.90315483005265662, 60.81789388943194297, -3.308002540436226990 ) ) ;
#18358 = CARTESIAN_POINT ( 'NONE',  ( -42.44874870218064444, -26.64985754041175525, 6.700000000000000178 ) ) ;
#18357 = CARTESIAN_POINT ( 'NONE',  ( 3.947630499704354090, -32.24896051801510310, 7.767720160662275219 ) ) ;
#18359 = CARTESIAN_POINT ( 'NONE',  ( -63.96695182803187407, 19.27020452292898867, -9.800414904976365804 ) ) ;
#18360 = CARTESIAN_POINT ( 'NONE',  ( 81.24747667584206567, 63.59436251575137078, -3.343039074468323157 ) ) ;
#18361 = CARTESIAN_POINT ( 'NONE',  ( 77.25343114543986189, 63.60010822905029215, 3.597602401604568012 ) ) ;
#18362 = VERTEX_POINT ( 'NONE', #2327 ) ;
#18363 = VERTEX_POINT ( 'NONE', #37086 ) ;
#18364 = CARTESIAN_POINT ( 'NONE',  ( 1.688104973690869537, -26.06994794917929781, 7.756742906098588186 ) ) ;
#18365 = ADVANCED_FACE ( 'NONE', ( #24532 ), #2741, .T. ) ;
#18366 = ADVANCED_FACE ( 'NONE', ( #9084 ), #39977, .F. ) ;
#18367 = CARTESIAN_POINT ( 'NONE',  ( 82.29094429576495884, 64.52076745355572029, 1.905332024690495007 ) ) ;
#18369 = CARTESIAN_POINT ( 'NONE',  ( -1.577286183139641418, -30.79746357491616138, 7.670465701733744979 ) ) ;
#18368 = DIRECTION ( 'NONE',  ( -1.000000000000000000, 0.000000000000000000, 0.000000000000000000 ) ) ;
#18370 = CARTESIAN_POINT ( 'NONE',  ( 33.61282307965942806, -4.196488527906213406, -4.700131347630155609 ) ) ;
#18371 = CARTESIAN_POINT ( 'NONE',  ( -23.07867591359219617, -24.55319635012989110, 6.700000000000000178 ) ) ;
#18372 = FACE_OUTER_BOUND ( 'NONE', #6729, .T. ) ;
#18373 = CARTESIAN_POINT ( 'NONE',  ( -62.76544114002936681, 35.76323014769233311, 5.464922856233965121 ) ) ;
#18374 = CARTESIAN_POINT ( 'NONE',  ( 25.98198111045553205, 0.8794612723162963386, -4.427497433388436932 ) ) ;
#18375 = AXIS2_PLACEMENT_3D ( 'NONE', #28063, #35825, #7600 ) ;
#18376 = DIRECTION ( 'NONE',  ( -0.000000000000000000, 1.000000000000000000, -0.000000000000000000 ) ) ;
#18377 = FACE_OUTER_BOUND ( 'NONE', #29446, .T. ) ;
#18378 = DIRECTION ( 'NONE',  ( -1.000000000000000000, 0.000000000000000000, 0.000000000000000000 ) ) ;
#18379 = CARTESIAN_POINT ( 'NONE',  ( -1.799609906766908685, -29.56993018339339940, 6.929570838012926615 ) ) ;
#18380 = CARTESIAN_POINT ( 'NONE',  ( 30.81598109780163952, 0.5927272948842338129, -4.684903830278420500 ) ) ;
#18381 = CARTESIAN_POINT ( 'NONE',  ( 4.458039033310292609, -27.41499233908904287, 7.754798119455333705 ) ) ;
#18382 = LINE ( 'NONE', #15092, #30146 ) ;
#18383 = FACE_OUTER_BOUND ( 'NONE', #28308, .T. ) ;
#18384 =( BOUNDED_CURVE ( )  B_SPLINE_CURVE ( 3, ( #7797, #20349, #1637, #36210 ),
 .UNSPECIFIED., .F., .T. ) 
 B_SPLINE_CURVE_WITH_KNOTS ( ( 4, 4 ),
 ( 4.748221474220560623, 4.941946782021394924 ),
 .UNSPECIFIED. ) 
 CURVE ( )  GEOMETRIC_REPRESENTATION_ITEM ( )  RATIONAL_B_SPLINE_CURVE ( ( 1.000000000000000000, 0.9968749865767494445, 0.9968749865767494445, 1.000000000000000000 ) ) 
 REPRESENTATION_ITEM ( '' )  );
#18385 = CARTESIAN_POINT ( 'NONE',  ( 0.5148699040292038509, -32.86303942011277712, 7.756742906098588186 ) ) ;
#18386 = LINE ( 'NONE', #28266, #28623 ) ;
#18387 = DIRECTION ( 'NONE',  ( 0.000000000000000000, 0.000000000000000000, 1.000000000000000000 ) ) ;
#18388 = EDGE_CURVE ( 'NONE', #28508, #9457, #24326, .T. ) ;
#18389 = CARTESIAN_POINT ( 'NONE',  ( -70.92837670882140344, -21.78291075931342391, 6.000000000000002665 ) ) ;
#18390 = CARTESIAN_POINT ( 'NONE',  ( 24.08254445156938317, 2.354971793711281958, -4.219079743025244689 ) ) ;
#18391 = VECTOR ( 'NONE', #8226, 1000.000000000000000 ) ;
#18392 = EDGE_LOOP ( 'NONE', ( #27040, #39921, #17732, #8011 ) ) ;
#18393 = CARTESIAN_POINT ( 'NONE',  ( -19.07867591359219972, -26.64985754041175525, 6.800000000000000711 ) ) ;
#18394 = CARTESIAN_POINT ( 'NONE',  ( 70.83363217041421933, 59.75074159095914439, -3.963404584535426434 ) ) ;
#18395 = ORIENTED_EDGE ( 'NONE', *, *, #2553, .F. ) ;
#18396 = CARTESIAN_POINT ( 'NONE',  ( 87.68638643695580015, -2.222987235672965411, -2.753905389729575326 ) ) ;
#18397 = CARTESIAN_POINT ( 'NONE',  ( -1.654012860102806570, -29.01496998062980381, 7.695279973900954751 ) ) ;
#18398 = CARTESIAN_POINT ( 'NONE',  ( 3.052721860142450172, -26.45044204593990145, 6.920489980334479263 ) ) ;
#18399 = EDGE_CURVE ( 'NONE', #20773, #8017, #35910, .T. ) ;
#18400 = EDGE_CURVE ( 'NONE', #29312, #21972, #15264, .T. ) ;
#18401 = CARTESIAN_POINT ( 'NONE',  ( 1.307444196246471124, -26.19270861743451206, 6.911401339314954484 ) ) ;
#18402 = APPLICATION_PROTOCOL_DEFINITION ( 'draft international standard', 'automotive_design', 1998, #18152 ) ;
#18403 = DIRECTION ( 'NONE',  ( 0.000000000000000000, 0.000000000000000000, 1.000000000000000000 ) ) ;
#18404 = ORIENTED_EDGE ( 'NONE', *, *, #33263, .T. ) ;
#18405 = EDGE_CURVE ( 'NONE', #18458, #5730, #10896, .T. ) ;
#18406 = AXIS2_PLACEMENT_3D ( 'NONE', #10007, #28961, #29361 ) ;
#18407 = VERTEX_POINT ( 'NONE', #21049 ) ;
#18408 = EDGE_LOOP ( 'NONE', ( #11460, #10097, #31099, #5721 ) ) ;
#18409 = CARTESIAN_POINT ( 'NONE',  ( 80.39537321288027272, 61.58102678004055264, -2.797036776683079040 ) ) ;
#18410 = LINE ( 'NONE', #18203, #26940 ) ;
#18411 = CARTESIAN_POINT ( 'NONE',  ( 81.16673370561979084, 65.10603640127597203, -2.903340743335492302 ) ) ;
#18412 = CARTESIAN_POINT ( 'NONE',  ( 80.76403243373638929, 61.15693784680268408, 1.612955153530313268 ) ) ;
#18413 = VERTEX_POINT ( 'NONE', #17725 ) ;
#18414 = DIRECTION ( 'NONE',  ( -0.8660254037844415942, 0.4999999999999950040, -0.000000000000000000 ) ) ;
#18415 = CARTESIAN_POINT ( 'NONE',  ( 4.899937972425366439, -30.72010120057137073, 7.635761828346577573 ) ) ;
#18416 = CARTESIAN_POINT ( 'NONE',  ( 22.32844273176644379, 5.552903595841022444, -4.279453667248723114 ) ) ;
#18417 = VERTEX_POINT ( 'NONE', #8669 ) ;
#18418 = CARTESIAN_POINT ( 'NONE',  ( -72.17678919972044582, 5.298235119234846913, 9.922868473773599263 ) ) ;
#18419 = CARTESIAN_POINT ( 'NONE',  ( 37.17104416159511970, -2.975766693752441405, 5.995325537273664018 ) ) ;
#18420 = DIRECTION ( 'NONE',  ( 0.000000000000000000, 0.000000000000000000, 1.000000000000000000 ) ) ;
#18421 = CARTESIAN_POINT ( 'NONE',  ( -81.79890681550139675, 10.46299657128043492, 0.6911394749367770762 ) ) ;
#18422 = CARTESIAN_POINT ( 'NONE',  ( 32.90341074813867550, -3.215396174707138677, -5.341771038058501730 ) ) ;
#18423 = CARTESIAN_POINT ( 'NONE',  ( 37.10444278664265028, -3.126632674519886468, -5.976181500518823242 ) ) ;
#18424 = CARTESIAN_POINT ( 'NONE',  ( 5.141684319425215755, -30.20828278875847062, 6.894806418505347700 ) ) ;
#18425 = CARTESIAN_POINT ( 'NONE',  ( -4.224659823956008253, -51.67615071827237472, 6.000000000000000000 ) ) ;
#18426 = DIRECTION ( 'NONE',  ( -0.000000000000000000, -0.000000000000000000, 1.000000000000000000 ) ) ;
#18427 = CARTESIAN_POINT ( 'NONE',  ( -69.08758708074093136, 36.88538962427716683, -8.800414904976364028 ) ) ;
#18428 = CARTESIAN_POINT ( 'NONE',  ( -75.45330471031414277, 33.71485196875532608, 8.800414904976364028 ) ) ;
#18429 = VECTOR ( 'NONE', #10030, 1000.000000000000000 ) ;
#18430 = EDGE_CURVE ( 'NONE', #16055, #23873, #40367, .T. ) ;
#18431 = CARTESIAN_POINT ( 'NONE',  ( 3.901280325574687957, -32.16147924937965996, 7.643333865083956624 ) ) ;
#18432 = CARTESIAN_POINT ( 'NONE',  ( 36.87286983558979614, -2.097983711965031528, -5.866507389336803158 ) ) ;
#18433 = CARTESIAN_POINT ( 'NONE',  ( 24.58590238555413876, 2.979194303875008387, -3.570749183279829264 ) ) ;
#18434 = EDGE_LOOP ( 'NONE', ( #21393, #15263, #33431, #25736, #25373, #15786, #27159, #29301 ) ) ;
#18435 = CARTESIAN_POINT ( 'NONE',  ( 67.18400333313441308, 57.97000644093014188, 3.997693602769901045 ) ) ;
#18436 = CARTESIAN_POINT ( 'NONE',  ( 35.50430187872925103, -1.785329816699790184, 5.747703001598215344 ) ) ;
#18437 = CARTESIAN_POINT ( 'NONE',  ( -1.663744362731840676, -30.06256111737130965, 7.774064877406527962 ) ) ;
#18438 = EDGE_CURVE ( 'NONE', #34397, #6604, #17935, .T. ) ;
#18439 = CARTESIAN_POINT ( 'NONE',  ( 13.52694889643372278, 17.29870644234688370, 2.500000000000000000 ) ) ;
#18441 = EDGE_CURVE ( 'NONE', #3524, #744, #5604, .T. ) ;
#18440 = CARTESIAN_POINT ( 'NONE',  ( 88.51539661956502414, -1.738042312505858389, 3.005881034771096250 ) ) ;
#18442 = CIRCLE ( 'NONE', #26972, 1.000000000000005551 ) ;
#18444 = CARTESIAN_POINT ( 'NONE',  ( 37.02167662054689146, -2.764188933150113048, -5.984526027905666901 ) ) ;
#18443 = DIRECTION ( 'NONE',  ( 0.000000000000000000, 0.000000000000000000, 1.000000000000000000 ) ) ;
#18445 = VERTEX_POINT ( 'NONE', #9703 ) ;
#18446 = CARTESIAN_POINT ( 'NONE',  ( 24.63695973801421957, 2.986857212966991248, 3.523430893224142935 ) ) ;
#18447 = CARTESIAN_POINT ( 'NONE',  ( 5.200390093233090205, -29.56993018339339940, 7.620413589471895399 ) ) ;
#18448 = ADVANCED_FACE ( 'NONE', ( #6629, #52, #28648, #3962, #35250, #456, #16481, #10100, #15677, #6420, #13197, #28225, #38103, #21861, #25765, #29053, #9488, #861, #3159, #12994, #6215, #7020, #22685, #25967, #22484, #31951, #34852, #19588, #34436, #22074, #13393, #12582, #25559, #18760, #25148, #9905, #35050, #37683, #32164, #31335, #31740, #34649, #18976, #9282, #31540, #15879, #3757, #28437, #245, #6826, #12783, #25358 ), #37896, .T. ) ;
#18449 = EDGE_LOOP ( 'NONE', ( #30114, #28287, #31147, #605 ) ) ;
#18450 = DIRECTION ( 'NONE',  ( 1.000000000000000000, 0.000000000000000000, 0.000000000000000000 ) ) ;
#18451 = PRODUCT_DEFINITION_CONTEXT ( 'detailed design', #39741, 'design' ) ;
#18452 = EDGE_LOOP ( 'NONE', ( #11257, #14093, #13358, #35623 ) ) ;
#18453 = ORIENTED_EDGE ( 'NONE', *, *, #15482, .T. ) ;
#18454 = CARTESIAN_POINT ( 'NONE',  ( 79.01373585440697411, 65.47072129778472060, -2.830664096605183033 ) ) ;
#18455 = CARTESIAN_POINT ( 'NONE',  ( 4.978659405551939088, -28.32469115355010914, 7.255881584735162981 ) ) ;
#18456 = CARTESIAN_POINT ( 'NONE',  ( 80.36115745751311579, 63.17601289530517761, 3.638935937159312850 ) ) ;
#18458 = VERTEX_POINT ( 'NONE', #3555 ) ;
#18457 = CARTESIAN_POINT ( 'NONE',  ( -0.8361945232212143475, -27.30589628897558896, 6.864651958020303368 ) ) ;
#18459 = AXIS2_PLACEMENT_3D ( 'NONE', #39139, #20604, #32593 ) ;
#18460 = CARTESIAN_POINT ( 'NONE',  ( 0.05705130999228511662, -26.47997509747052192, 7.754798119455333705 ) ) ;
#18462 = FACE_OUTER_BOUND ( 'NONE', #21428, .T. ) ;
#18461 = CARTESIAN_POINT ( 'NONE',  ( 4.921350899141003765, -30.93938997316396566, 6.989977667959438534 ) ) ;
#18463 = CARTESIAN_POINT ( 'NONE',  ( -71.92837670882107659, -20.91513571952110340, 9.949874371066202983 ) ) ;
#18464 = CARTESIAN_POINT ( 'NONE',  ( -54.79610818216033152, 31.51396769785350926, 1.000000000000000000 ) ) ;
#18465 = CARTESIAN_POINT ( 'NONE',  ( 24.35951259229402055, 3.143687006796874517, -3.365150753154290353 ) ) ;
#18466 = EDGE_LOOP ( 'NONE', ( #33310, #32274, #38006, #20459 ) ) ;
#18467 = DIRECTION ( 'NONE',  ( 1.224646799147353207E-16, 1.000000000000000000, -0.000000000000000000 ) ) ;
#18468 = CARTESIAN_POINT ( 'NONE',  ( 25.22633673370294360, -3.172752697882940343, -5.351597462314125586 ) ) ;
#18469 = DIRECTION ( 'NONE',  ( 0.02975940812527386875, -0.9995570907297058882, 0.000000000000000000 ) ) ;
#18470 = CARTESIAN_POINT ( 'NONE',  ( 5.006037652185061582, -30.36535116702205883, 6.969307238440507923 ) ) ;
#18471 = CARTESIAN_POINT ( 'NONE',  ( 81.38674634791392748, 61.68395714348712033, 2.028924249969739080 ) ) ;
#18472 = CARTESIAN_POINT ( 'NONE',  ( 86.86785128967072467, -0.4505172232112327757, -5.755800129507335328 ) ) ;
#18473 = FACE_OUTER_BOUND ( 'NONE', #7768, .T. ) ;
#18474 = ORIENTED_EDGE ( 'NONE', *, *, #34982, .F. ) ;
#18475 = CARTESIAN_POINT ( 'NONE',  ( -64.16206517525715469, 35.04753771064019929, -4.696770012396532579 ) ) ;
#18476 = CARTESIAN_POINT ( 'NONE',  ( 3.498496326533036882, -26.68430824457884398, 6.864276522220859711 ) ) ;
#18477 = CARTESIAN_POINT ( 'NONE',  ( 3.992140197745001728, -26.92457926934255141, 6.875671892026062437 ) ) ;
#18478 = CARTESIAN_POINT ( 'NONE',  ( 23.83742322420201276, -3.141359013241465714, -3.807232997737503677 ) ) ;
#18479 = FACE_OUTER_BOUND ( 'NONE', #32044, .T. ) ;
#18480 = CARTESIAN_POINT ( 'NONE',  ( 1.825221044428271044, -26.17220649359113338, 6.863904403958575706 ) ) ;
#18481 = ORIENTED_EDGE ( 'NONE', *, *, #23836, .F. ) ;
#18482 = CARTESIAN_POINT ( 'NONE',  ( 36.79712590745128864, -2.556887556061694600, 5.949479458347596506 ) ) ;
#18483 = CARTESIAN_POINT ( 'NONE',  ( 85.88709644997106807, 1.885261416588465799, 4.127327262050844325 ) ) ;
#18484 = ORIENTED_EDGE ( 'NONE', *, *, #28132, .T. ) ;
#18486 = CARTESIAN_POINT ( 'NONE',  ( -63.99293516169446150, 35.89893413629672381, 7.506047544094577084 ) ) ;
#18485 = CARTESIAN_POINT ( 'NONE',  ( 79.08570711028920641, 65.99300539798551313, -2.058202901128790785 ) ) ;
#18487 =( BOUNDED_CURVE ( )  B_SPLINE_CURVE ( 3, ( #26510, #26710, #10842, #39244 ),
 .UNSPECIFIED., .F., .F. ) 
 B_SPLINE_CURVE_WITH_KNOTS ( ( 4, 4 ),
 ( 1.347909859412853795, 1.534781240595298746 ),
 .UNSPECIFIED. ) 
 CURVE ( )  GEOMETRIC_REPRESENTATION_ITEM ( )  RATIONAL_B_SPLINE_CURVE ( ( 1.000000000000000000, 0.9970920404276226723, 0.9970920404276226723, 1.000000000000000000 ) ) 
 REPRESENTATION_ITEM ( '' )  );
#18488 = CARTESIAN_POINT ( 'NONE',  ( 22.09655393983083371, -2.652383328716616973, 3.655099668123841905 ) ) ;
#18489 = CARTESIAN_POINT ( 'NONE',  ( -17.69482985384421880, -29.56993018339339940, -6.000000000000000000 ) ) ;
#18490 = CARTESIAN_POINT ( 'NONE',  ( 21.58863023475808873, 7.202558683720228672, -2.923977588977705544 ) ) ;
#18491 = EDGE_CURVE ( 'NONE', #14653, #12843, #16082, .T. ) ;
#18492 = VERTEX_POINT ( 'NONE', #28852 ) ;
#18493 = B_SPLINE_CURVE_WITH_KNOTS ( 'NONE', 3,
 ( #27779, #5969, #18934, #12544, #18510, #34404, #2906, #6591, #15638, #37645, #11918, #27985, #9450, #40532, #12340, #22032, #34609, #12747, #3323, #24913, #37449, #15842, #27585, #206, #25324, #40137, #37048, #8834, #21418, #7377, #32318, #6785, #19742, #3926, #16440, #25722, #38066, #13351, #19935, #38663, #16833, #38458, #25926, #28609, #31909, #35414, #4117, #20135, #10262, #3519, #417, #35011, #12956, #3721, #22443, #13161, #32125, #26132, #1024, #19339 ),
 .UNSPECIFIED., .F., .F.,
 ( 4, 1, 2, 2, 1, 1, 1, 1, 2, 2, 1, 1, 1, 1, 1, 2, 2, 1, 1, 1, 1, 2, 2, 1, 1, 1, 1, 1, 2, 2, 1, 1, 1, 1, 1, 1, 2, 2, 1, 1, 1, 1, 1, 2, 4 ),
 ( 0.000000000000000000, 0.03125000000000305311, 0.03515625000000274780, 0.03906250000000244249, 0.04687500000000294209, 0.05468750000000344169, 0.05859375000000369149, 0.06054687500000378170, 0.06152343750000379557, 0.06250000000000380251, 0.09374999999998534506, 0.1093749999999761024, 0.1171874999999714534, 0.1210937499999693440, 0.1230468749999680672, 0.1240234374999676509, 0.1249999999999672345, 0.1874999999999666656, 0.2187499999999664990, 0.2343749999999664158, 0.2421874999999664158, 0.2460937499999664158, 0.2499999999999664158, 0.3124999999999670264, 0.3437499999999674150, 0.3593749999999675815, 0.3671874999999676925, 0.3710937499999676370, 0.3730468749999676370, 0.3749999999999675815, 0.4062499999999664158, 0.4218749999999655831, 0.4296874999999649170, 0.4335937499999643063, 0.4355468749999643063, 0.4365234374999645839, 0.4370117187499647504, 0.4374999999999649170, 0.4687499999999821254, 0.4843749999999903411, 0.4921874999999944489, 0.4960937499999965583, 0.4980468749999982792, 0.4990234374999991118, 0.5000000000000000000 ),
 .UNSPECIFIED. ) ;
#18494 = EDGE_CURVE ( 'NONE', #20325, #21904, #660, .T. ) ;
#18495 = CARTESIAN_POINT ( 'NONE',  ( 27.68906107752918189, -4.318180587071351439, -3.785118428133491530 ) ) ;
#18496 = EDGE_CURVE ( 'NONE', #16084, #30583, #39167, .T. ) ;
#18497 = VERTEX_POINT ( 'NONE', #39103 ) ;
#18498 = CIRCLE ( 'NONE', #23761, 7.999999999999992895 ) ;
#18499 = EDGE_CURVE ( 'NONE', #36144, #8080, #39308, .T. ) ;
#18500 = ORIENTED_EDGE ( 'NONE', *, *, #17506, .T. ) ;
#18501 = CARTESIAN_POINT ( 'NONE',  ( 80.46181058475264081, 63.58258928487767037, -3.654032574946328271 ) ) ;
#18502 = CARTESIAN_POINT ( 'NONE',  ( -59.46024017484872815, 26.94883531126003007, -5.502890977078439327 ) ) ;
#18503 = ORIENTED_EDGE ( 'NONE', *, *, #31024, .T. ) ;
#18505 = CARTESIAN_POINT ( 'NONE',  ( -70.92837670882107659, 26.72470171467712063, 0.000000000000000000 ) ) ;
#18504 = CARTESIAN_POINT ( 'NONE',  ( 24.12638665588002596, 2.663754577735522489, 3.995026624097451240 ) ) ;
#18506 = ORIENTED_EDGE ( 'NONE', *, *, #25251, .T. ) ;
#18507 = CARTESIAN_POINT ( 'NONE',  ( 81.98137654593473655, 62.63634409986672580, -2.334361474589122132 ) ) ;
#18508 = CARTESIAN_POINT ( 'NONE',  ( 4.668948836787977896, -27.91232378075620701, 6.894806418505348589 ) ) ;
#18510 = CARTESIAN_POINT ( 'NONE',  ( 86.47917723929778333, 1.220208172167279503, -4.908343648090710332 ) ) ;
#18509 = CARTESIAN_POINT ( 'NONE',  ( 5.751251297819365504, -26.64985754041175525, 6.700000000000000178 ) ) ;
#18511 = DIRECTION ( 'NONE',  ( 0.3754033771448229140, 0.6502177225477935307, -0.6605219282605403475 ) ) ;
#18512 = CARTESIAN_POINT ( 'NONE',  ( 0.5718647330646855487, -26.27158218865373129, 7.784725160561909441 ) ) ;
#18513 = CARTESIAN_POINT ( 'NONE',  ( 73.91602183453733232, 60.46016365699546924, 3.923277237800832928 ) ) ;
#18514 = CARTESIAN_POINT ( 'NONE',  ( 23.07119635075321185, 3.097555360989402651, -4.080821451665009647 ) ) ;
#18515 = ORIENTED_EDGE ( 'NONE', *, *, #24126, .T. ) ;
#18516 = CARTESIAN_POINT ( 'NONE',  ( 4.460814650971867579, -27.41817363093848314, 7.750000000000000888 ) ) ;
#18517 = CARTESIAN_POINT ( 'NONE',  ( 21.85643539959773207, -2.612013071670181041, -15.99649826491319971 ) ) ;
#18518 = CARTESIAN_POINT ( 'NONE',  ( 0.9213240864078056092, -26.64985754041175525, 6.700000000000000178 ) ) ;
#18519 = VERTEX_POINT ( 'NONE', #13806 ) ;
#18520 = ORIENTED_EDGE ( 'NONE', *, *, #39068, .F. ) ;
#18521 = CARTESIAN_POINT ( 'NONE',  ( -54.79610818216088575, 31.51396769785300123, -1.028983900456674538 ) ) ;
#18522 = CARTESIAN_POINT ( 'NONE',  ( 81.77617677873431035, 62.02699640077097598, 2.046910133536369969 ) ) ;
#18523 = CARTESIAN_POINT ( 'NONE',  ( 86.62997685915109969, 1.050822881766228845, -5.316720303788503799 ) ) ;
#18524 = ORIENTED_EDGE ( 'NONE', *, *, #449, .F. ) ;
#18525 = CARTESIAN_POINT ( 'NONE',  ( -64.08758708074093136, 38.34299140179469134, 3.014629887202059155 ) ) ;
#18526 = CARTESIAN_POINT ( 'NONE',  ( 14.93019310335909111, -6.111523010399976918, 2.531807211659590884 ) ) ;
#18527 = CARTESIAN_POINT ( 'NONE',  ( 1.075343990422650275, -26.12619373866192873, 7.640616322432101093 ) ) ;
#18528 = AXIS2_PLACEMENT_3D ( 'NONE', #12748, #12341, #25325 ) ;
#18529 = CARTESIAN_POINT ( 'NONE',  ( 36.44800439370845169, -2.352474353827100018, -5.894990602592409701 ) ) ;
#18530 = CARTESIAN_POINT ( 'NONE',  ( 5.140967908914694462, -28.99159849420241741, 7.781480525794719938 ) ) ;
#18531 = DIRECTION ( 'NONE',  ( 0.4690749385695657803, 0.8831583674551003460, -0.000000000000000000 ) ) ;
#18532 = VERTEX_POINT ( 'NONE', #29256 ) ;
#18533 = CIRCLE ( 'NONE', #19227, 0.1000000000000028644 ) ;
#18534 = DIRECTION ( 'NONE',  ( 0.000000000000000000, 0.000000000000000000, 1.000000000000000000 ) ) ;
#18535 = CARTESIAN_POINT ( 'NONE',  ( 1.719724692003898658, -33.06987729247488517, 7.747520101777647383 ) ) ;
#18536 = EDGE_LOOP ( 'NONE', ( #13045, #21530, #14338, #6643 ) ) ;
#18537 = ORIENTED_EDGE ( 'NONE', *, *, #19124, .T. ) ;
#18538 = CARTESIAN_POINT ( 'NONE',  ( 33.88294556138480118, -0.6033199263786843680, 5.261213554215595778 ) ) ;
#18539 = PLANE ( 'NONE',  #813 ) ;
#18540 = CARTESIAN_POINT ( 'NONE',  ( 66.81418162778464875, 58.07599004166701206, -3.996206253860483226 ) ) ;
#18541 = ORIENTED_EDGE ( 'NONE', *, *, #15327, .F. ) ;
#18542 = CARTESIAN_POINT ( 'NONE',  ( -55.42153689335682998, 31.50958069423711549, 3.999999999999998668 ) ) ;
#18544 = EDGE_CURVE ( 'NONE', #6683, #2116, #17468, .T. ) ;
#18543 = CARTESIAN_POINT ( 'NONE',  ( -77.51841857730454421, -6.230424868427139273, -7.532757448271641287 ) ) ;
#18545 = CARTESIAN_POINT ( 'NONE',  ( -68.92837670882107659, -42.87473357531881391, 0.000000000000000000 ) ) ;
#18546 = EDGE_LOOP ( 'NONE', ( #24527, #20605, #39976, #24621, #26907, #30733, #13107, #33968 ) ) ;
#18547 = DIRECTION ( 'NONE',  ( 1.000000000000000000, 0.000000000000000000, 0.000000000000000000 ) ) ;
#18548 = CARTESIAN_POINT ( 'NONE',  ( -1.744066689084928345, -30.19099175420856440, 7.635761828346576685 ) ) ;
#18549 = ORIENTED_EDGE ( 'NONE', *, *, #38202, .T. ) ;
#18550 = CARTESIAN_POINT ( 'NONE',  ( 24.71585255522903779, 3.004271553411825835, 3.424932163101386706 ) ) ;
#18551 = CARTESIAN_POINT ( 'NONE',  ( 81.30214557805295783, 65.90511036421341373, -1.555014038483378158 ) ) ;
#18552 = CARTESIAN_POINT ( 'NONE',  ( 80.91556171499748018, 62.42588715431494961, 3.188730975143402091 ) ) ;
#18553 = CARTESIAN_POINT ( 'NONE',  ( -0.05515801212132670495, -32.48165012009213370, 6.880147297696981745 ) ) ;
#18554 = VERTEX_POINT ( 'NONE', #10303 ) ;
#18555 = CARTESIAN_POINT ( 'NONE',  ( 76.63461511614536903, 62.03359853006622870, -3.872369636031699258 ) ) ;
#18557 = LINE ( 'NONE', #256, #1345 ) ;
#18556 = CYLINDRICAL_SURFACE ( 'NONE', #22643, 0.09010775117053000660 ) ;
#18558 = CARTESIAN_POINT ( 'NONE',  ( 14.86212623557473478, 12.07207427411234768, -2.525992259579474375 ) ) ;
#18559 = CARTESIAN_POINT ( 'NONE',  ( 79.15160802321746303, 66.03480532732676522, -2.011547652602700076 ) ) ;
#18560 = CARTESIAN_POINT ( 'NONE',  ( 77.67868059383667401, 64.13990294438296758, 3.401348408886265329 ) ) ;
#18561 = CIRCLE ( 'NONE', #23811, 1.000000000000000000 ) ;
#18562 = ORIENTED_EDGE ( 'NONE', *, *, #31254, .F. ) ;
#18563 = CARTESIAN_POINT ( 'NONE',  ( 4.748716522672954632, -31.28972995975264837, 7.678495282201404315 ) ) ;
#18564 = DIRECTION ( 'NONE',  ( 0.000000000000000000, -1.000000000000000000, 0.000000000000000000 ) ) ;
#18565 = CARTESIAN_POINT ( 'NONE',  ( 81.44533364721146995, 61.45470812716254727, 1.173033592341437004 ) ) ;
#18567 = CARTESIAN_POINT ( 'NONE',  ( -1.693306178808691609, -29.36295009413090540, 6.979335674598003969 ) ) ;
#18566 = CARTESIAN_POINT ( 'NONE',  ( -64.08758708074094557, 43.44410442557501995, 1.728127058819059814 ) ) ;
#18568 = CARTESIAN_POINT ( 'NONE',  ( 33.81722006525239266, -4.984950771528167124, -3.153948780582495726 ) ) ;
#18569 = EDGE_CURVE ( 'NONE', #25263, #833, #24700, .T. ) ;
#18570 = DIRECTION ( 'NONE',  ( 1.000000000000000000, 0.000000000000000000, 0.000000000000000000 ) ) ;
#18571 = PLANE ( 'NONE',  #24608 ) ;
#18572 = CARTESIAN_POINT ( 'NONE',  ( -64.43126815475770286, 34.69310041339028317, 5.627269573384544366 ) ) ;
#18573 = CARTESIAN_POINT ( 'NONE',  ( 21.73547365326574621, 0.2723378343146318215, -8.960011461284089762 ) ) ;
#18574 = DIRECTION ( 'NONE',  ( 0.3420201433256790380, -0.9396926207859046531, -0.000000000000000000 ) ) ;
#18575 = FACE_OUTER_BOUND ( 'NONE', #18723, .T. ) ;
#18576 = CARTESIAN_POINT ( 'NONE',  ( 5.198171123944452354, -29.69454897310232155, 7.751599049952198506 ) ) ;
#18577 = CARTESIAN_POINT ( 'NONE',  ( -38.44874870218063734, -25.49307895267003587, 6.700000000000000178 ) ) ;
#18578 = CARTESIAN_POINT ( 'NONE',  ( 29.42001906605359451, 1.119432858802278830, -4.432475847736385255 ) ) ;
#18579 = CARTESIAN_POINT ( 'NONE',  ( 8.290806648384990041, 0.000000000000000000, 6.000000000000000000 ) ) ;
#18580 = DIRECTION ( 'NONE',  ( -0.9848077530122092416, 0.1736481776669241694, -0.000000000000000000 ) ) ;
#18581 = CARTESIAN_POINT ( 'NONE',  ( -0.9113260236350476662, -31.74685638300427826, 7.775108481317166031 ) ) ;
#18582 = LINE ( 'NONE', #40011, #13376 ) ;
#18583 = CARTESIAN_POINT ( 'NONE',  ( -35.07867591359219972, -26.64985754041175525, 6.700000000000000178 ) ) ;
#18584 = B_SPLINE_CURVE_WITH_KNOTS ( 'NONE', 3,
 ( #26097, #25287, #19511, #6555, #25484, #13314, #6348, #382, #16406, #19100 ),
 .UNSPECIFIED., .F., .F.,
 ( 4, 3, 3, 4 ),
 ( 0.0001585009270395775123, 0.0001815657551981816192, 0.0002118214035944121802, 0.0002170292169044816383 ),
 .UNSPECIFIED. ) ;
#18585 = LINE ( 'NONE', #15305, #7044 ) ;
#18586 = ADVANCED_FACE ( 'NONE', ( #16670 ), #22881, .T. ) ;
#18587 = CARTESIAN_POINT ( 'NONE',  ( 21.44690707717986911, 7.928456536348717165, 2.757011952239331265 ) ) ;
#18588 = CARTESIAN_POINT ( 'NONE',  ( -1.535120485362819753, -30.61471740307679568, 6.863904403958576594 ) ) ;
#18589 = EDGE_LOOP ( 'NONE', ( #2312, #8767, #2420, #7022 ) ) ;
#18590 = EDGE_LOOP ( 'NONE', ( #31539, #7314, #12782, #26386 ) ) ;
#18591 = DIRECTION ( 'NONE',  ( 0.9848077530122103518, -0.1736481776669172583, -0.000000000000000000 ) ) ;
#18592 = CARTESIAN_POINT ( 'NONE',  ( 69.82526079983220768, 58.91932963963509451, -3.982895692900140894 ) ) ;
#18593 = VECTOR ( 'NONE', #21862, 1000.000000000000000 ) ;
#18594 = VERTEX_POINT ( 'NONE', #1461 ) ;
#18595 = DIRECTION ( 'NONE',  ( 0.000000000000000000, 0.000000000000000000, 1.000000000000000000 ) ) ;
#18597 = ADVANCED_FACE ( 'NONE', ( #10501 ), #11025, .T. ) ;
#18596 = FACE_OUTER_BOUND ( 'NONE', #18062, .T. ) ;
#18598 = CARTESIAN_POINT ( 'NONE',  ( 5.023800704533929462, -28.47218391387568204, 6.863784140767622333 ) ) ;
#18599 = DIRECTION ( 'NONE',  ( -0.000000000000000000, 1.000000000000000000, -0.000000000000000000 ) ) ;
#18600 = CARTESIAN_POINT ( 'NONE',  ( 5.052941056949534548, -30.13600185428053635, 7.740055089680399902 ) ) ;
#18601 = VERTEX_POINT ( 'NONE', #37242 ) ;
#18602 = CARTESIAN_POINT ( 'NONE',  ( 22.38252468730212996, 4.953197636376286184, 3.028858097227504320 ) ) ;
#18603 = DIRECTION ( 'NONE',  ( 0.000000000000000000, 0.000000000000000000, 1.000000000000000000 ) ) ;
#18604 = ORIENTED_EDGE ( 'NONE', *, *, #25900, .F. ) ;
#18605 = CARTESIAN_POINT ( 'NONE',  ( 80.57587054825803818, 61.08954103313657669, -1.748505333477117452 ) ) ;
#18606 = CARTESIAN_POINT ( 'NONE',  ( -1.482088180267138622, -30.76652202637871625, 7.695279973900954751 ) ) ;
#18607 = CARTESIAN_POINT ( 'NONE',  ( 79.63061436091753365, 66.14207560456340218, -2.046910133536484100 ) ) ;
#18608 = CARTESIAN_POINT ( 'NONE',  ( 78.47662320409183678, 65.68507013823818852, 2.197205184446135107 ) ) ;
#18609 = EDGE_CURVE ( 'NONE', #4341, #13150, #27824, .T. ) ;
#18610 = CARTESIAN_POINT ( 'NONE',  ( 4.421861210295527478, -27.53188506292452686, 6.895222827070019989 ) ) ;
#18611 =( BOUNDED_CURVE ( )  B_SPLINE_CURVE ( 3, ( #24658, #30855, #36605, #11669 ),
 .UNSPECIFIED., .F., .T. ) 
 B_SPLINE_CURVE_WITH_KNOTS ( ( 4, 4 ),
 ( 1.381924640371166690, 1.574767692156074483 ),
 .UNSPECIFIED. ) 
 CURVE ( )  GEOMETRIC_REPRESENTATION_ITEM ( )  RATIONAL_B_SPLINE_CURVE ( ( 1.000000000000000000, 0.9969033633783033199, 0.9969033633783033199, 1.000000000000000000 ) ) 
 REPRESENTATION_ITEM ( '' )  );
#18612 = B_SPLINE_CURVE_WITH_KNOTS ( 'NONE', 3,
 ( #35529, #5025, #20658, #1959, #30351, #36520, #35927, #27245, #8091, #36321 ),
 .UNSPECIFIED., .F., .F.,
 ( 4, 3, 3, 4 ),
 ( 0.0002170292169044774099, 0.0002420761345915964716, 0.0002723302478207020459, 0.0002816811360866753916 ),
 .UNSPECIFIED. ) ;
#18613 = CARTESIAN_POINT ( 'NONE',  ( 2.761442704594925246, -32.80013489931718595, 7.768425012602591551 ) ) ;
#18614 = CARTESIAN_POINT ( 'NONE',  ( 21.85643539959774273, 9.255709152629782110, 0.01215589129642568461 ) ) ;
#18615 = CARTESIAN_POINT ( 'NONE',  ( -31.07867591359219617, -24.55319635012989110, 6.700000000000000178 ) ) ;
#18616 = ORIENTED_EDGE ( 'NONE', *, *, #26909, .T. ) ;
#18617 = CARTESIAN_POINT ( 'NONE',  ( -72.46955098809822005, 6.128517033932898705, 9.881631157665120568 ) ) ;
#18618 = LINE ( 'NONE', #31205, #14778 ) ;
#18619 = CARTESIAN_POINT ( 'NONE',  ( -0.1551898507743131317, -32.53746921202473175, 7.753200566781576875 ) ) ;
#18620 = CARTESIAN_POINT ( 'NONE',  ( 1.629959277500286685, -32.96921550338401374, 7.784476445165072533 ) ) ;
#18621 = CARTESIAN_POINT ( 'NONE',  ( 3.421838780265678004, -26.52253300979309003, 7.720710062488887360 ) ) ;
#18622 = CARTESIAN_POINT ( 'NONE',  ( 33.45661454515796862, -3.832864999374546944, -5.089924726100075958 ) ) ;
#18623 = CARTESIAN_POINT ( 'NONE',  ( 3.723586923686467376, -32.30245183660008479, 6.929923840112067523 ) ) ;
#18624 = CARTESIAN_POINT ( 'NONE',  ( 14.67649090451648597, 13.02133489615250106, 2.497019376560389414 ) ) ;
#18625 = LINE ( 'NONE', #25035, #18123 ) ;
#18626 = CARTESIAN_POINT ( 'NONE',  ( 29.78968071384544203, -3.771415970051185784, 4.475279941939479755 ) ) ;
#18627 = EDGE_CURVE ( 'NONE', #18363, #23072, #12232, .T. ) ;
#18628 = ADVANCED_FACE ( 'NONE', ( #36637 ), #31981, .T. ) ;
#18629 = DIRECTION ( 'NONE',  ( 0.000000000000000000, 0.000000000000000000, 1.000000000000000000 ) ) ;
#18630 = EDGE_CURVE ( 'NONE', #35146, #16635, #17886, .T. ) ;
#18631 = AXIS2_PLACEMENT_3D ( 'NONE', #24364, #5431, #8706 ) ;
#18632 = CARTESIAN_POINT ( 'NONE',  ( 17.33476859172393603, 14.29741483272972147, -2.500000000000000000 ) ) ;
#18633 = AXIS2_PLACEMENT_3D ( 'NONE', #29182, #13925, #10434 ) ;
#18634 = CARTESIAN_POINT ( 'NONE',  ( 25.95728207872785731, 0.9011556877583806191, -4.428986979826762038 ) ) ;
#18635 = CYLINDRICAL_SURFACE ( 'NONE', #22100, 6.000000000000005329 ) ;
#18636 = CARTESIAN_POINT ( 'NONE',  ( 24.54108476865473776, 2.742666202680888343, -3.872715312010981847 ) ) ;
#18637 = VERTEX_POINT ( 'NONE', #36840 ) ;
#18638 = CARTESIAN_POINT ( 'NONE',  ( 67.13068300324758297, 58.11650739856835202, 3.998197261021420701 ) ) ;
#18639 = CARTESIAN_POINT ( 'NONE',  ( 37.07071770796867582, -2.906269623872106855, 5.992180075661026173 ) ) ;
#18640 = LINE ( 'NONE', #21342, #12558 ) ;
#18641 = VECTOR ( 'NONE', #39885, 1000.000000000000000 ) ;
#18642 = DIRECTION ( 'NONE',  ( 1.000000000000000000, 0.000000000000000000, 0.000000000000000000 ) ) ;
#18643 = CARTESIAN_POINT ( 'NONE',  ( 88.47081344899795852, -1.206222823704210301, -3.524641158899461058 ) ) ;
#18644 = EDGE_CURVE ( 'NONE', #14367, #24859, #8823, .T. ) ;
#18646 = CARTESIAN_POINT ( 'NONE',  ( -38.44874870218063734, -25.49307895267003587, 6.700000000000000178 ) ) ;
#18645 = DIRECTION ( 'NONE',  ( 0.000000000000000000, 0.000000000000000000, 1.000000000000000000 ) ) ;
#18647 = ORIENTED_EDGE ( 'NONE', *, *, #14039, .F. ) ;
#18648 = CARTESIAN_POINT ( 'NONE',  ( 24.61222844760713002, 2.982919474122702308, 3.547505255288157855 ) ) ;
#18649 = LINE ( 'NONE', #9186, #27225 ) ;
#18650 = ORIENTED_EDGE ( 'NONE', *, *, #34789, .F. ) ;
#18651 = CARTESIAN_POINT ( 'NONE',  ( -69.93541594206888590, -20.90143516061696616, 5.929309462487109883 ) ) ;
#18652 = ORIENTED_EDGE ( 'NONE', *, *, #16773, .F. ) ;
#18653 = CARTESIAN_POINT ( 'NONE',  ( 80.78018476400323777, 61.88220158024270035, -2.864416008774563593 ) ) ;
#18654 = CARTESIAN_POINT ( 'NONE',  ( -1.697427395360086244, -29.44812577374269580, 7.754798119455333705 ) ) ;
#18655 = B_SPLINE_CURVE_WITH_KNOTS ( 'NONE', 3,
 ( #30337, #33846, #2764, #8898 ),
 .UNSPECIFIED., .F., .F.,
 ( 4, 4 ),
 ( 0.000000000000000000, 6.391136169994862974E-06 ),
 .UNSPECIFIED. ) ;
#18656 = CARTESIAN_POINT ( 'NONE',  ( 78.99045122244679362, 65.44959329978490814, 2.843122152733565056 ) ) ;
#18658 = VERTEX_POINT ( 'NONE', #22025 ) ;
#18657 = CARTESIAN_POINT ( 'NONE',  ( -28.97867591359219475, -26.64985754041175525, 6.700000000000000178 ) ) ;
#18659 = EDGE_CURVE ( 'NONE', #33117, #12043, #21446, .T. ) ;
#18660 = AXIS2_PLACEMENT_3D ( 'NONE', #28786, #10234, #7549 ) ;
#18661 = VECTOR ( 'NONE', #26178, 1000.000000000000000 ) ;
#18662 = CARTESIAN_POINT ( 'NONE',  ( -1.784512137809761700, -29.51577928193536593, 7.785387725071483800 ) ) ;
#18664 = CYLINDRICAL_SURFACE ( 'NONE', #17663, 0.1000000000000028644 ) ;
#18663 = CARTESIAN_POINT ( 'NONE',  ( 4.919623465605695856, -30.94344769399372908, 6.931070083220548739 ) ) ;
#18665 = CARTESIAN_POINT ( 'NONE',  ( 0.9053063435450576790, -25.37262878166647084, 7.695279973900954751 ) ) ;
#18666 = CARTESIAN_POINT ( 'NONE',  ( 33.89631951754260797, -5.457875755526142569, -0.7132651481052724174 ) ) ;
#18667 = CARTESIAN_POINT ( 'NONE',  ( 24.01772313286779337, 3.314519433455826558, -3.335196132849951312 ) ) ;
#18668 = ORIENTED_EDGE ( 'NONE', *, *, #22195, .T. ) ;
#18669 = CYLINDRICAL_SURFACE ( 'NONE', #12348, 0.09010775117053039518 ) ;
#18670 = EDGE_CURVE ( 'NONE', #24849, #19674, #23386, .T. ) ;
#18671 = VECTOR ( 'NONE', #18138, 1000.000000000000000 ) ;
#18672 = CARTESIAN_POINT ( 'NONE',  ( 24.14839210154553584, 1.598524049810922998, 6.350534879451781300 ) ) ;
#18673 = EDGE_CURVE ( 'NONE', #38156, #15393, #6710, .T. ) ;
#18674 = CARTESIAN_POINT ( 'NONE',  ( -77.76488672280875392, -5.012270680665758427, -8.924360589981601422 ) ) ;
#18675 = AXIS2_PLACEMENT_3D ( 'NONE', #8218, #5358, #21209 ) ;
#18676 = FACE_OUTER_BOUND ( 'NONE', #31610, .T. ) ;
#18677 = CARTESIAN_POINT ( 'NONE',  ( 79.92917477698721029, 65.49944209122678274, 2.989933650883223493 ) ) ;
#18678 = B_SPLINE_CURVE_WITH_KNOTS ( 'NONE', 3,
 ( #23823, #33733, #21167, #30645 ),
 .UNSPECIFIED., .F., .F.,
 ( 4, 4 ),
 ( 0.000000000000000000, 6.391136169994469103E-06 ),
 .UNSPECIFIED. ) ;
#18679 = CARTESIAN_POINT ( 'NONE',  ( 87.89980060869044109, -1.794189136469996004, 3.743635721206352684 ) ) ;
#18680 = LINE ( 'NONE', #15810, #23349 ) ;
#18681 = ORIENTED_EDGE ( 'NONE', *, *, #17451, .T. ) ;
#18682 = CARTESIAN_POINT ( 'NONE',  ( 2.913833110970087681, -32.85284901314008010, 7.750000000000001776 ) ) ;
#18683 = CARTESIAN_POINT ( 'NONE',  ( 14.77500326541903952, -5.175625724643098557, -2.499997102511863911 ) ) ;
#18684 = EDGE_CURVE ( 'NONE', #11044, #2129, #26697, .T. ) ;
#18685 = CARTESIAN_POINT ( 'NONE',  ( 4.066175018403209940, -26.99056084707641290, 6.880828092187096345 ) ) ;
#18686 = DIRECTION ( 'NONE',  ( 1.000000000000000000, 0.000000000000000000, 0.000000000000000000 ) ) ;
#18687 = CARTESIAN_POINT ( 'NONE',  ( 4.792526203416204389, -27.93020634197934982, 7.750000000000000888 ) ) ;
#18688 = CARTESIAN_POINT ( 'NONE',  ( 86.00054146471580907, 0.2529338399765344580, 5.999804812770356932 ) ) ;
#18689 = CARTESIAN_POINT ( 'NONE',  ( 1.910276347359660898, -26.17641463748400810, 6.959317978105163505 ) ) ;
#18690 = ORIENTED_EDGE ( 'NONE', *, *, #14563, .F. ) ;
#18691 = CARTESIAN_POINT ( 'NONE',  ( 32.77907637591459888, -0.9333423657278323571, 5.322365652056097574 ) ) ;
#18692 = AXIS2_PLACEMENT_3D ( 'NONE', #8664, #23905, #30930 ) ;
#18693 = AXIS2_PLACEMENT_3D ( 'NONE', #9771, #37966, #31202 ) ;
#18694 = DIRECTION ( 'NONE',  ( 1.000000000000000000, 0.000000000000000000, 0.000000000000000000 ) ) ;
#18695 = VERTEX_POINT ( 'NONE', #19127 ) ;
#18697 = CARTESIAN_POINT ( 'NONE',  ( 20.92112565569648552, 4.582337785983522593, 2.646877878247182903 ) ) ;
#18696 = CARTESIAN_POINT ( 'NONE',  ( 81.31277617166799132, 62.04138461958081763, -2.639511535887550053 ) ) ;
#18698 = APPLICATION_CONTEXT ( 'automotive_design' ) ;
#18699 = CARTESIAN_POINT ( 'NONE',  ( 18.14764728852392750, -2.851772390853231531, 3.038777280519134649 ) ) ;
#18700 = DIRECTION ( 'NONE',  ( -0.000000000000000000, -0.000000000000000000, -1.000000000000000000 ) ) ;
#18701 = CARTESIAN_POINT ( 'NONE',  ( 5.928245814084836418, -30.19173177851781276, 7.754798119455333705 ) ) ;
#18702 = EDGE_LOOP ( 'NONE', ( #37786, #25820, #20557, #13265 ) ) ;
#18703 = CARTESIAN_POINT ( 'NONE',  ( 27.06227200975126124, -4.553918775559605336, -3.575370272941529315 ) ) ;
#18704 = VECTOR ( 'NONE', #32389, 1000.000000000000000 ) ;
#18705 = ORIENTED_EDGE ( 'NONE', *, *, #28783, .F. ) ;
#18706 = ORIENTED_EDGE ( 'NONE', *, *, #4988, .T. ) ;
#18707 = CARTESIAN_POINT ( 'NONE',  ( 80.35739993109717716, 63.53218113005920742, -3.674973878998262222 ) ) ;
#18708 = CARTESIAN_POINT ( 'NONE',  ( -71.19001092293638067, 0.1909006763965998277, 5.995522264747400243 ) ) ;
#18709 = ORIENTED_EDGE ( 'NONE', *, *, #17840, .F. ) ;
#18711 = CARTESIAN_POINT ( 'NONE',  ( 35.58747779558025570, -1.229805145029287727, 5.504146291393874790 ) ) ;
#18710 = CARTESIAN_POINT ( 'NONE',  ( 24.26828315858369933, 2.497494390861238145, 4.073910292191768256 ) ) ;
#18712 = ORIENTED_EDGE ( 'NONE', *, *, #3078, .T. ) ;
#18713 = CARTESIAN_POINT ( 'NONE',  ( 81.56984355495252714, 61.60674381500905383, -1.524764441711166763 ) ) ;
#18714 = CARTESIAN_POINT ( 'NONE',  ( 6.029042948269167645, -32.11059846819836139, 7.695279973900954751 ) ) ;
#18715 = ADVANCED_FACE ( 'NONE', ( #3713 ), #31694, .F. ) ;
#18716 = CARTESIAN_POINT ( 'NONE',  ( -0.9786759135921931918, -24.55319635012989110, 6.700000000000000178 ) ) ;
#18718 = CARTESIAN_POINT ( 'NONE',  ( -10.97867591359219475, -26.64985754041175525, 6.700000000000000178 ) ) ;
#18717 = DIRECTION ( 'NONE',  ( 0.000000000000000000, 0.000000000000000000, 1.000000000000000000 ) ) ;
#18719 = CARTESIAN_POINT ( 'NONE',  ( 0.8302441911734864677, -26.17279668076718835, 7.501983001166816933 ) ) ;
#18720 = CARTESIAN_POINT ( 'NONE',  ( -64.08758708074093136, 41.34482390022287035, -2.999999996405878111 ) ) ;
#18721 = CARTESIAN_POINT ( 'NONE',  ( 73.64144479846403613, 59.51803038729781292, 3.736020861036525531 ) ) ;
#18722 = CARTESIAN_POINT ( 'NONE',  ( 23.93748849625432129, 2.937348812402350795, -3.838641491431229902 ) ) ;
#18723 = EDGE_LOOP ( 'NONE', ( #603, #29706, #30631, #8479, #2689, #22870 ) ) ;
#18724 = EDGE_CURVE ( 'NONE', #36751, #16025, #25367, .T. ) ;
#18725 = AXIS2_PLACEMENT_3D ( 'NONE', #18579, #40403, #19209 ) ;
#18726 = CARTESIAN_POINT ( 'NONE',  ( 21.85643539959774273, -9.053501261307662418, 13.64238141129353110 ) ) ;
#18727 = EDGE_CURVE ( 'NONE', #651, #38473, #799, .T. ) ;
#18728 = CARTESIAN_POINT ( 'NONE',  ( -58.94581694272203265, 28.88139188076748454, -6.382668916716455421 ) ) ;
#18729 = ORIENTED_EDGE ( 'NONE', *, *, #30165, .T. ) ;
#18730 = CARTESIAN_POINT ( 'NONE',  ( 3.939786388318850641, -26.88011527646091992, 7.635761828346575797 ) ) ;
#18731 = CARTESIAN_POINT ( 'NONE',  ( 81.81391746733756065, 63.52311930392516359, 2.869341960395463520 ) ) ;
#18732 = VECTOR ( 'NONE', #4041, 1000.000000000000000 ) ;
#18733 = CARTESIAN_POINT ( 'NONE',  ( 88.50738123939095203, -1.057966825106399389, -0.8062500484416172952 ) ) ;
#18734 = VERTEX_POINT ( 'NONE', #9237 ) ;
#18735 = EDGE_CURVE ( 'NONE', #561, #16288, #38615, .T. ) ;
#18736 = CIRCLE ( 'NONE', #31897, 6.406751979251626317 ) ;
#18737 = CARTESIAN_POINT ( 'NONE',  ( 0.5502190760550982329, -32.76947806258566231, 7.635761828346577573 ) ) ;
#18738 = CARTESIAN_POINT ( 'NONE',  ( 16.23297496238618720, -3.365206226087963159, 2.739004174318827367 ) ) ;
#18739 = CARTESIAN_POINT ( 'NONE',  ( 1.073548286649947725, -26.12652063041838346, 7.643192810543820492 ) ) ;
#18740 = EDGE_CURVE ( 'NONE', #2378, #11346, #8934, .T. ) ;
#18741 = CARTESIAN_POINT ( 'NONE',  ( 35.87004182851519829, -2.084339523132501704, -5.804785566216419390 ) ) ;
#18742 = CARTESIAN_POINT ( 'NONE',  ( 5.098207581826219581, -29.69173459304409946, 7.754798119455333705 ) ) ;
#18743 = CARTESIAN_POINT ( 'NONE',  ( 21.89858067459283575, 5.089326824990051179, 3.617611013575467105 ) ) ;
#18744 =( BOUNDED_CURVE ( )  B_SPLINE_CURVE ( 3, ( #37210, #31870, #40294, #34571 ),
 .UNSPECIFIED., .F., .F. ) 
 B_SPLINE_CURVE_WITH_KNOTS ( ( 4, 4 ),
 ( 4.748221474220558846, 4.941946782021394036 ),
 .UNSPECIFIED. ) 
 CURVE ( )  GEOMETRIC_REPRESENTATION_ITEM ( )  RATIONAL_B_SPLINE_CURVE ( ( 1.000000000000000000, 0.9968749865767494445, 0.9968749865767494445, 1.000000000000000000 ) ) 
 REPRESENTATION_ITEM ( '' )  );
#18745 = DIRECTION ( 'NONE',  ( 0.000000000000000000, 0.000000000000000000, 1.000000000000000000 ) ) ;
#18746 = DIRECTION ( 'NONE',  ( 0.3757233601570964532, 0.9267318687906771491, -0.000000000000000000 ) ) ;
#18747 = EDGE_LOOP ( 'NONE', ( #13942, #30953, #6799, #18268 ) ) ;
#18748 = EDGE_LOOP ( 'NONE', ( #6372, #29253, #12428, #12155 ) ) ;
#18749 = CARTESIAN_POINT ( 'NONE',  ( 35.36800336353066143, -3.790791895310993365, 5.512052037117470604 ) ) ;
#18750 = CYLINDRICAL_SURFACE ( 'NONE', #29078, 0.09010775117052798044 ) ;
#18751 = CARTESIAN_POINT ( 'NONE',  ( 66.69989039061726999, 57.93340768760646142, -3.999416444362182688 ) ) ;
#18752 = CARTESIAN_POINT ( 'NONE',  ( 86.50956153430306017, -0.6400250991913265519, -5.705005027417270114 ) ) ;
#18753 = CIRCLE ( 'NONE', #26645, 1.000000000000000000 ) ;
#18754 = ORIENTED_EDGE ( 'NONE', *, *, #4346, .F. ) ;
#18755 = VECTOR ( 'NONE', #31244, 1000.000000000000000 ) ;
#18756 = CARTESIAN_POINT ( 'NONE',  ( -56.64002613362055882, 29.83241628681511770, 1.779850828381770445 ) ) ;
#18757 = CARTESIAN_POINT ( 'NONE',  ( -80.57566330002634913, -6.630847404920713117, -2.665206594670471940 ) ) ;
#18758 = CARTESIAN_POINT ( 'NONE',  ( 4.960212797054523115, -28.60371536055546926, 6.979335674598003969 ) ) ;
#18759 = CARTESIAN_POINT ( 'NONE',  ( -0.8532251611581016526, -27.17638696620667105, 6.951256099901587326 ) ) ;
#18760 = FACE_BOUND ( 'NONE', #25429, .T. ) ;
#18761 = LINE ( 'NONE', #40175, #38951 ) ;
#18762 = ORIENTED_EDGE ( 'NONE', *, *, #39866, .F. ) ;
#18763 = CARTESIAN_POINT ( 'NONE',  ( 23.14338651803718250, 4.000357944295927837, 3.156986160450860446 ) ) ;
#18764 = VECTOR ( 'NONE', #20713, 1000.000000000000000 ) ;
#18765 = CARTESIAN_POINT ( 'NONE',  ( 81.95295003160654801, 61.95651309483395153, -1.189854999565593818 ) ) ;
#18766 = CARTESIAN_POINT ( 'NONE',  ( 79.29422675899259332, 65.38839789421687954, 2.978180346930987099 ) ) ;
#18767 = CARTESIAN_POINT ( 'NONE',  ( -1.749422520758312505, -28.97934324792513294, 7.750000000000000000 ) ) ;
#18768 = VERTEX_POINT ( 'NONE', #11425 ) ;
#18769 = CARTESIAN_POINT ( 'NONE',  ( 75.68803578311077729, 63.95394130778559116, -2.805892758485396765 ) ) ;
#18771 = CARTESIAN_POINT ( 'NONE',  ( -26.24874870218063450, -26.64985754041175525, 6.700000000000000178 ) ) ;
#18770 = CARTESIAN_POINT ( 'NONE',  ( -71.12603986806550438, -45.62685002856374439, 5.997522800198533233 ) ) ;
#18772 = CARTESIAN_POINT ( 'NONE',  ( 14.98826240343326965, 12.12410137783581199, -2.538583708695383745 ) ) ;
#18773 = CARTESIAN_POINT ( 'NONE',  ( 81.20101650719858810, 62.86240828450102924, -3.233552917234641555 ) ) ;
#18774 = CARTESIAN_POINT ( 'NONE',  ( 78.95923394621949853, 61.57577394195569553, 3.401348408886338159 ) ) ;
#18775 = ORIENTED_EDGE ( 'NONE', *, *, #38118, .F. ) ;
#18776 = DIRECTION ( 'NONE',  ( -0.9949204587440765302, -0.1006641980670203163, 0.000000000000000000 ) ) ;
#18777 = FACE_OUTER_BOUND ( 'NONE', #2205, .T. ) ;
#18778 = CARTESIAN_POINT ( 'NONE',  ( 82.29984285855105952, 63.07754316838597219, 2.094266784918906943 ) ) ;
#18780 = CARTESIAN_POINT ( 'NONE',  ( -1.693494594903330652, -29.36608178104888722, 6.920489980334477487 ) ) ;
#18779 = CARTESIAN_POINT ( 'NONE',  ( 4.254702208415469755, -31.96273153170552916, 6.971170733404099984 ) ) ;
#18781 = CARTESIAN_POINT ( 'NONE',  ( 31.64923038865762805, -3.528005414130610529, -5.019302312848182623 ) ) ;
#18782 = CARTESIAN_POINT ( 'NONE',  ( -1.420400527842048843, -31.15443827722234360, 6.980586498568969844 ) ) ;
#18783 = DIRECTION ( 'NONE',  ( 0.000000000000000000, 1.000000000000000000, 0.000000000000000000 ) ) ;
#18784 = CARTESIAN_POINT ( 'NONE',  ( 1.519733255401420458, -33.06526953655340861, 6.998987538705437217 ) ) ;
#18785 = CARTESIAN_POINT ( 'NONE',  ( 22.30416999533203892, 0.2663055805526909903, -7.088243610313228693 ) ) ;
#18786 = EDGE_CURVE ( 'NONE', #12131, #20345, #11021, .T. ) ;
#18787 = LINE ( 'NONE', #31365, #39256 ) ;
#18788 = AXIS2_PLACEMENT_3D ( 'NONE', #26305, #38838, #32687 ) ;
#18789 = CARTESIAN_POINT ( 'NONE',  ( -0.6412820820920860365, -32.03500197365509194, 6.939395833800439561 ) ) ;
#18790 = AXIS2_PLACEMENT_3D ( 'NONE', #4686, #4101, #4298 ) ;
#18791 = CARTESIAN_POINT ( 'NONE',  ( -0.03065438358791758300, -26.64358689880297248, 7.695279973900954751 ) ) ;
#18792 = EDGE_CURVE ( 'NONE', #28485, #15211, #8549, .T. ) ;
#18793 = CARTESIAN_POINT ( 'NONE',  ( -67.83000114521873058, 27.33924089054923101, 15.50000000000000000 ) ) ;
#18794 = CARTESIAN_POINT ( 'NONE',  ( 37.19502771478310166, -2.749426064116375468, -6.000945458054299131 ) ) ;
#18795 = CARTESIAN_POINT ( 'NONE',  ( -38.24874870218063450, -26.64985754041175525, 6.700000000000000178 ) ) ;
#18796 = CARTESIAN_POINT ( 'NONE',  ( -56.02725819615764635, 27.69325783080268266, -46.17089178453873188 ) ) ;
#18797 = CARTESIAN_POINT ( 'NONE',  ( 0.4893092558450570229, -32.84442375634601063, 7.778495531946294506 ) ) ;
#18798 = PLANE ( 'NONE',  #33204 ) ;
#18799 = CARTESIAN_POINT ( 'NONE',  ( 2.128010023882844326, -32.94294212574573777, 6.876076431790006716 ) ) ;
#18800 = AXIS2_PLACEMENT_3D ( 'NONE', #29278, #16306, #32183 ) ;
#18801 = DIRECTION ( 'NONE',  ( 0.000000000000000000, 0.000000000000000000, 1.000000000000000000 ) ) ;
#18802 = DIRECTION ( 'NONE',  ( -0.000000000000000000, -0.000000000000000000, 1.000000000000000000 ) ) ;
#18803 = VERTEX_POINT ( 'NONE', #24412 ) ;
#18804 = SURFACE_STYLE_FILL_AREA ( #15311 ) ;
#18805 = CARTESIAN_POINT ( 'NONE',  ( 68.17490759376208587, 57.99096015551094041, -3.964697573200900660 ) ) ;
#18806 = CARTESIAN_POINT ( 'NONE',  ( 2.933026231274471485, -26.29416234278157916, 6.887161170156907986 ) ) ;
#18807 = EDGE_LOOP ( 'NONE', ( #10853, #6653, #19114, #23419 ) ) ;
#18808 = CYLINDRICAL_SURFACE ( 'NONE', #23267, 0.09010775117052854943 ) ;
#18809 = CARTESIAN_POINT ( 'NONE',  ( 0.09112544421487976665, -26.57487120552241322, 6.864651958020304257 ) ) ;
#18810 = CARTESIAN_POINT ( 'NONE',  ( 5.038904606479174042, -28.51902327498534362, 6.880828092187097234 ) ) ;
#18811 = B_SPLINE_SURFACE_WITH_KNOTS ( 'NONE', 3, 3, ( 
 ( #10951, #36099, #16530, #29107, #22937, #17940, #8880, #39565, #24330, #5608, #34037, #40179, #24121, #15268, #30521, #27819, #17729, #15064, #11959, #12176, #8673, #36287, #21462, #27215, #24536 ),
 ( #39776, #5810, #2745, #2331, #14852, #11550, #8063, #37091, #18349, #36689, #11753, #14448, #18146, #30939, #30735, #20623, #8469, #27622, #11348, #5197, #23913, #2539, #27418, #40371, #33209 ),
 ( #1925, #30315, #4995, #17520, #30116, #27019, #2126, #21254, #36489, #8261, #20832, #33428, #14643, #21053, #33625, #5400, #36895, #39981, #33825, #25363, #6633, #3558, #31744, #31135, #24955 ),
 ( #3164, #16085, #24746, #18765, #22286, #37491, #28031, #28652, #28855, #37295, #31956, #9089, #19180, #34442, #663, #459, #37900, #9286, #38106, #56, #12586, #15882, #6828, #25152, #9492 ),
 ( #21665, #3760, #34243, #12997, #6219, #6015, #25562, #9707, #21865, #9910, #37687, #22079, #28441, #19385, #34653, #22490, #18551, #2953, #6424, #18981, #28229, #35054, #15470, #15681, #31544 ),
 ( #40577, #12387, #12787, #16285, #31339, #3367, #249, #34856, #36049, #7629, #32560, #29655, #23087, #10102, #38505, #39108, #23281, #866, #19787, #23482, #1073, #26571, #7421, #22884, #13810 ),
 ( #19979, #32957, #35454, #32764, #1466, #29857, #26378, #13200, #10906, #4156, #14000, #17078, #4553, #25971, #7826, #13604, #35848, #22688, #10307, #20375, #7226, #35651, #20181, #38910, #10505 ),
 ( #4743, #25769, #16674, #17276, #16485, #32361, #13398, #38305, #4359, #35255, #7023, #29258, #19591, #32167, #26176, #3966, #29058, #38709, #16880, #29460, #10702, #1271, #4945, #15016, #24488 ),
 ( #14803, #26971, #2083, #11102, #27579, #33380, #39933, #8627, #40132, #21413, #36240, #17892, #17474, #20786, #21206, #1668, #36439, #11708, #1877, #30065, #11912, #14401, #18302, #36643, #26775 ),
 ( #5761, #14202, #8828, #39313, #36844, #11298, #23674, #18094, #2279, #39517, #37044, #17684, #30265, #33577, #33989, #14596, #33778, #8019, #20572, #27167, #24071, #5149, #33159, #23863, #39724 ),
 ( #11505, #8422, #8212, #20998, #2494, #5355, #30473, #30687, #27371, #24285, #5556, #6782, #37444, #25321, #22029, #9242, #12336, #34401, #12540, #3516, #34196, #18930, #12741, #28604, #34810 ),
 ( #25112, #9865, #24910, #9658, #6586, #30890, #3320, #2702, #16038, #6172, #19132, #31699, #412, #2901, #12953, #31295, #37852, #40327, #27980, #25516, #15420, #34603, #38062, #28396, #28183 ),
 ( #22437, #15220, #18713, #35007, #5962, #40528, #18507, #27774, #31496, #12120, #24697, #3118, #37248, #9039, #15634, #21617, #31091, #13347, #11204, #25921, #27078, #31906, #10258, #39623, #22839 ),
 ( #19739, #13554, #8731, #17792, #34305, #40037, #5873, #15326, #21722, #28091, #2182, #24596, #11609, #27487, #18411, #31194, #30999, #20895, #11810, #27881, #24188, #18001, #36744, #2802, #27679 ),
 ( #36952, #30587, #30796, #40642, #37150, #40426, #40235, #14700, #27269, #8529, #39840, #2394, #21315, #3014, #15534, #6074, #21523, #33680, #33887, #30378, #18607, #24393, #12237, #24811, #12445 ),
 ( #21112, #5460, #5667, #8939, #25012, #14919, #8321, #2604, #33481, #18204, #37352, #15123, #12019, #5252, #34098, #9146, #37750, #37551, #34501, #19239, #3225, #13255, #19647, #32218, #34712 ),
 ( #3823, #9346, #21927, #9766, #31805, #313, #10157, #15741, #28501, #34916, #22547, #12850, #3620, #31396, #19040, #38360, #6275, #28710, #25824, #18824, #28293, #6691, #13456, #3425, #32016 ),
 ( #31602, #15936, #16147, #22746, #114, #25617, #6887, #35313, #717, #25419, #16538, #522, #29115, #37959, #16340, #7081, #12646, #9966, #25220, #4020, #22346, #921, #9555, #28911, #22139 ),
 ( #13055, #38160, #35109, #6488, #19441, #23729, #1329, #1521, #4210, #26629, #39368, #26237, #1935, #20235, #10370, #10756, #20433, #35905, #1133, #11158, #23336, #38769, #10565, #26028, #22946 ),
 ( #36295, #13866, #26434, #17138, #8072, #38961, #33014, #38560, #35508, #32818, #4607, #29518, #20631, #32415, #16940, #29711, #10959, #14054, #39163, #19844, #7482, #26827, #7280, #23542, #1725 ),
 ( #4801, #36107, #14256, #7883, #16730, #23139, #33218, #17332, #13665, #32620, #5003, #29910, #17529, #30123, #35706, #29316, #20039, #4416, #8477, #27223, #8888, #31144, #27828, #33834, #11760 ),
 ( #2133, #15277, #5408, #17947, #40380, #21676, #36903, #21262, #30530, #14456, #18360, #12185, #2339, #30746, #33435, #24544, #37303, #37101, #27027, #14861, #34047, #17736, #24132, #14651, #21470 ),
 ( #27430, #39989, #36696, #8680, #34252, #2547, #5821, #5615, #20841, #5205, #39788, #30325, #21060, #24339, #9099, #6025, #24755, #27630, #11558, #18155, #23924, #18559, #15073, #11968, #30948 ),
 ( #33632, #40187, #2753, #39572, #11356, #36498, #8269, #21874, #25371, #6641, #38115, #28662, #22087, #19393, #3375, #6836, #15689, #3567, #468, #3768, #9715, #2962, #9918, #37696, #13008 ),
 ( #31347, #22499, #34661, #19188, #12397, #28240, #25571, #65, #15891, #31754, #22294, #31552, #258, #12596, #25161, #28451, #12798, #35062, #31966, #15478, #37909, #37501, #16096, #6434, #18991 ),
 ( #34451, #9504, #24965, #28040, #6228, #40588, #34865, #9296, #18773, #3175, #12317, #21803, #2883, #11490, #24893, #11688, #40312, #21395, #33970, #12101, #21601, #18485, #5947, #5336, #39914 ),
 ( #18080, #31075, #39703, #33759, #37228, #24266, #2261, #15404, #3098, #24053, #6156, #36622, #34182, #8610, #15614, #27964, #24679, #36828, #37429, #15000, #27560, #30876, #34381, #40117, #40507 ),
 ( #5743, #33560, #27355, #9022, #9224, #18696, #8408, #31278, #20981, #17870, #30454, #27758, #14786, #21188, #5539, #18285, #30668, #2477, #11895, #2682, #24468, #8809, #37025, #15205, #13328 ),
 ( #16022, #797, #22421, #37837, #28797, #3910, #19317, #22222, #189, #22625, #4096, #25904, #6766, #25498, #13142, #6363, #15825, #28995, #19115, #31682, #38441, #35394, #9847, #34991, #3499 ),
 ( #12726, #31891, #10044, #25700, #38046, #3702, #9640, #34792, #16223, #38243, #16423, #10245, #28167, #12936, #9424, #35193, #28589, #398, #6569, #6965, #7165, #19524, #32105, #22824, #34588 ),
 ( #19726, #32298, #31480, #24854, #12522, #25096, #37625, #18912, #25302, #3304, #28379, #10839, #17214, #39242, #36176, #23610, #23023, #16816, #19918, #20114, #29785, #29990, #29395, #33302, #23415 ),
 ( #20717, #29193, #23799, #16609, #11032, #26311, #1005, #33088, #1600, #1213, #1805, #32693, #4493, #7760, #39444, #17013, #7956, #13540, #26113, #29590, #39038, #1405, #14330, #35589, #7559 ),
 ( #38644, #10442, #7360, #4680, #26901, #13748, #20504, #35979, #38846, #11234, #4873, #20308, #17408, #26508, #32489, #10640, #36374, #26708, #4289, #23217, #8145, #32893, #35781, #14131, #13938 ),
 ( #21408, #12330, #11499, #21610, #31084, #12111, #20778, #34191, #20992, #8822, #30679, #2489, #33981, #30884, #27768, #15214, #14589, #8417, #24064, #11701, #5756, #5956, #33569, #24903, #15010 ),
 ( #40321, #8204, #33372, #15413, #5142, #2696, #17884, #17676, #24691, #18295, #5348, #18501, #24279, #36839, #40126, #2895, #8619, #37240, #30258, #2077, #21199, #27573, #33773, #27972, #27161 ),
 ( #9033, #39716, #36636, #30466, #37036, #40520, #2273, #14795, #11906, #27365, #39927, #5550, #24481, #18089, #6580, #34395, #22024, #22636, #6777, #25106, #3314, #6975, #25315, #10054, #31693 ),
 ( #37846, #16431, #3508, #29005, #18922, #16236, #13151, #13342, #9857, #37437, #35203, #28389, #25711, #609, #28807, #9439, #19534, #9650, #19330, #6166, #34598, #38257, #6373, #19126, #31901 ),
 ( #3711, #32116, #3919, #9235, #198, #808, #2, #31490, #37635, #21813, #16032, #18707, #31288, #15834, #3106, #15628, #12736, #12946, #28177, #12533, #22235, #34801, #28599, #409, #25511 ),
 ( #38057, #22433, #35003, #17416, #39252, #38655, #20515, #32309, #7369, #22832, #20320, #19735, #17224, #19926, #39050, #30001, #29205, #11046, #7965, #29797, #38450, #23621, #10452, #26517, #7571 ),
 ( #23424, #32902, #36185, #4885, #4106, #1415, #1017, #4304, #4691, #25916, #32502, #35990, #26123, #13549, #1610, #1817, #10253, #33100, #35403, #14145, #35599, #7176, #26718, #10849, #23034 ),
 ( #16620, #16826, #29408, #29600, #7772, #1224, #13758, #32706, #26322, #38859, #10650, #23229, #35795, #20126, #4503, #17025, #13951, #11243, #2440, #27721, #14538, #8771, #8572, #36588, #37192 ),
 ( #30836, #24226, #23807, #39662, #40276, #24433, #2022, #20937, #24641, #2221, #12060, #21150, #24011, #14960, #2646, #5496, #8363, #27112, #21357, #31040, #8982, #33717, #11649, #40079, #33312 ),
 ( #18246, #5706, #11445, #21567, #14742, #36989, #36383, #33523, #15163, #5292, #8155, #20727, #27527, #34146, #17831, #33932, #18039, #30414, #5914, #18454, #30632, #14339, #36787, #5091, #27313 ),
 ( #39874, #11857, #26911, #17625, #39455, #30203, #565, #6731, #31444, #22587, #37797, #35154, #25059, #22389, #19281, #19489, #15982, #2847, #16189, #34550, #31848, #3662, #34954, #15580, #13103 ),
 ( #9603, #6324, #15367, #28755, #25662, #18871, #19080, #21766, #12897, #38204, #25462, #27924, #3266, #10004, #6119, #12492, #31242, #38007, #22185, #6926, #40470, #28134, #12279, #9191, #37593 ),
 ( #37397, #24853, #9390, #28549, #34349, #18653, #3063, #40687, #21975, #15791, #28342, #156, #3464, #25265, #34757, #359, #9809, #12689, #6533, #31648, #32264, #35355, #35554, #32661, #4648 ),
 ( #29554, #4062, #7127, #23377, #36145, #3868, #39209, #32063, #26473, #966, #7925, #7727, #4459, #16577, #17181, #7322, #19881, #23178, #14094, #32453, #39001, #16384, #28958, #4253, #13711 ),
 ( #29750, #16982, #761, #1374, #13292, #35748, #26673, #16779, #10799, #25865, #38405, #29358, #26278, #1178, #1564, #10205, #22988, #38811, #13905, #10604, #7522, #22788, #13503, #32859, #19688 ),
 ( #26075, #10997, #35945, #20083, #20274, #23581, #29157, #38608, #10412, #30584, #8111, #27076, #30793, #8319, #33885, #14698, #30161, #21110, #36950, #11607, #14501, #33265, #14917, #37149, #5665 ),
 ( #20474, #18202, #11402, #8729, #24390, #11807, #5048, #2602, #20893, #2392, #29955, #17577, #21313, #1981, #2180, #27484, #33677, #17789, #39838, #39620, #23968, #27267, #30376, #15121, #27677 ),
 ( #40035, #24186, #12017, #40233, #36543, #24594, #26867, #33479, #17374, #33056, #14298, #4843, #5250, #5458, #1768, #23768, #39411, #11202, #36343, #20680, #36742, #8527, #17998, #31393, #3221 ),
 ( #28498, #15933, #15324, #9144, #12235, #12442, #9552, #22343, #21720, #25614, #15738, #34095, #34498, #3422, #18820, #24809, #34913, #6272, #34303, #6072, #8937, #5871, #28290, #27878, #25415 ),
 ( #18605, #3616, #40424, #31192, #18409, #310, #2800, #12847, #3012, #22133, #13051, #37350, #6687, #31802, #37956, #21521, #19235, #15531, #34708, #110, #12643, #6484, #31599, #9763, #16144 ),
 ( #25216, #28088, #40639, #28706, #30997, #25008, #19037, #37548, #9343, #519, #21924, #37747, #4604, #38157, #32617, #7078, #14051, #13863, #38766, #10154, #10754, #13452, #26025, #29313, #20232 ),
 ( #29515, #16535, #4207, #32012, #25821, #10561, #23333, #23136, #1518, #35703, #19437, #35106, #6884, #26232, #35902, #38358, #4412, #32412, #19644, #32816, #16937, #16727, #26431, #7277, #3820 ),
 ( #32215, #29112, #19841, #7682, #714, #7478, #20035, #17132, #1324, #38556, #29707, #1129, #9963, #4017, #38958, #22544, #16335, #28908, #13252, #22743, #918, #35308, #10366, #22943, #35505 ),
 ( #13662, #33432, #30120, #26626, #30527, #24336, #1930, #2130, #4797, #36693, #8677, #8474, #39160, #17524, #5405, #29907, #36292, #14252, #21057, #5202, #18151, #39986, #33009, #14453, #23919 ),
 ( #23539, #36104, #14648, #11757, #26824, #33629, #20837, #8067, #21259, #17944, #17733, #2336, #36495, #7880, #11155, #36899, #14856, #39365, #33215, #33831, #27023, #5612, #30321, #20628, #27220 ),
 ( #39782, #30740, #4999, #27425, #2544, #10955, #11555, #20430, #17329, #39569, #1721, #23725, #11353, #8266, #24128, #15474, #25157, #24540, #12181, #31548, #40376, #37495, #37692, #28235, #12392 ),
 ( #9498, #27626, #6020, #34657, #18356, #24750, #2749, #22083, #34446, #6637, #28446, #27823, #9711, #21466, #37299, #11964, #6429, #8884, #18986, #9096, #61, #19184, #30944, #254, #37905 ),
 ( #12794, #21670, #15684, #9292, #21870, #12590, #3371, #15887, #25366, #34042, #15272, #34248, #18555, #22290, #34861, #31139, #31750, #6224, #40183, #40581, #15070, #24961, #2958, #37097, #18769 ),
 ( #5815, #28036, #31343, #3170, #19983, #26918, #39461, #667, #7230, #13608, #35655, #22693, #10310, #38111, #31962, #4160, #38509, #28658, #29062, #38714, #13401, #19389, #16883, #869, #3764 ),
 ( #32566, #16677, #16290, #30008, #19596, #32170, #35458, #11249, #3969, #10510, #3562, #16092, #16488, #25976, #7028, #1827, #9914, #35259, #22889, #29263, #19791, #32364, #22495, #25772, #4363 ),
 ( #1076, #38309, #23814, #23090, #26180, #14348, #7425, #464, #28860, #36390, #8163, #13204, #10106, #20733, #13003, #25567, #35058, #6832, #27532, #30842, #30638, #30421, #20945, #21363, #5920 ),
 ( #40084, #33318, #40281, #39882, #2651, #15169, #27727, #33529, #24647, #24232, #8777, #2029, #17837, #12070, #5302, #5503, #33937, #24438, #33724, #2446, #2229, #14750, #18046, #14970, #37198 ),
 ( #8372, #5711, #11862, #5100, #8987, #27320, #21573, #11453, #11658, #14545, #18253, #39668, #34151, #36794, #36998, #17631, #8579, #30213, #27120, #24020, #21157, #36594, #1360, #29938, #10987 ),
 ( #26855, #36328, #1968, #8303, #22620, #4830, #32647, #7713, #8098, #28791, #23365, #39397, #35933, #11185, #29544, #4445, #20665, #33468, #597, #36529, #13138, #23758, #38988, #5236, #5034 ),
 ( #14486, #4636, #17166, #20461, #11387, #29735, #33250, #25696, #38239, #1550, #23567, #32847, #27059, #35735, #20261, #26660, #14286, #14081, #36131, #7508, #10787, #30150, #10040, #33040, #17564 ),
 ( #39605, #7912, #23952, #39194, #20071, #13895, #20879, #16971, #26459, #17361, #1755, #5650, #31178, #12001, #27465, #18394, #34288, #8920, #11791, #30567, #12220, #34482, #2999, #37132, #15104 ),
 ( #8715, #6057, #21707, #9133, #2377, #28072, #18187, #27864, #27254, #14896, #18592, #40020, #40219, #40414, #30980, #27663, #21504, #24373, #36933, #24581, #34083, #15517, #40625, #17773, #2583 ),
 ( #9328, #12430, #21294, #24998, #24172, #33868, #14686, #24793, #11591, #37533, #30779, #2786, #21907, #21092, #30360, #2165, #39823, #36728, #8512, #5857, #15312, #37338, #33663, #5440, #17980 ),
 ( #12627, #6471, #9537, #9748, #6869, #19626, #31378, #31785, #701, #16127, #22120, #32201, #3600, #19021, #31583, #6260, #3204, #28691, #25197, #22726, #29095, #897, #3408, #9945, #16319 ),
 ( #18805, #19221, #501, #22327, #4001, #37728, #37940, #13037, #31995, #34896, #25598, #95, #28483, #7059, #15723, #38143, #35291, #28276, #34693, #22527, #22920, #12830, #13237, #35093, #25402 ),
 ( #15920, #6670, #16519, #19423, #13433, #3799, #289, #28894, #26011, #25802, #38339, #10137, #38541, #10348, #8050, #14033, #32798, #20413, #13643, #23118, #36276, #26413, #38942, #20609, #1913 ),
 ( #10737, #35488, #39346, #33194, #23316, #10940, #26215, #4777, #17510, #17311, #7259, #35886, #14236, #38747, #4396, #35688, #29888, #26607, #27005, #4982, #7461, #30104, #1112, #16918, #32398 ),
 ( #10541, #20016, #32599, #29498, #1307, #7664, #14434, #39551, #11335, #7864, #13844, #20215, #4191, #19823, #4588, #32992, #1705, #16708, #29298, #17116, #23519, #29688, #1500, #26808, #39144 ),
 ( #36086, #11138, #23709, #18131, #33612, #24524, #40362, #15051, #17926, #36672, #18335, #40565, #37284, #2527, #21237, #8864, #2113, #11538, #24733, #14838, #27406, #9077, #31125, #5591, #30722 ),
 ( #12159, #8455, #27610, #5797, #37074, #40168, #11948, #5386, #30509, #21450, #34026, #21653, #6004, #23901, #8660, #5185, #30925, #24316, #11738, #2315, #2732, #2941, #15256, #27808, #18540 ),
 ( #39968, #15457, #28016, #27204, #36473, #8248, #20818, #33414, #30299, #21039, #14630, #39760, #24108, #12989, #35042, #31943, #19374, #18751, #12574, #15667, #15872, #25554, #25756, #25143, #29047 ),
 ( #28215, #3751, #16475, #24946, #19581, #12377, #6820, #22066, #37479, #28847, #38095, #37674, #38295, #28430, #237, #3548, #35243, #12777, #16274, #9277, #21853, #25348, #34842, #37889, #10096 ),
 ( #34429, #9897, #6208, #31329, #3151, #447, #22680, #9477, #654, #6619, #34640, #7015, #13190, #31734, #32157, #22275, #45, #6413, #3955, #22475, #18964, #31529, #3355, #9698, #19168 ),
 ( #16077, #28640, #35840, #10493, #1455, #17266, #32752, #35642, #13593, #36037, #17460, #14190, #20169, #38899, #26560, #19777, #29250, #1655, #32547, #4347, #26762, #8005, #23273, #7614, #16869 ) ),
 .UNSPECIFIED., .F., .F., .F.,
 ( 4, 3, 3, 3, 3, 3, 3, 3, 3, 3, 3, 3, 3, 3, 3, 3, 3, 3, 3, 3, 3, 3, 3, 3, 3, 3, 3, 4 ),
 ( 4, 3, 3, 3, 3, 3, 3, 3, 4 ),
 ( -2.249698332083740343E-17, 9.220626685372613810E-07, 1.844125337097019745E-06, 3.688250674216536686E-06, 5.532376011336053626E-06, 7.376501348455570566E-06, 1.106475202269460445E-05, 1.475300269693363833E-05, 2.212950404541170609E-05, 2.950600539388977385E-05, 4.425900809084590937E-05, 5.901201078780204490E-05, 8.851801618171431594E-05, 0.0001180240215756265870, 0.0001770360323634511291, 0.0002360480431512756712, 0.0003540720647269247554, 0.0004720960863025738395, 0.0009441921726051701221, 0.001888384345210362796, 0.003776768690420748142, 0.005665153035631133489, 0.007553537380841518836, 0.01133030607126228953, 0.01321869041647267401, 0.01416288258907786798, 0.01463497867538046324, 0.01510707476168306022 ),
 ( 0.000000000000000000, 0.1250000000000000000, 0.2500000000000000000, 0.3750000000000000000, 0.5000000000000000000, 0.6250000000000000000, 0.7500000000000000000, 0.8750000000000000000, 1.000000000000000000 ),
 .UNSPECIFIED. ) ;
#18812 = CARTESIAN_POINT ( 'NONE',  ( 1.317809913116059883, -26.19152339826795739, 6.959317978105164393 ) ) ;
#18813 = CARTESIAN_POINT ( 'NONE',  ( 5.031981677282425736, -30.24852985705353348, 7.778050822775632867 ) ) ;
#18814 = VERTEX_POINT ( 'NONE', #2199 ) ;
#18815 = CARTESIAN_POINT ( 'NONE',  ( 21.82816986786027158, 5.980044178900067564, 3.126748918376258235 ) ) ;
#18816 = FACE_OUTER_BOUND ( 'NONE', #20954, .T. ) ;
#18817 = CARTESIAN_POINT ( 'NONE',  ( 18.16951175210537883, -3.146849537680269648, 2.997227928983285494 ) ) ;
#18818 = DIRECTION ( 'NONE',  ( -0.000000000000000000, -0.000000000000000000, 1.000000000000000000 ) ) ;
#18819 = ORIENTED_EDGE ( 'NONE', *, *, #22386, .T. ) ;
#18820 = CARTESIAN_POINT ( 'NONE',  ( 79.38338525671692025, 64.07937768075929341, -3.690346394509879335 ) ) ;
#18822 = CARTESIAN_POINT ( 'NONE',  ( -1.673641830192087676, -29.98934475122311838, 6.882085323592687764 ) ) ;
#18821 = CARTESIAN_POINT ( 'NONE',  ( 24.72895772277339077, 0.6241560937809621512, 4.782015836530520758 ) ) ;
#18823 = AXIS2_PLACEMENT_3D ( 'NONE', #2178, #37951, #28286 ) ;
#18824 = CARTESIAN_POINT ( 'NONE',  ( 79.78729094670478617, 65.99503481514534542, -2.368810654844697439 ) ) ;
#18825 = CARTESIAN_POINT ( 'NONE',  ( 80.48656635915796187, 62.05344631111049836, 3.128253119413327177 ) ) ;
#18826 = EDGE_CURVE ( 'NONE', #34290, #36144, #40583, .T. ) ;
#18827 = CARTESIAN_POINT ( 'NONE',  ( 4.434886103410926594, -27.54940263586490801, 6.959317978105159952 ) ) ;
#18828 = AXIS2_PLACEMENT_3D ( 'NONE', #10711, #14211, #11113 ) ;
#18829 = CARTESIAN_POINT ( 'NONE',  ( -1.591993232420714444, -30.71360387936050529, 7.785344483711591934 ) ) ;
#18831 = ORIENTED_EDGE ( 'NONE', *, *, #21627, .F. ) ;
#18830 = CARTESIAN_POINT ( 'NONE',  ( 2.815854552281536805, -32.78175835696561791, 7.785868773668302545 ) ) ;
#18832 = CARTESIAN_POINT ( 'NONE',  ( 22.43090457150155004, 1.240285785788341810, -8.908344141805525140 ) ) ;
#18833 = DIRECTION ( 'NONE',  ( 1.000000000000000000, 0.000000000000000000, 0.000000000000000000 ) ) ;
#18834 = EDGE_LOOP ( 'NONE', ( #11278, #662, #15125, #15160, #37685, #3126 ) ) ;
#18835 = CARTESIAN_POINT ( 'NONE',  ( -73.09841737725705002, 0.2944336502508215769, 9.825022498446474017 ) ) ;
#18836 = CARTESIAN_POINT ( 'NONE',  ( 35.83985725928805266, -3.722406797855700056, 5.627729815070630082 ) ) ;
#18837 = EDGE_LOOP ( 'NONE', ( #6686, #23279, #8636, #15881 ) ) ;
#18838 = CARTESIAN_POINT ( 'NONE',  ( -52.01549048184568846, -38.28842912540938670, 6.800000000000000711 ) ) ;
#18839 = CARTESIAN_POINT ( 'NONE',  ( -80.59506793348410270, 11.48890230165596194, -2.592577747312847958 ) ) ;
#18840 = EDGE_CURVE ( 'NONE', #5389, #20836, #12061, .T. ) ;
#18841 = CARTESIAN_POINT ( 'NONE',  ( -37.07867591359219261, -24.55319635012989110, 6.700000000000000178 ) ) ;
#18842 = CARTESIAN_POINT ( 'NONE',  ( 25.73466472507932679, 2.638154739548788541, -3.516479417547335729 ) ) ;
#18843 = B_SPLINE_CURVE_WITH_KNOTS ( 'NONE', 3,
 ( #24929, #24092, #39954, #27189, #2719, #37265, #9061, #39747, #30910, #21840 ),
 .UNSPECIFIED., .F., .F.,
 ( 4, 3, 3, 4 ),
 ( 1.817454023025239628E-18, 3.025570593003134020E-05, 6.051145698344051330E-05, 6.468151674594376400E-05 ),
 .UNSPECIFIED. ) ;
#18844 = DIRECTION ( 'NONE',  ( -0.000000000000000000, -0.000000000000000000, -1.000000000000000000 ) ) ;
#18845 = CARTESIAN_POINT ( 'NONE',  ( 16.78011557480152760, 9.616836425704338609, 2.806367541052271708 ) ) ;
#18846 = LINE ( 'NONE', #15553, #39165 ) ;
#18847 = CARTESIAN_POINT ( 'NONE',  ( 4.327546298727369845, -31.72818190512046499, 7.680992449362112673 ) ) ;
#18848 = PLANE ( 'NONE',  #28956 ) ;
#18849 = CARTESIAN_POINT ( 'NONE',  ( -70.92837670882107659, -27.85319909218681644, 6.138794830819693793 ) ) ;
#18850 = CARTESIAN_POINT ( 'NONE',  ( 21.86238218247489939, 0.3889561109544238948, -7.946803484597631417 ) ) ;
#18851 = CARTESIAN_POINT ( 'NONE',  ( 30.79110773244140731, -3.772180204026406969, -4.560163372754496791 ) ) ;
#18852 = CARTESIAN_POINT ( 'NONE',  ( 24.57886943115599365, 2.978281377686288867, -3.576560291590100693 ) ) ;
#18853 = EDGE_LOOP ( 'NONE', ( #39790, #3410, #1497, #31814 ) ) ;
#18854 = AXIS2_PLACEMENT_3D ( 'NONE', #19433, #22338, #25211 ) ;
#18855 = CARTESIAN_POINT ( 'NONE',  ( 67.14845837397145090, 58.06767444754134289, 3.999036733496184048 ) ) ;
#18856 = CARTESIAN_POINT ( 'NONE',  ( 32.81185505326144636, -0.8379172344137845174, 5.327481557411383406 ) ) ;
#18857 = CIRCLE ( 'NONE', #25448, 0.1000000000000028644 ) ;
#18858 = AXIS2_PLACEMENT_3D ( 'NONE', #28372, #32096, #12720 ) ;
#18859 = DIRECTION ( 'NONE',  ( 1.000000000000000000, -0.000000000000000000, -0.000000000000000000 ) ) ;
#18860 = CARTESIAN_POINT ( 'NONE',  ( 86.54108089765607303, -0.3148381559440514010, -5.858094985366312457 ) ) ;
#18861 = CARTESIAN_POINT ( 'NONE',  ( 35.94440725716257390, -2.118452061082618076, -5.816392089891535555 ) ) ;
#18862 = ORIENTED_EDGE ( 'NONE', *, *, #5073, .F. ) ;
#18863 = CARTESIAN_POINT ( 'NONE',  ( 24.40553902836886735, 2.951342829192842299, 3.698142355126557757 ) ) ;
#18864 = EDGE_CURVE ( 'NONE', #37836, #5603, #39856, .T. ) ;
#18865 = DIRECTION ( 'NONE',  ( 0.01395351027862084224, -0.9999026450364577601, 0.000000000000000000 ) ) ;
#18866 = EDGE_LOOP ( 'NONE', ( #19328, #3007, #15648, #600 ) ) ;
#18867 = DIRECTION ( 'NONE',  ( -1.000000000000000000, 0.000000000000000000, -0.000000000000000000 ) ) ;
#18868 = PRODUCT_DEFINITION_CONTEXT ( 'detailed design', #27896, 'design' ) ;
#18869 = VERTEX_POINT ( 'NONE', #19058 ) ;
#18870 = ORIENTED_EDGE ( 'NONE', *, *, #34462, .F. ) ;
#18871 = CARTESIAN_POINT ( 'NONE',  ( 80.80742440666386983, 61.88848183320471463, -2.854164747638210820 ) ) ;
#18872 = ADVANCED_FACE ( 'NONE', ( #21949 ), #12465, .F. ) ;
#18873 = CARTESIAN_POINT ( 'NONE',  ( -1.730496578629491689, -28.93663728645029920, 7.781480525794718162 ) ) ;
#18874 = CARTESIAN_POINT ( 'NONE',  ( 81.00146336277434500, 61.29413404061270398, 1.724274471760811167 ) ) ;
#18877 = ORIENTED_EDGE ( 'NONE', *, *, #25768, .F. ) ;
#18876 = ORIENTED_EDGE ( 'NONE', *, *, #16890, .F. ) ;
#18875 = CARTESIAN_POINT ( 'NONE',  ( -2.248748702180634940, -26.64985754041175525, 6.700000000000000178 ) ) ;
#18878 = DIRECTION ( 'NONE',  ( -1.000000000000000000, -5.325537380878540815E-15, 0.000000000000000000 ) ) ;
#18879 = EDGE_CURVE ( 'NONE', #5466, #39349, #15554, .T. ) ;
#18880 = TOROIDAL_SURFACE ( 'NONE', #16891, 5.681288188914805026, 1.000000000000000000 ) ;
#18881 = DIRECTION ( 'NONE',  ( -1.000000000000000000, 0.000000000000000000, 0.000000000000000000 ) ) ;
#18882 = CARTESIAN_POINT ( 'NONE',  ( 27.16049945410617994, -4.514626814156768475, 3.607957147575535650 ) ) ;
#18883 =( GEOMETRIC_REPRESENTATION_CONTEXT ( 3 ) GLOBAL_UNCERTAINTY_ASSIGNED_CONTEXT ( ( #6531 ) ) GLOBAL_UNIT_ASSIGNED_CONTEXT ( ( #39307, #19973, #1460 ) ) REPRESENTATION_CONTEXT ( 'NONE', 'WORKASPACE' ) );
#18884 = FACE_OUTER_BOUND ( 'NONE', #26632, .T. ) ;
#18885 = AXIS2_PLACEMENT_3D ( 'NONE', #5628, #18170, #5835 ) ;
#18886 = CARTESIAN_POINT ( 'NONE',  ( 22.87953249933443800, 4.317477008691624540, -3.087559474757433531 ) ) ;
#18887 = ORIENTED_EDGE ( 'NONE', *, *, #24394, .T. ) ;
#18888 = PLANE ( 'NONE',  #17584 ) ;
#18889 = VECTOR ( 'NONE', #15175, 1000.000000000000000 ) ;
#18890 = ORIENTED_EDGE ( 'NONE', *, *, #11134, .T. ) ;
#18891 = CARTESIAN_POINT ( 'NONE',  ( -0.9451523768770455636, -31.70561910709598052, 6.880147297696979969 ) ) ;
#18892 = DIRECTION ( 'NONE',  ( 0.3420201433256662704, 0.9396926207859093161, -0.000000000000000000 ) ) ;
#18893 = CARTESIAN_POINT ( 'NONE',  ( -76.47431036836700002, -5.779992581808538255, -8.329558765771590600 ) ) ;
#18894 = EDGE_CURVE ( 'NONE', #13304, #8526, #38528, .T. ) ;
#18895 = DIRECTION ( 'NONE',  ( -1.000000000000000000, 0.000000000000000000, 0.000000000000000000 ) ) ;
#18896 = CARTESIAN_POINT ( 'NONE',  ( 81.15394892944381411, 63.54712375394903745, 3.396356880840902370 ) ) ;
#18897 = CARTESIAN_POINT ( 'NONE',  ( 87.47409246771869107, -1.962666243356603557, 3.672687813029068771 ) ) ;
#18898 = CARTESIAN_POINT ( 'NONE',  ( -70.92837670882107659, 13.87661300689599742, 0.000000000000000000 ) ) ;
#18899 = ORIENTED_EDGE ( 'NONE', *, *, #26499, .F. ) ;
#18900 = DIRECTION ( 'NONE',  ( 0.000000000000000000, 1.000000000000000000, 0.000000000000000000 ) ) ;
#18901 = CARTESIAN_POINT ( 'NONE',  ( 22.06632471839147414, 4.214975381128987841, 2.277617108976539129 ) ) ;
#18902 = CARTESIAN_POINT ( 'NONE',  ( 4.093191441545242171, -27.01561806821104739, 6.971170733404101760 ) ) ;
#18903 = PLANE ( 'NONE',  #28495 ) ;
#18904 = DIRECTION ( 'NONE',  ( -0.8820753183692411348, 0.4711084086744811161, -0.000000000000000000 ) ) ;
#18905 = PLANE ( 'NONE',  #4320 ) ;
#18906 = VERTEX_POINT ( 'NONE', #25036 ) ;
#18907 = CARTESIAN_POINT ( 'NONE',  ( 25.29651566011737529, 1.736446006507980089, 4.154531085941302493 ) ) ;
#18908 = EDGE_CURVE ( 'NONE', #18951, #1190, #31243, .T. ) ;
#18909 = CIRCLE ( 'NONE', #24163, 12.80480339192541628 ) ;
#18910 = CARTESIAN_POINT ( 'NONE',  ( 87.04213330793400871, 0.5878691963681530464, -4.891134986362597914 ) ) ;
#18911 = ORIENTED_EDGE ( 'NONE', *, *, #16086, .F. ) ;
#18913 = CARTESIAN_POINT ( 'NONE',  ( 6.053772676492744864, -27.07209504432901070, 7.635761828346577573 ) ) ;
#18912 = CARTESIAN_POINT ( 'NONE',  ( 81.08176929032271119, 62.48897713179231772, -3.134554000843273514 ) ) ;
#18914 = FACE_OUTER_BOUND ( 'NONE', #28326, .T. ) ;
#18915 = VECTOR ( 'NONE', #22669, 1000.000000000000000 ) ;
#18916 = AXIS2_PLACEMENT_3D ( 'NONE', #25659, #9600, #34754 ) ;
#18917 = EDGE_LOOP ( 'NONE', ( #5290, #2830, #23070, #21938, #39343, #37597 ) ) ;
#18918 = CARTESIAN_POINT ( 'NONE',  ( 28.09640073134533367, -4.183647163201285935, -3.920990555712708492 ) ) ;
#18919 = EDGE_LOOP ( 'NONE', ( #18650, #16047, #35346, #29959, #14192 ) ) ;
#18920 = LINE ( 'NONE', #17021, #13627 ) ;
#18921 = ORIENTED_EDGE ( 'NONE', *, *, #19481, .F. ) ;
#18922 = CARTESIAN_POINT ( 'NONE',  ( 81.09335400879909628, 61.74513338965305564, -2.494286432550476995 ) ) ;
#18923 = EDGE_CURVE ( 'NONE', #21155, #29030, #6298, .T. ) ;
#18924 = CARTESIAN_POINT ( 'NONE',  ( 35.97450302262141264, -3.154424668010459953, 5.821089261960223027 ) ) ;
#18925 = EDGE_CURVE ( 'NONE', #16760, #9551, #13700, .T. ) ;
#18927 = CARTESIAN_POINT ( 'NONE',  ( 14.77222812468937363, 12.33286846116137347, 2.511961485181785747 ) ) ;
#18926 = CARTESIAN_POINT ( 'NONE',  ( 22.26021987840845284, 2.688082151531064223, 4.954761472530542221 ) ) ;
#18928 = VERTEX_POINT ( 'NONE', #36969 ) ;
#18929 = EDGE_CURVE ( 'NONE', #37836, #2601, #9167, .T. ) ;
#18930 = CARTESIAN_POINT ( 'NONE',  ( 79.49585004866908378, 66.23094581382571278, -1.662695954554820554 ) ) ;
#18931 = DIRECTION ( 'NONE',  ( 1.000000000000000000, 0.000000000000000000, 0.000000000000000000 ) ) ;
#18932 = VECTOR ( 'NONE', #9818, 1000.000000000000000 ) ;
#18934 = CARTESIAN_POINT ( 'NONE',  ( 86.69898499333136499, 0.9733096701313710408, -5.030742382222590514 ) ) ;
#18933 = DIRECTION ( 'NONE',  ( -1.000000000000000000, 0.000000000000000000, 0.000000000000000000 ) ) ;
#18935 = CARTESIAN_POINT ( 'NONE',  ( 21.85643539959776760, -15.11462368761991293, 2.500000000000000000 ) ) ;
#18936 = CARTESIAN_POINT ( 'NONE',  ( -80.92837670882107659, 2.429809908903242555, 15.50000000000000000 ) ) ;
#18937 = CARTESIAN_POINT ( 'NONE',  ( 74.80267162900737787, 60.00335986791986898, 3.708893976703238948 ) ) ;
#18938 = VERTEX_POINT ( 'NONE', #30815 ) ;
#18939 = CARTESIAN_POINT ( 'NONE',  ( 21.84823020783428760, 4.269274562117517213, -4.178901852297197017 ) ) ;
#18940 = VERTEX_POINT ( 'NONE', #31215 ) ;
#18941 = VECTOR ( 'NONE', #1091, 1000.000000000000000 ) ;
#18942 = CARTESIAN_POINT ( 'NONE',  ( 21.85643539959780313, 0.8081825263151607430, -15.79083533483346535 ) ) ;
#18943 = CARTESIAN_POINT ( 'NONE',  ( -57.44564769468265553, 32.97701904356408420, -4.025706866804887873 ) ) ;
#18944 = ORIENTED_EDGE ( 'NONE', *, *, #28941, .T. ) ;
#18945 = CARTESIAN_POINT ( 'NONE',  ( -1.368289865235002178, -28.08953866528909415, 7.505001789837628223 ) ) ;
#18946 = CARTESIAN_POINT ( 'NONE',  ( 81.90837201943169532, 62.87926165960877256, 2.626729253126739216 ) ) ;
#18947 = CARTESIAN_POINT ( 'NONE',  ( 87.66750401967712492, -0.1145768689462967616, 4.387407120178886899 ) ) ;
#18948 = EDGE_LOOP ( 'NONE', ( #31742, #13257, #17727, #16986 ) ) ;
#18949 = CIRCLE ( 'NONE', #24193, 0.1000000000000028644 ) ;
#18950 = CARTESIAN_POINT ( 'NONE',  ( 0.4535750661203729606, -32.73306980853894999, 7.778050822775633755 ) ) ;
#18951 = VERTEX_POINT ( 'NONE', #27695 ) ;
#18952 = CARTESIAN_POINT ( 'NONE',  ( 15.57034054627223085, -3.673666129765767341, 2.635867821429580982 ) ) ;
#18953 = CARTESIAN_POINT ( 'NONE',  ( 36.99252390190989104, -2.719198568494679780, -5.979976041101225270 ) ) ;
#18954 = DIRECTION ( 'NONE',  ( 0.5000000000000015543, 0.000000000000000000, 0.8660254037844378194 ) ) ;
#18955 = CARTESIAN_POINT ( 'NONE',  ( 21.95206253975293009, 4.960245780819739991, 3.632525366124041533 ) ) ;
#18956 = CARTESIAN_POINT ( 'NONE',  ( -0.07645708395594488782, -32.58535952412007930, 6.894806418505347700 ) ) ;
#18957 = CARTESIAN_POINT ( 'NONE',  ( -1.273818662545060709, -31.21737738347374602, 7.785172627573962778 ) ) ;
#18958 = CARTESIAN_POINT ( 'NONE',  ( 30.71037367896834880, -3.512617482052606821, 4.877620608057760876 ) ) ;
#18959 = EDGE_LOOP ( 'NONE', ( #29748, #3815, #36388, #33622 ) ) ;
#18960 = VERTEX_POINT ( 'NONE', #9578 ) ;
#18961 = CARTESIAN_POINT ( 'NONE',  ( 37.00923632130533747, -2.250050275659773114, 5.913415034251472413 ) ) ;
#18962 = VECTOR ( 'NONE', #16106, 1000.000000000000000 ) ;
#18963 = CARTESIAN_POINT ( 'NONE',  ( -1.135875017054286618, -33.94315967623287378, 6.894806418505347700 ) ) ;
#18964 = CARTESIAN_POINT ( 'NONE',  ( 66.41505992881675979, 57.81052748253004125, -4.000000000000023093 ) ) ;
#18965 = ADVANCED_FACE ( 'NONE', ( #21540 ), #12037, .F. ) ;
#18966 = CARTESIAN_POINT ( 'NONE',  ( 86.77891424509762430, -1.040114302260652046, -5.346981141011549532 ) ) ;
#18967 = CARTESIAN_POINT ( 'NONE',  ( -0.5067439190362983403, -26.87212914619025739, 7.785096263473212375 ) ) ;
#18968 = ORIENTED_EDGE ( 'NONE', *, *, #35263, .F. ) ;
#18969 = CARTESIAN_POINT ( 'NONE',  ( 88.12997514058099569, -0.6340463821490202045, -2.468799945080301761 ) ) ;
#18970 = EDGE_CURVE ( 'NONE', #8010, #11160, #23882, .T. ) ;
#18971 = CARTESIAN_POINT ( 'NONE',  ( -71.80703402346622966, 3.441338441424772743, -9.961354656704822119 ) ) ;
#18972 = CYLINDRICAL_SURFACE ( 'NONE', #20066, 1.000000000000000888 ) ;
#18973 = CARTESIAN_POINT ( 'NONE',  ( 5.904749997263966321, -30.32498317729107740, 7.635761828346577573 ) ) ;
#18974 = CARTESIAN_POINT ( 'NONE',  ( 2.272716057154847924, -26.11704110451741556, 7.685194954629195330 ) ) ;
#18975 = ORIENTED_EDGE ( 'NONE', *, *, #9733, .T. ) ;
#18976 = FACE_BOUND ( 'NONE', #21422, .T. ) ;
#18977 = CYLINDRICAL_SURFACE ( 'NONE', #20581, 6.406751979251626317 ) ;
#18978 = ORIENTED_EDGE ( 'NONE', *, *, #19993, .T. ) ;
#18979 = CARTESIAN_POINT ( 'NONE',  ( 22.42121470216353174, 4.796581755807473257, 3.154605090790354005 ) ) ;
#18980 = EDGE_CURVE ( 'NONE', #17250, #39647, #6927, .T. ) ;
#18981 = CARTESIAN_POINT ( 'NONE',  ( 80.34788146105260864, 66.29920961842009319, -1.394285451510165252 ) ) ;
#18982 = AXIS2_PLACEMENT_3D ( 'NONE', #32034, #9575, #22156 ) ;
#18983 = CARTESIAN_POINT ( 'NONE',  ( 79.02959213847955766, 65.76024385718582721, 2.482170738714648550 ) ) ;
#18984 = CARTESIAN_POINT ( 'NONE',  ( -1.752170693794088185, -28.99562711716245644, 7.714178352335857802 ) ) ;
#18985 = ORIENTED_EDGE ( 'NONE', *, *, #5785, .F. ) ;
#18986 = CARTESIAN_POINT ( 'NONE',  ( 76.63893934653984275, 63.44172143924971152, -3.539370024148525307 ) ) ;
#18987 = CARTESIAN_POINT ( 'NONE',  ( 14.88717023490364966, 12.58473342882037471, -2.513050065054561522 ) ) ;
#18989 = DIRECTION ( 'NONE',  ( -0.000000000000000000, -0.000000000000000000, -1.000000000000000000 ) ) ;
#18988 = CARTESIAN_POINT ( 'NONE',  ( 3.930644293244915044, -32.25600374108427104, 7.778495531946298058 ) ) ;
#18990 = CARTESIAN_POINT ( 'NONE',  ( 19.12106624447652337, 7.213790669980742365, -3.190702850821951486 ) ) ;
#18991 = CARTESIAN_POINT ( 'NONE',  ( 78.67710717883703353, 66.04916176178686271, -1.122020883098632904 ) ) ;
#18992 = CARTESIAN_POINT ( 'NONE',  ( 78.66234234182425666, 62.19549841187289019, 3.710351296122935683 ) ) ;
#18993 = ORIENTED_EDGE ( 'NONE', *, *, #29895, .F. ) ;
#18994 = DIRECTION ( 'NONE',  ( 0.000000000000000000, 0.000000000000000000, 1.000000000000000000 ) ) ;
#18995 = AXIS2_PLACEMENT_3D ( 'NONE', #8906, #5224, #21490 ) ;
#18996 = CARTESIAN_POINT ( 'NONE',  ( 3.438683469850188690, -26.53211252316276259, 7.635761828346582014 ) ) ;
#18997 = CARTESIAN_POINT ( 'NONE',  ( 81.57551674523639917, 65.32158946912302611, 2.325514254128254965 ) ) ;
#18998 =( BOUNDED_CURVE ( )  B_SPLINE_CURVE ( 3, ( #7440, #7648, #681, #16109 ),
 .UNSPECIFIED., .F., .F. ) 
 B_SPLINE_CURVE_WITH_KNOTS ( ( 4, 4 ),
 ( 1.347909859412855793, 1.534781240595299856 ),
 .UNSPECIFIED. ) 
 CURVE ( )  GEOMETRIC_REPRESENTATION_ITEM ( )  RATIONAL_B_SPLINE_CURVE ( ( 1.000000000000000000, 0.9970920404276226723, 0.9970920404276226723, 1.000000000000000000 ) ) 
 REPRESENTATION_ITEM ( '' )  );
#19000 = CARTESIAN_POINT ( 'NONE',  ( -1.699260392630454364, -29.52118006577551412, 6.894806418505346812 ) ) ;
#18999 = FACE_OUTER_BOUND ( 'NONE', #533, .T. ) ;
#19001 = CARTESIAN_POINT ( 'NONE',  ( 29.52748857962093965, -2.713093490715668743, -5.368793458836177201 ) ) ;
#19002 = CARTESIAN_POINT ( 'NONE',  ( -1.414328007069049375, -31.16634214640615141, 7.006908160621414083 ) ) ;
#19003 = CARTESIAN_POINT ( 'NONE',  ( -8.878675913592189772, -26.64985754041175525, 6.700000000000000178 ) ) ;
#19004 = CARTESIAN_POINT ( 'NONE',  ( 1.527332651948331899, -33.06564960244016760, 7.009310105710487626 ) ) ;
#19005 = PLANE ( 'NONE',  #26125 ) ;
#19006 = DIRECTION ( 'NONE',  ( -1.000000000000000000, 0.000000000000000000, 0.000000000000000000 ) ) ;
#19007 = DIRECTION ( 'NONE',  ( -0.000000000000000000, -1.000000000000000000, -0.000000000000000000 ) ) ;
#19008 = CARTESIAN_POINT ( 'NONE',  ( -22.87867591359218977, -26.64985754041175525, 6.800000000000000711 ) ) ;
#19009 = CARTESIAN_POINT ( 'NONE',  ( 37.09088143372432711, -3.108852245844890394, -5.978546864269264738 ) ) ;
#19010 = CARTESIAN_POINT ( 'NONE',  ( 3.056550635926903237, -26.44443126081507600, 7.386948897581450346 ) ) ;
#19011 = CARTESIAN_POINT ( 'NONE',  ( 4.358774179341475374, -27.29331111184919934, 7.710604733652631992 ) ) ;
#19012 = CARTESIAN_POINT ( 'NONE',  ( 23.82967770391586626, -2.761398267376460769, -3.925595547265982255 ) ) ;
#19013 = CARTESIAN_POINT ( 'NONE',  ( 1.075454873741154005, -26.12617409861640638, 7.750000000000000888 ) ) ;
#19014 = CARTESIAN_POINT ( 'NONE',  ( 2.156915105547790645, -32.93915630191352761, 6.865312560952603782 ) ) ;
#19015 = CARTESIAN_POINT ( 'NONE',  ( -64.08758708074093136, 36.76354445449491948, -3.435823087746522120 ) ) ;
#19016 = VECTOR ( 'NONE', #20813, 1000.000000000000000 ) ;
#19017 = CARTESIAN_POINT ( 'NONE',  ( -1.473412216555795018, -28.35051274117816789, 7.785172627573962778 ) ) ;
#19018 = DIRECTION ( 'NONE',  ( 1.000000000000000000, 8.966158204770716457E-16, 0.000000000000000000 ) ) ;
#19019 = ORIENTED_EDGE ( 'NONE', *, *, #17981, .F. ) ;
#19020 = CARTESIAN_POINT ( 'NONE',  ( 5.067143666762728316, -33.49802700238250708, 7.695279973900954751 ) ) ;
#19021 = CARTESIAN_POINT ( 'NONE',  ( 68.59886892412534110, 58.63590986220410173, -3.993768376023888234 ) ) ;
#19022 = EDGE_LOOP ( 'NONE', ( #825, #6827, #8327, #3615 ) ) ;
#19023 = FACE_OUTER_BOUND ( 'NONE', #27109, .T. ) ;
#19024 = CARTESIAN_POINT ( 'NONE',  ( 0.04964925160023719169, -26.59754819687732308, 6.887041543973313473 ) ) ;
#19025 = CARTESIAN_POINT ( 'NONE',  ( 22.99364181696555676, 3.589457867690851067, 3.733328102171712626 ) ) ;
#19026 = CARTESIAN_POINT ( 'NONE',  ( 1.139827216511555052, -26.21645895774650370, 7.782167645815905033 ) ) ;
#19028 = EDGE_CURVE ( 'NONE', #25150, #25263, #26052, .T. ) ;
#19027 = CARTESIAN_POINT ( 'NONE',  ( -80.92837670882107659, 2.429809908903242555, 15.50000000000000000 ) ) ;
#19029 = VERTEX_POINT ( 'NONE', #1353 ) ;
#19030 = B_SPLINE_CURVE_WITH_KNOTS ( 'NONE', 3,
 ( #3876, #16392, #29363, #573, #6738, #13110, #34766, #973, #35363, #38014, #7330, #16584, #25670, #25470, #13510, #29165, #28963, #768, #13300, #19886, #25873, #38413, #22793, #32461, #13718, #26284, #38818, #33485, #35952, #1774, #8117 ),
 .UNSPECIFIED., .F., .F.,
 ( 4, 3, 3, 3, 3, 3, 3, 3, 3, 3, 4 ),
 ( 6.484403375994738403E-05, 8.983333709522376971E-05, 0.0001203539973219378077, 0.0001514144607149686141, 0.0001828916862241615547, 0.0002144221682127263285, 0.0002455195857862215369, 0.0002758614570916280775, 0.0003055381793602579294, 0.0003350143730643711853, 0.0003497271997307910231 ),
 .UNSPECIFIED. ) ;
#19031 = CARTESIAN_POINT ( 'NONE',  ( 21.98812987590129708, 5.622928254491678324, 3.083847952653145708 ) ) ;
#19032 = EDGE_CURVE ( 'NONE', #25414, #40311, #20687, .T. ) ;
#19033 = DIRECTION ( 'NONE',  ( 1.000000000000000000, -0.000000000000000000, -0.000000000000000000 ) ) ;
#19034 = EDGE_CURVE ( 'NONE', #17047, #32358, #21037, .T. ) ;
#19035 = CARTESIAN_POINT ( 'NONE',  ( -0.5217032702065468319, -32.27405686018897768, 7.695279973900954751 ) ) ;
#19036 = ORIENTED_EDGE ( 'NONE', *, *, #36767, .F. ) ;
#19037 = CARTESIAN_POINT ( 'NONE',  ( 80.05518365985739138, 61.93129665380739368, -3.228498513792977587 ) ) ;
#19039 = CARTESIAN_POINT ( 'NONE',  ( -1.675359094926574866, -29.97529103330290212, 7.013842709614101167 ) ) ;
#19038 = CARTESIAN_POINT ( 'NONE',  ( 24.69442438258014860, 0.6739242910027807287, 4.791210749312426742 ) ) ;
#19040 = CARTESIAN_POINT ( 'NONE',  ( 80.93493477626104493, 64.98323193449208190, -3.125232205748941006 ) ) ;
#19041 = CARTESIAN_POINT ( 'NONE',  ( 79.60839748543872929, 63.85977214187242623, 3.734652355492746434 ) ) ;
#19042 = VECTOR ( 'NONE', #32426, 1000.000000000000000 ) ;
#19043 = CARTESIAN_POINT ( 'NONE',  ( 81.04763707098177861, 66.10603528134694784, 1.000000000000000000 ) ) ;
#19044 = CARTESIAN_POINT ( 'NONE',  ( -70.92837670882107659, -23.80776546975053520, -10.00000000000000888 ) ) ;
#19045 = CARTESIAN_POINT ( 'NONE',  ( 21.85643539959775694, 2.837881715527333260, -11.82040581148825353 ) ) ;
#19046 = ORIENTED_EDGE ( 'NONE', *, *, #1576, .F. ) ;
#19047 = CARTESIAN_POINT ( 'NONE',  ( -75.23145188694429919, 8.172688008897852185, 9.065593416914579095 ) ) ;
#19048 = DIRECTION ( 'NONE',  ( -0.000000000000000000, -0.000000000000000000, -1.000000000000000000 ) ) ;
#19049 = VERTEX_POINT ( 'NONE', #37982 ) ;
#19050 = LINE ( 'NONE', #31819, #33397 ) ;
#19051 = DIRECTION ( 'NONE',  ( -0.000000000000000000, 0.7508067542896647018, 0.6605219282605379050 ) ) ;
#19052 = VECTOR ( 'NONE', #31970, 1000.000000000000000 ) ;
#19053 = CARTESIAN_POINT ( 'NONE',  ( 32.00641903142002320, -3.049359518210221776, -5.201773786605959238 ) ) ;
#19054 = CARTESIAN_POINT ( 'NONE',  ( 37.01057800680626286, -2.248353986704187513, -5.912806876547849200 ) ) ;
#19055 = FACE_OUTER_BOUND ( 'NONE', #1457, .T. ) ;
#19056 = CARTESIAN_POINT ( 'NONE',  ( 17.79089637503647126, 8.596792681990928386, 2.958187967343824720 ) ) ;
#19057 = DIRECTION ( 'NONE',  ( -0.000000000000000000, 1.000000000000000000, -0.000000000000000000 ) ) ;
#19058 = CARTESIAN_POINT ( 'NONE',  ( -70.92837670882107659, -36.87473357531881391, -5.950000000000010836 ) ) ;
#19059 = DIRECTION ( 'NONE',  ( 0.000000000000000000, 1.000000000000000000, 0.000000000000000000 ) ) ;
#19060 = CARTESIAN_POINT ( 'NONE',  ( 3.551251297819357777, -25.49307895267003587, 6.700000000000000178 ) ) ;
#19061 = CARTESIAN_POINT ( 'NONE',  ( 21.97109001347866553, 0.9630426953691740843, -7.010656934984691446 ) ) ;
#19062 = DIRECTION ( 'NONE',  ( -1.000000000000000000, 0.000000000000000000, 0.000000000000000000 ) ) ;
#19063 = DIRECTION ( 'NONE',  ( -0.6427876096865327016, -0.7660444431189835646, -0.000000000000000000 ) ) ;
#19064 = ORIENTED_EDGE ( 'NONE', *, *, #35951, .T. ) ;
#19065 = CARTESIAN_POINT ( 'NONE',  ( 67.47105843325410035, 58.09313517554802075, 3.997566301760142160 ) ) ;
#19066 = CARTESIAN_POINT ( 'NONE',  ( 36.94063378041538215, -3.101443124462082146, 5.970284356405101356 ) ) ;
#19067 = AXIS2_PLACEMENT_3D ( 'NONE', #18657, #28138, #25062 ) ;
#19068 = CYLINDRICAL_SURFACE ( 'NONE', #16158, 4.357836081054403010 ) ;
#19069 = CARTESIAN_POINT ( 'NONE',  ( 86.22674662394152278, 0.2046669357502599595, -6.014203425234573963 ) ) ;
#19070 = CARTESIAN_POINT ( 'NONE',  ( 24.97750119118845546, 3.110153433881029272, 2.920260296092602292 ) ) ;
#19071 = EDGE_LOOP ( 'NONE', ( #9238, #6821, #10446, #2275 ) ) ;
#19072 = CARTESIAN_POINT ( 'NONE',  ( 24.66036887970934544, 2.991013199203838901, 3.498539802152044853 ) ) ;
#19073 = LINE ( 'NONE', #6317, #32479 ) ;
#19074 = CARTESIAN_POINT ( 'NONE',  ( 0.6874672402166666085, -34.21933100612760370, 6.894806418505347700 ) ) ;
#19075 = EDGE_LOOP ( 'NONE', ( #11674, #6165, #24930, #17048, #27279, #16230, #31180 ) ) ;
#19076 = CARTESIAN_POINT ( 'NONE',  ( 3.985769669582015062, -26.93874319361661662, 7.785593909369613819 ) ) ;
#19077 = AXIS2_PLACEMENT_3D ( 'NONE', #19259, #25845, #31828 ) ;
#19078 = EDGE_CURVE ( 'NONE', #3677, #4425, #22769, .T. ) ;
#19079 = VERTEX_POINT ( 'NONE', #19861 ) ;
#19080 = CARTESIAN_POINT ( 'NONE',  ( 80.71678001510446165, 62.11300466482757088, -3.061371641637534502 ) ) ;
#19081 = DIRECTION ( 'NONE',  ( -0.000000000000000000, -1.000000000000000000, -0.000000000000000000 ) ) ;
#19082 = CARTESIAN_POINT ( 'NONE',  ( 80.98641699598172750, 61.40056178693504307, 2.031354376635673198 ) ) ;
#19084 = EDGE_LOOP ( 'NONE', ( #21350, #2710, #17830, #39510 ) ) ;
#19083 = CARTESIAN_POINT ( 'NONE',  ( -1.340386146056437688, -31.09100870292229857, 6.988553391373219625 ) ) ;
#19085 = CARTESIAN_POINT ( 'NONE',  ( -40.24874870218063450, -26.64985754041175525, 6.800000000000000711 ) ) ;
#19086 = CARTESIAN_POINT ( 'NONE',  ( 28.09351773336840452, -4.184899630424881778, 3.919764035321353646 ) ) ;
#19087 = CARTESIAN_POINT ( 'NONE',  ( -30.87867591359218977, -24.55319635012989110, 6.800000000000000711 ) ) ;
#19088 = CARTESIAN_POINT ( 'NONE',  ( -54.89797088024758409, 31.42847739604817647, 1.178388813972039983 ) ) ;
#19089 = CARTESIAN_POINT ( 'NONE',  ( 23.74582114624947238, 3.564727581926975475, -3.175216399458318683 ) ) ;
#19090 = EDGE_LOOP ( 'NONE', ( #31783, #9996, #19555, #25897 ) ) ;
#19091 = CARTESIAN_POINT ( 'NONE',  ( -64.66796849410253856, 36.23110552202045653, -6.165526157072432234 ) ) ;
#19092 = VECTOR ( 'NONE', #28784, 1000.000000000000000 ) ;
#19093 = CARTESIAN_POINT ( 'NONE',  ( -1.033767024100737508, -31.59091637407721009, 6.969307238440508812 ) ) ;
#19094 = CARTESIAN_POINT ( 'NONE',  ( -68.71186372058383540, 37.81212149306785619, 9.800414904976364028 ) ) ;
#19095 = LINE ( 'NONE', #22403, #20336 ) ;
#19096 = DIRECTION ( 'NONE',  ( 0.000000000000000000, -0.000000000000000000, -1.000000000000000000 ) ) ;
#19097 = CARTESIAN_POINT ( 'NONE',  ( -75.45330471031414277, 33.71485196875532608, -46.17089178453873188 ) ) ;
#19098 = CARTESIAN_POINT ( 'NONE',  ( 79.83674225097152544, 65.44563770485291343, 3.036434590848153370 ) ) ;
#19099 = CARTESIAN_POINT ( 'NONE',  ( 85.08782340246310127, 1.754895396694989840, 5.093632142551737907 ) ) ;
#19100 = CARTESIAN_POINT ( 'NONE',  ( -0.01837800939314739035, -32.61883756299590686, 7.695279973900954751 ) ) ;
#19101 = ORIENTED_EDGE ( 'NONE', *, *, #1590, .F. ) ;
#19102 = CARTESIAN_POINT ( 'NONE',  ( 2.866894658930008610, -26.27004123098783950, 7.670465701733748531 ) ) ;
#19103 = CARTESIAN_POINT ( 'NONE',  ( 22.06908225159077119, 4.294879054371497418, -1.925114753942556156 ) ) ;
#19104 = ADVANCED_FACE ( 'NONE', ( #35530 ), #13078, .F. ) ;
#19105 = CARTESIAN_POINT ( 'NONE',  ( 1.790155505744531084, -26.17111536485493772, 7.778050822775631978 ) ) ;
#19106 = VECTOR ( 'NONE', #14075, 1000.000000000000227 ) ;
#19107 = DIRECTION ( 'NONE',  ( -0.7126435865141306225, 0.000000000000000000, -0.7015262779114384006 ) ) ;
#19108 = CARTESIAN_POINT ( 'NONE',  ( 4.632456985502078517, -27.84858802096400510, 7.740055089680403455 ) ) ;
#19109 = CARTESIAN_POINT ( 'NONE',  ( 85.58452164909124349, 1.000110208193303540, 5.791573931091940075 ) ) ;
#19110 = ORIENTED_EDGE ( 'NONE', *, *, #30891, .T. ) ;
#19111 = CARTESIAN_POINT ( 'NONE',  ( 33.46269705087502899, -3.085794937887296641, 5.429061191812215803 ) ) ;
#19112 = EDGE_CURVE ( 'NONE', #10847, #4150, #16557, .T. ) ;
#19113 = CARTESIAN_POINT ( 'NONE',  ( 86.62997685915109969, 1.050822881766228845, -5.316720303788503799 ) ) ;
#19114 = ORIENTED_EDGE ( 'NONE', *, *, #14221, .T. ) ;
#19116 = CARTESIAN_POINT ( 'NONE',  ( 23.38715862913678478, 3.561327236325438683, 3.087504282192082616 ) ) ;
#19115 = CARTESIAN_POINT ( 'NONE',  ( 79.50768156050780533, 65.53910429656815495, -2.885071930847946664 ) ) ;
#19117 = CARTESIAN_POINT ( 'NONE',  ( -1.334894404175721805, -31.29013112173537792, 7.781480525794719050 ) ) ;
#19118 = CARTESIAN_POINT ( 'NONE',  ( -69.62722026347231008, -46.36434999406230872, 9.915139134996609371 ) ) ;
#19119 = ORIENTED_EDGE ( 'NONE', *, *, #30973, .F. ) ;
#19120 = DIRECTION ( 'NONE',  ( 1.000000000000000000, 0.000000000000000000, 0.000000000000000000 ) ) ;
#19121 = ORIENTED_EDGE ( 'NONE', *, *, #2208, .T. ) ;
#19122 = CARTESIAN_POINT ( 'NONE',  ( -71.86802756984693019, 3.923644143335089929, 9.956082279489690379 ) ) ;
#19123 = ORIENTED_EDGE ( 'NONE', *, *, #1516, .T. ) ;
#19124 = EDGE_CURVE ( 'NONE', #13553, #22791, #25640, .T. ) ;
#19125 = B_SPLINE_CURVE_WITH_KNOTS ( 'NONE', 3,
 ( #28174, #5600, #23908, #30308, #36282, #12530, #8254, #18140, #1712, #8057, #4990, #36482, #5394, #20826, #33422, #5192, #2120, #14638, #36680, #8462, #21046, #804, #4104, #13547, #196, #6973, #6578, #19122, #6370, #3310, #28805, #12732, #22829, #29200, #1014, #3506, #10051, #16429, #38448, #25508, #13149, #606, #9854, #19732, #25312, #38054, #3708, #32113, #22431, #25709, #37843, #28597, #7171, #15831, #38251, #35401, #31488, #28386, #16231, #23031, #12942, #9647, #31690, #32307, #29002, #34798, #34998, #16616 ),
 .UNSPECIFIED., .F., .F.,
 ( 4, 2, 2, 2, 2, 2, 2, 2, 2, 2, 2, 2, 2, 2, 2, 2, 2, 2, 2, 2, 2, 2, 2, 2, 2, 2, 2, 2, 2, 2, 2, 2, 2, 4 ),
 ( 0.0006286237102968045840, 0.003159057492149853694, 0.004424274383076385458, 0.005689491274002918091, 0.006954708164929450723, 0.008219925055855984222, 0.009485141946782512518, 0.01075035883770904428, 0.01201557572863557605, 0.01328079261956210608, 0.01454600951048863958, 0.01581122640141517308, 0.01707644329234170311, 0.01834166018326823661, 0.01960687707419476664, 0.02087209396512130014, 0.02340252774697436366, 0.02466774463790090063, 0.02593296152882743760, 0.02656556997429069394, 0.02719817841975395722, 0.02846339531068046991, 0.02909600375614372972, 0.02972861220160698606, 0.03099382909253349874, 0.03162643753799675161, 0.03225904598346000102, 0.03352426287438650676, 0.03478947976531301250, 0.03605469665623952519, 0.03731991354716603093, 0.03858513043809252974, 0.03985034732901904242, 0.04111556421994554816 ),
 .UNSPECIFIED. ) ;
#19126 = CARTESIAN_POINT ( 'NONE',  ( 78.69119446862563905, 66.01295734309310603, -1.592560325354585915 ) ) ;
#19127 = CARTESIAN_POINT ( 'NONE',  ( -81.07947155388369254, 30.81399289130168029, -12.49999999999999645 ) ) ;
#19129 = FACE_OUTER_BOUND ( 'NONE', #37096, .T. ) ;
#19128 = CARTESIAN_POINT ( 'NONE',  ( 21.82789562172892417, 2.051186498413608561, 6.030864959255196389 ) ) ;
#19131 = ORIENTED_EDGE ( 'NONE', *, *, #4869, .T. ) ;
#19130 = ORIENTED_EDGE ( 'NONE', *, *, #32052, .F. ) ;
#19132 = CARTESIAN_POINT ( 'NONE',  ( 81.95280109346356312, 63.95510859576435081, -2.731810022748015321 ) ) ;
#19133 = VECTOR ( 'NONE', #148, 1000.000000000000000 ) ;
#19134 = CARTESIAN_POINT ( 'NONE',  ( 4.714904839365606115, -27.99744780023306134, 6.868387053540519815 ) ) ;
#19136 = CARTESIAN_POINT ( 'NONE',  ( -6.448748702180637338, -26.64985754041175525, 6.700000000000000178 ) ) ;
#19135 = CARTESIAN_POINT ( 'NONE',  ( -58.05766836353178917, 29.90785475872966259, -4.511249903221973945 ) ) ;
#19137 = DIRECTION ( 'NONE',  ( -0.000000000000000000, -0.000000000000000000, -1.000000000000000000 ) ) ;
#19138 = FACE_OUTER_BOUND ( 'NONE', #39548, .T. ) ;
#19139 = CARTESIAN_POINT ( 'NONE',  ( 69.55412262724962602, 59.60600320152340004, 3.916752429509892774 ) ) ;
#19140 = CARTESIAN_POINT ( 'NONE',  ( 22.60925884027456334, 3.558685826784935280, -4.008354383335261950 ) ) ;
#19141 = ORIENTED_EDGE ( 'NONE', *, *, #18569, .F. ) ;
#19142 = ORIENTED_EDGE ( 'NONE', *, *, #26785, .F. ) ;
#19143 = EDGE_CURVE ( 'NONE', #40099, #23269, #19463, .T. ) ;
#19144 = CARTESIAN_POINT ( 'NONE',  ( 21.85643539959776760, 9.193408351192362105, 7.099988578988766008 ) ) ;
#19145 = CARTESIAN_POINT ( 'NONE',  ( -36.87867591359218977, -26.64985754041175525, 6.800000000000000711 ) ) ;
#19146 = CARTESIAN_POINT ( 'NONE',  ( -54.79610818216033152, 31.51396769785350926, -1.000000000000000000 ) ) ;
#19147 = CARTESIAN_POINT ( 'NONE',  ( 81.58578928044241252, 61.77466459011640865, 1.878604182848663262 ) ) ;
#19148 = CARTESIAN_POINT ( 'NONE',  ( 86.17769677085827595, 1.483769024673816661, 5.380928644057212828 ) ) ;
#19149 = ORIENTED_EDGE ( 'NONE', *, *, #17560, .F. ) ;
#19150 = AXIS2_PLACEMENT_3D ( 'NONE', #8759, #15355, #12477 ) ;
#19151 = CARTESIAN_POINT ( 'NONE',  ( 0.4299795134041287659, -32.72366716650702756, 7.761597726988851420 ) ) ;
#19152 = VERTEX_POINT ( 'NONE', #38791 ) ;
#19153 = CARTESIAN_POINT ( 'NONE',  ( 21.52218790455891906, -2.808060335668637997, 3.561660395461073048 ) ) ;
#19154 = CARTESIAN_POINT ( 'NONE',  ( 36.89719978986997972, -3.002184996989889054, -5.965098407995004237 ) ) ;
#19155 = CARTESIAN_POINT ( 'NONE',  ( 5.099854031935251442, -29.63030343461936411, 7.785172627573962778 ) ) ;
#19156 = CARTESIAN_POINT ( 'NONE',  ( -80.92837670882107659, 2.429809908903242555, 12.50000000000000000 ) ) ;
#19157 = PRODUCT ( 'slotted cheese head screw_iso_ISO 1207 - M5 x 35 - 35N', 'slotted cheese head screw_iso_ISO 1207 - M5 x 35 - 35N', '', ( #7516 ) ) ;
#19158 = EDGE_CURVE ( 'NONE', #32112, #16761, #1100, .T. ) ;
#19159 = EDGE_CURVE ( 'NONE', #19681, #36032, #19957, .T. ) ;
#19160 = CARTESIAN_POINT ( 'NONE',  ( 0.5160167997142889318, -32.86344804452599533, 7.635761828346576685 ) ) ;
#19161 = ADVANCED_FACE ( 'NONE', ( #28935 ), #13689, .T. ) ;
#19162 = CARTESIAN_POINT ( 'NONE',  ( -34.34874870218063592, -26.64985754041175525, 6.700000000000000178 ) ) ;
#19163 = CARTESIAN_POINT ( 'NONE',  ( 32.01954582267668314, -3.753399427551567413, 4.807335171585498834 ) ) ;
#19164 = VERTEX_POINT ( 'NONE', #35725 ) ;
#19165 = ORIENTED_EDGE ( 'NONE', *, *, #26456, .F. ) ;
#19166 = CARTESIAN_POINT ( 'NONE',  ( 34.63535154135784211, -0.7851648049891344350, 5.278750410354886569 ) ) ;
#19167 = CARTESIAN_POINT ( 'NONE',  ( 1.712675212775339517, -33.06991241760749745, 7.756742906098588186 ) ) ;
#19168 = CARTESIAN_POINT ( 'NONE',  ( 66.41110252083150556, 57.82170748331512300, -4.000000000000026645 ) ) ;
#19169 = ORIENTED_EDGE ( 'NONE', *, *, #22150, .F. ) ;
#19170 = CARTESIAN_POINT ( 'NONE',  ( -55.16208421294562925, 31.22611435454062345, 1.446432346866579621 ) ) ;
#19171 = CARTESIAN_POINT ( 'NONE',  ( -40.24874870218063450, -26.64985754041175525, 6.700000000000000178 ) ) ;
#19172 = CARTESIAN_POINT ( 'NONE',  ( 4.957993191292200841, -28.59625817525675018, 6.997764925645181044 ) ) ;
#19173 = EDGE_CURVE ( 'NONE', #4809, #11346, #35335, .T. ) ;
#19174 = CARTESIAN_POINT ( 'NONE',  ( 2.292186059008701093, -26.12032476611858911, 7.638991368224661294 ) ) ;
#19175 = ORIENTED_EDGE ( 'NONE', *, *, #9514, .T. ) ;
#19176 = DIRECTION ( 'NONE',  ( 1.000000000000000000, 0.000000000000000000, -0.000000000000000000 ) ) ;
#19177 = CARTESIAN_POINT ( 'NONE',  ( 3.829758772512354970, -32.34767630444171971, 6.880828092187096345 ) ) ;
#19178 = ORIENTED_EDGE ( 'NONE', *, *, #3064, .F. ) ;
#19179 = CARTESIAN_POINT ( 'NONE',  ( 22.24260148052792729, 5.041501173538935454, 3.209353097046206305 ) ) ;
#19180 = CARTESIAN_POINT ( 'NONE',  ( 82.23130663822949771, 64.88126268290422161, -1.480606629406893804 ) ) ;
#19181 = CARTESIAN_POINT ( 'NONE',  ( 79.55117250774245008, 64.91534908514034896, 3.386558198656119512 ) ) ;
#19182 = CARTESIAN_POINT ( 'NONE',  ( -69.92837670882107659, -20.78299143688747819, 3.916079783099623679 ) ) ;
#19183 = ORIENTED_EDGE ( 'NONE', *, *, #40605, .F. ) ;
#19184 = CARTESIAN_POINT ( 'NONE',  ( 76.39468346684414257, 63.92226846272791363, -3.160174624570336821 ) ) ;
#19186 = CARTESIAN_POINT ( 'NONE',  ( 0.08558287364504800487, -0.6000000000000004219, 3.903552650893701514 ) ) ;
#19185 = CARTESIAN_POINT ( 'NONE',  ( -72.42837670882107659, -47.11702805680359063, 5.809475019311127753 ) ) ;
#19187 = CARTESIAN_POINT ( 'NONE',  ( 15.05162924821635251, 12.14958264902990059, -2.534429217488545216 ) ) ;
#19188 = CARTESIAN_POINT ( 'NONE',  ( 81.36407395805152021, 61.67455102447421211, -2.043563575549276479 ) ) ;
#19189 = CARTESIAN_POINT ( 'NONE',  ( 77.19967638839703739, 62.30393748795762576, 3.856837490695280923 ) ) ;
#19190 = B_SPLINE_CURVE_WITH_KNOTS ( 'NONE', 3,
 ( #15752, #34108, #28099, #123, #18419, #15335, #40653, #27496, #3233, #40436, #5882, #28305, #24402, #31007, #37759, #36960, #12455, #25024, #12245, #25230, #24819, #21937, #37361, #37561, #21323, #22148, #9568, #9356, #2812, #18836, #27687, #34511, #27889, #6287 ),
 .UNSPECIFIED., .F., .F.,
 ( 4, 2, 1, 1, 2, 2, 2, 1, 1, 2, 1, 2, 2, 1, 2, 1, 2, 2, 1, 2, 4 ),
 ( 0.8213160790108455789, 0.8227120471435722671, 0.8241080152762988442, 0.8268999515417521096, 0.8296918878072053749, 0.8300408798403869914, 0.8303898718735686080, 0.8310878559399325072, 0.8324838240726603056, 0.8436515691344798062, 0.8464435053999349590, 0.8478394735326628684, 0.8492354416653907778, 0.8548193141963014163, 0.8659870592581228044, 0.8715709317890331098, 0.8743628680544878184, 0.8771548043199426381, 0.8883225493817656915, 0.9106580395054132415, 1.000000000000000000 ),
 .UNSPECIFIED. ) ;
#19191 = ORIENTED_EDGE ( 'NONE', *, *, #3069, .F. ) ;
#19192 = VERTEX_POINT ( 'NONE', #8295 ) ;
#19193 = EDGE_CURVE ( 'NONE', #19421, #18407, #34730, .T. ) ;
#19194 = CARTESIAN_POINT ( 'NONE',  ( 1.718491058161632168, -26.07869869449652001, 7.778495531946298058 ) ) ;
#19195 = AXIS2_PLACEMENT_3D ( 'NONE', #31301, #24705, #619 ) ;
#19196 = CARTESIAN_POINT ( 'NONE',  ( -58.88327606466311437, 29.11203654247168870, 6.075279880813873490 ) ) ;
#19197 = CARTESIAN_POINT ( 'NONE',  ( 79.25820086742470494, 66.26332994521376918, 1.378120381825653551 ) ) ;
#19198 = CARTESIAN_POINT ( 'NONE',  ( 17.20447520187076762, 12.11625420413208332, 2.499999999999993339 ) ) ;
#19199 = CARTESIAN_POINT ( 'NONE',  ( 30.06379901557190237, -4.186058752285889639, 3.090730270791094636 ) ) ;
#19200 = CARTESIAN_POINT ( 'NONE',  ( -1.367092955110547514, -31.25535295005563796, 6.867280401193707640 ) ) ;
#19201 = CARTESIAN_POINT ( 'NONE',  ( -64.29080678322934261, 36.57451004496311953, 5.531098403533500907 ) ) ;
#19202 = ADVANCED_FACE ( 'NONE', ( #33461 ), #33656, .F. ) ;
#19203 = DIRECTION ( 'NONE',  ( -0.8831583674551005680, 0.4690749385695655027, 0.000000000000000000 ) ) ;
#19204 = CARTESIAN_POINT ( 'NONE',  ( -0.6017143941908295046, -32.07201138884889247, 6.871394612369935651 ) ) ;
#19205 = PLANE ( 'NONE',  #2631 ) ;
#19206 = EDGE_CURVE ( 'NONE', #32421, #10601, #8874, .T. ) ;
#19207 = CARTESIAN_POINT ( 'NONE',  ( 33.45777346496446825, -3.169730459255029054, -5.428292747153331099 ) ) ;
#19208 = CARTESIAN_POINT ( 'NONE',  ( 21.58554896752337982, 4.069564431507699531, -3.350826899357332689 ) ) ;
#19209 = DIRECTION ( 'NONE',  ( -0.000000000000000000, 0.000000000000000000, -1.000000000000000000 ) ) ;
#19210 = B_SPLINE_CURVE_WITH_KNOTS ( 'NONE', 5,
 ( #4377, #35275, #7043, #29481, #10720, #25990, #10329, #19610 ),
 .UNSPECIFIED., .F., .F.,
 ( 6, 2, 6 ),
 ( 0.000000000000000000, 0.5000000000000000000, 1.000000000000000000 ),
 .UNSPECIFIED. ) ;
#19211 = CARTESIAN_POINT ( 'NONE',  ( -0.9781255058339732855, -31.66410296430423443, 7.759451378593094084 ) ) ;
#19212 = CARTESIAN_POINT ( 'NONE',  ( 15.19569296197379238, -3.822826931744748968, -2.578053414575811608 ) ) ;
#19213 = CARTESIAN_POINT ( 'NONE',  ( -1.577774374486538678, -28.34370111728035013, 6.894806418505347700 ) ) ;
#19214 = CARTESIAN_POINT ( 'NONE',  ( -79.81169712350360612, 10.44897077626513671, 6.725963864478613274 ) ) ;
#19215 = ADVANCED_FACE ( 'NONE', ( #17765 ), #20255, .F. ) ;
#19216 = FACE_OUTER_BOUND ( 'NONE', #14395, .T. ) ;
#19217 = FACE_OUTER_BOUND ( 'NONE', #19924, .T. ) ;
#19218 = ORIENTED_EDGE ( 'NONE', *, *, #4776, .F. ) ;
#19219 = ORIENTED_EDGE ( 'NONE', *, *, #13709, .T. ) ;
#19220 = CYLINDRICAL_SURFACE ( 'NONE', #8037, 0.09010775117052882699 ) ;
#19221 = CARTESIAN_POINT ( 'NONE',  ( 68.16305384742138074, 58.02271910793402299, -3.969942683317755350 ) ) ;
#19222 = ORIENTED_EDGE ( 'NONE', *, *, #37881, .T. ) ;
#19223 = DIRECTION ( 'NONE',  ( 0.000000000000000000, 0.000000000000000000, 1.000000000000000000 ) ) ;
#19224 = CARTESIAN_POINT ( 'NONE',  ( -1.600658481268678823, -28.40671124064021669, 7.697032948437508182 ) ) ;
#19225 = CARTESIAN_POINT ( 'NONE',  ( 24.38892444693420458, 2.847891321149697230, 3.812990230678215742 ) ) ;
#19226 = CARTESIAN_POINT ( 'NONE',  ( 3.601045828089646239, -26.63095849577496566, 6.903112506833891437 ) ) ;
#19227 = AXIS2_PLACEMENT_3D ( 'NONE', #38492, #6819, #444 ) ;
#19228 = CARTESIAN_POINT ( 'NONE',  ( -1.268168650321787716, -31.22753658603060956, 6.894806418505346812 ) ) ;
#19229 = EDGE_LOOP ( 'NONE', ( #27441, #23580, #37938, #7192 ) ) ;
#19230 = CYLINDRICAL_SURFACE ( 'NONE', #18854, 0.09010775117053149152 ) ;
#19231 = CARTESIAN_POINT ( 'NONE',  ( 80.87203728266233327, 63.05930952086730201, 3.432259906339284683 ) ) ;
#19232 = VERTEX_POINT ( 'NONE', #30352 ) ;
#19233 = CYLINDRICAL_SURFACE ( 'NONE', #27191, 0.1000000000000028644 ) ;
#19234 = ORIENTED_EDGE ( 'NONE', *, *, #23641, .F. ) ;
#19235 = CARTESIAN_POINT ( 'NONE',  ( 78.95999731999182814, 64.46943033386044419, -3.516968106976288588 ) ) ;
#19236 =( BOUNDED_CURVE ( )  B_SPLINE_CURVE ( 3, ( #26936, #17857, #4908, #36208 ),
 .UNSPECIFIED., .F., .T. ) 
 B_SPLINE_CURVE_WITH_KNOTS ( ( 4, 4 ),
 ( 4.748221474220560623, 4.941946782021394924 ),
 .UNSPECIFIED. ) 
 CURVE ( )  GEOMETRIC_REPRESENTATION_ITEM ( )  RATIONAL_B_SPLINE_CURVE ( ( 1.000000000000000000, 0.9968749865767494445, 0.9968749865767494445, 1.000000000000000000 ) ) 
 REPRESENTATION_ITEM ( '' )  );
#19238 = DIRECTION ( 'NONE',  ( -0.000000000000000000, -0.000000000000000000, -1.000000000000000000 ) ) ;
#19237 = CARTESIAN_POINT ( 'NONE',  ( 24.72106036938118478, 0.6348158216212017591, 4.784554241740610614 ) ) ;
#19239 = CARTESIAN_POINT ( 'NONE',  ( 79.85781052176623973, 66.03394566247139608, -2.299173245602593507 ) ) ;
#19240 = CARTESIAN_POINT ( 'NONE',  ( 80.15282788578683437, 62.77883523856217352, 3.578491385641962452 ) ) ;
#19241 = ADVANCED_FACE ( 'NONE', ( #5432 ), #2158, .T. ) ;
#19242 = CARTESIAN_POINT ( 'NONE',  ( 82.45631153319118312, 62.87735296625318426, 1.000000000000000000 ) ) ;
#19244 = ORIENTED_EDGE ( 'NONE', *, *, #13349, .T. ) ;
#19243 = CARTESIAN_POINT ( 'NONE',  ( -64.08758708074093136, 43.90699456340107787, 1.959021792961942898 ) ) ;
#19245 = CARTESIAN_POINT ( 'NONE',  ( 22.40307219844260800, 2.196575021783337522, 8.487454310335619923 ) ) ;
#19246 = DIRECTION ( 'NONE',  ( -0.000000000000000000, -0.000000000000000000, 1.000000000000000000 ) ) ;
#19247 = EDGE_LOOP ( 'NONE', ( #23485, #8389, #39410, #14966 ) ) ;
#19248 = CARTESIAN_POINT ( 'NONE',  ( -75.48351715386579031, 8.403134493634572877, 10.29384773356716565 ) ) ;
#19249 = CARTESIAN_POINT ( 'NONE',  ( 23.58564635679343269, 0.4093974991330989188, -5.530654786722362104 ) ) ;
#19250 = EDGE_LOOP ( 'NONE', ( #38409, #10560, #16782, #40121 ) ) ;
#19251 = CARTESIAN_POINT ( 'NONE',  ( -1.543298022821887328, -28.25521066738867049, 7.750000000000000888 ) ) ;
#19252 = CARTESIAN_POINT ( 'NONE',  ( 1.697525331384263314, -32.96992897650194720, 7.769368695748486431 ) ) ;
#19253 = CARTESIAN_POINT ( 'NONE',  ( 32.89832779772925875, -3.752711978480219646, -5.048536920064313982 ) ) ;
#19254 = CARTESIAN_POINT ( 'NONE',  ( 36.87105087205511467, -2.087304334115438031, -5.864227613858936650 ) ) ;
#19255 = CARTESIAN_POINT ( 'NONE',  ( 3.821287304908778548, -32.22733399491815476, 6.870716933885664623 ) ) ;
#19256 = CARTESIAN_POINT ( 'NONE',  ( 16.45636466660662833, 9.968736736387965536, 2.757778904987983726 ) ) ;
#19257 = CARTESIAN_POINT ( 'NONE',  ( 5.195093854244484000, -29.76240288740631357, 6.961115707816230902 ) ) ;
#19258 = CARTESIAN_POINT ( 'NONE',  ( 30.67349724481533002, -3.593355625737403525, 4.777428303402127874 ) ) ;
#19259 = CARTESIAN_POINT ( 'NONE',  ( 5.150390093233091271, -29.56993018339339940, 7.750000000000000888 ) ) ;
#19260 = AXIS2_PLACEMENT_3D ( 'NONE', #37142, #25409, #15523 ) ;
#19261 = EDGE_CURVE ( 'NONE', #36144, #31580, #14678, .T. ) ;
#19262 = EDGE_CURVE ( 'NONE', #14452, #25263, #24160, .T. ) ;
#19263 = CARTESIAN_POINT ( 'NONE',  ( 1.731470216958145070, -26.07006818241261215, 6.894806418505347700 ) ) ;
#19264 = CARTESIAN_POINT ( 'NONE',  ( 21.76310852954332020, 0.8497392545002346864, -7.746649034779642840 ) ) ;
#19265 = CARTESIAN_POINT ( 'NONE',  ( 35.35174707496273072, -1.118750166776470989, -5.447475926327616236 ) ) ;
#19266 = ADVANCED_FACE ( 'NONE', ( #4823 ), #29931, .F. ) ;
#19267 = CARTESIAN_POINT ( 'NONE',  ( 1.822194502883806022, -33.27093018339341768, 7.754798119455333705 ) ) ;
#19268 = VERTEX_POINT ( 'NONE', #23751 ) ;
#19269 = CARTESIAN_POINT ( 'NONE',  ( 66.72933079118084265, 57.85140187965895819, 3.999416444359401357 ) ) ;
#19270 = B_SPLINE_CURVE_WITH_KNOTS ( 'NONE', 3,
 ( #19580, #19167, #1058, #13382, #16073, #7012, #16660, #22872, #25553, #28846, #7212, #38093, #22473, #35242, #34637, #10294, #31941, #35041, #35442 ),
 .UNSPECIFIED., .F., .F.,
 ( 4, 3, 3, 3, 3, 3, 4 ),
 ( 0.000000000000000000, 2.546128104244783067E-05, 5.711050680484007236E-05, 8.113074941675932556E-05, 0.0001053129305727076745, 0.0001360598016347103331, 0.0001612931755702044952 ),
 .UNSPECIFIED. ) ;
#19271 = FACE_OUTER_BOUND ( 'NONE', #32466, .T. ) ;
#19272 = CARTESIAN_POINT ( 'NONE',  ( 86.75210013534866960, -0.2795847087395720298, -5.842668109216860195 ) ) ;
#19273 = ORIENTED_EDGE ( 'NONE', *, *, #18786, .T. ) ;
#19274 = CARTESIAN_POINT ( 'NONE',  ( 24.75830837035764276, 3.019210359990082804, 3.350572556515618583 ) ) ;
#19275 =( LENGTH_UNIT ( ) NAMED_UNIT ( * ) SI_UNIT ( .MILLI., .METRE. ) );
#19276 = CARTESIAN_POINT ( 'NONE',  ( -75.45330471031414277, 33.71485196875532608, -8.800414904976364028 ) ) ;
#19277 = DIRECTION ( 'NONE',  ( -0.000000000000000000, 1.000000000000000000, -0.000000000000000000 ) ) ;
#19278 = EDGE_LOOP ( 'NONE', ( #12437, #24354, #23853, #8179 ) ) ;
#19279 = CARTESIAN_POINT ( 'NONE',  ( 4.017083442752244160, -26.95596097974580729, 7.776484688137382584 ) ) ;
#19280 = ORIENTED_EDGE ( 'NONE', *, *, #7898, .T. ) ;
#19281 = CARTESIAN_POINT ( 'NONE',  ( 79.70130230958179141, 64.28379252955068068, -3.649417990092605368 ) ) ;
#19282 = DIRECTION ( 'NONE',  ( -0.000000000000000000, 0.000000000000000000, 1.000000000000000000 ) ) ;
#19283 = CARTESIAN_POINT ( 'NONE',  ( 81.00792578075066785, 61.24501526813143215, 1.386845825021845835 ) ) ;
#19287 = VERTEX_POINT ( 'NONE', #19013 ) ;
#19286 = ORIENTED_EDGE ( 'NONE', *, *, #21256, .F. ) ;
#19285 = CARTESIAN_POINT ( 'NONE',  ( 38.29999999999999716, 0.000000000000000000, 2.500000000000000000 ) ) ;
#19284 = CIRCLE ( 'NONE', #25868, 0.1000000000000028644 ) ;
#19288 = CARTESIAN_POINT ( 'NONE',  ( -0.06024024948605010560, -26.54499921554088360, 7.756742906098588186 ) ) ;
#19289 = CARTESIAN_POINT ( 'NONE',  ( 27.32683644248853483, -4.450517831252136070, 3.663591729240187611 ) ) ;
#19290 = CARTESIAN_POINT ( 'NONE',  ( 21.85643539959779957, -14.30241103581959727, -6.272691714111175543 ) ) ;
#19291 = CARTESIAN_POINT ( 'NONE',  ( 22.62733628673683128, 4.569048702858772515, -3.101284368409240155 ) ) ;
#19292 = ORIENTED_EDGE ( 'NONE', *, *, #28989, .T. ) ;
#19293 = CARTESIAN_POINT ( 'NONE',  ( -63.71117060422339051, 35.77969396829408311, -7.174848616057552420 ) ) ;
#19294 = ORIENTED_EDGE ( 'NONE', *, *, #9827, .T. ) ;
#19295 = CARTESIAN_POINT ( 'NONE',  ( -1.754169330766808699, -30.13215794990895091, 6.880608371227949327 ) ) ;
#19296 = CARTESIAN_POINT ( 'NONE',  ( -0.6073368879808319631, -32.18772608075904174, 7.780491323090166667 ) ) ;
#19297 = CIRCLE ( 'NONE', #35103, 3.449999999999999734 ) ;
#19298 = CARTESIAN_POINT ( 'NONE',  ( -78.36124264143398932, -5.233282719009260120, -8.391784592071982019 ) ) ;
#19299 = CYLINDRICAL_SURFACE ( 'NONE', #35360, 10.00000000000000888 ) ;
#19300 = CARTESIAN_POINT ( 'NONE',  ( 5.137206238981461226, -30.23196853600094158, 6.875671892026062437 ) ) ;
#19301 = CARTESIAN_POINT ( 'NONE',  ( 79.06971639787835215, 65.98240043192649296, 2.069468987430128415 ) ) ;
#19302 = CARTESIAN_POINT ( 'NONE',  ( 87.65251942239244443, -2.181810347267220340, 2.926837865475490297 ) ) ;
#19303 = CARTESIAN_POINT ( 'NONE',  ( -81.07947155388369254, 30.81399289130168384, -46.17089178453873188 ) ) ;
#19304 = VERTEX_POINT ( 'NONE', #34281 ) ;
#19305 = CARTESIAN_POINT ( 'NONE',  ( -69.32837670882108227, -34.30579396504363388, 1.870248747537495149E-15 ) ) ;
#19306 = CARTESIAN_POINT ( 'NONE',  ( 4.594123659639434365, -31.35497693952491005, 7.774064877406528851 ) ) ;
#19307 = EDGE_CURVE ( 'NONE', #20724, #11501, #37527, .T. ) ;
#19308 = CARTESIAN_POINT ( 'NONE',  ( 1.711546634882549212, -26.16993837675040524, 7.775108481317162479 ) ) ;
#19309 = CARTESIAN_POINT ( 'NONE',  ( 21.52001214132182483, -3.049911746754888409, -3.476945207078641076 ) ) ;
#19310 = ADVANCED_FACE ( 'NONE', ( #6049 ), #31171, .F. ) ;
#19311 = CARTESIAN_POINT ( 'NONE',  ( 4.684314823655713944, -27.94012068505428559, 7.782034975670475418 ) ) ;
#19312 = CARTESIAN_POINT ( 'NONE',  ( -0.9997577495568453765, -27.34300195364327735, 7.660770905198786451 ) ) ;
#19313 = CARTESIAN_POINT ( 'NONE',  ( 68.63113683135277654, 58.55076364936792288, 3.993768376023898448 ) ) ;
#19314 = CARTESIAN_POINT ( 'NONE',  ( 20.42491269841142554, 3.667755154276754137, 3.394199623604145177 ) ) ;
#19315 = CARTESIAN_POINT ( 'NONE',  ( 87.97568001472090771, -0.4607347734944167716, -3.153239710520575390 ) ) ;
#19316 = VERTEX_POINT ( 'NONE', #25187 ) ;
#19318 = DIRECTION ( 'NONE',  ( -1.000000000000000000, 0.000000000000000000, 0.000000000000000000 ) ) ;
#19317 = CARTESIAN_POINT ( 'NONE',  ( 81.21077662890941440, 62.27078576854650294, -2.885071930847909805 ) ) ;
#19319 = PRODUCT_DEFINITION_SHAPE ( 'NONE', 'NONE',  #35317 ) ;
#19320 = CARTESIAN_POINT ( 'NONE',  ( -0.04165398999324298329, -32.48973880933039737, 6.894806418505347700 ) ) ;
#19321 = DIRECTION ( 'NONE',  ( 0.6662082868431827842, 0.000000000000000000, 0.7457657263118703250 ) ) ;
#19322 = ORIENTED_EDGE ( 'NONE', *, *, #37217, .F. ) ;
#19323 = CARTESIAN_POINT ( 'NONE',  ( 11.29080664838498826, -10.90558813203967148, -6.000000000000000000 ) ) ;
#19324 = ORIENTED_EDGE ( 'NONE', *, *, #910, .F. ) ;
#19325 = FACE_OUTER_BOUND ( 'NONE', #4502, .T. ) ;
#19326 = AXIS2_PLACEMENT_3D ( 'NONE', #20416, #1312, #29502 ) ;
#19327 = AXIS2_PLACEMENT_3D ( 'NONE', #9040, #15018, #5965 ) ;
#19329 = VERTEX_POINT ( 'NONE', #21287 ) ;
#19328 = ORIENTED_EDGE ( 'NONE', *, *, #35184, .T. ) ;
#19330 = CARTESIAN_POINT ( 'NONE',  ( 79.29422675899260753, 65.38839789421687954, -2.978180346930986211 ) ) ;
#19331 = CARTESIAN_POINT ( 'NONE',  ( 5.152603803343559719, -30.14631978585090621, 7.724038915126860694 ) ) ;
#19332 = ADVANCED_FACE ( 'NONE', ( #11784 ), #8707, .F. ) ;
#19333 = CARTESIAN_POINT ( 'NONE',  ( 25.64976342364274586, 1.736051923866335223, 4.267932205033374338 ) ) ;
#19335 = ORIENTED_EDGE ( 'NONE', *, *, #23077, .F. ) ;
#19334 = ORIENTED_EDGE ( 'NONE', *, *, #30824, .F. ) ;
#19336 = DIRECTION ( 'NONE',  ( 0.000000000000000000, 0.000000000000000000, 1.000000000000000000 ) ) ;
#19337 = CIRCLE ( 'NONE', #1593, 0.1000000000000028644 ) ;
#19339 = CARTESIAN_POINT ( 'NONE',  ( 86.46043323462474461, 1.241262327860113590, 4.894917242394325463 ) ) ;
#19338 = CARTESIAN_POINT ( 'NONE',  ( 4.543259257677775054, -31.43490735317836027, 7.006423389747791219 ) ) ;
#19340 = DIRECTION ( 'NONE',  ( -0.000000000000000000, -0.000000000000000000, 1.000000000000000000 ) ) ;
#19341 = CARTESIAN_POINT ( 'NONE',  ( -64.08758708074093136, 41.42070492151870553, -3.928592456684763423 ) ) ;
#19342 = CARTESIAN_POINT ( 'NONE',  ( 71.23183612236115891, 58.76351790733232860, 3.862811858476256965 ) ) ;
#19343 = CARTESIAN_POINT ( 'NONE',  ( 24.12346661364753686, 3.039791896184803832, -3.681378513681969000 ) ) ;
#19344 = ORIENTED_EDGE ( 'NONE', *, *, #16956, .T. ) ;
#19345 = CARTESIAN_POINT ( 'NONE',  ( 3.121324086407806231, -26.64985754041175525, 6.700000000000000178 ) ) ;
#19346 = ORIENTED_EDGE ( 'NONE', *, *, #8566, .F. ) ;
#19347 = EDGE_CURVE ( 'NONE', #33823, #15769, #25257, .T. ) ;
#19348 = CARTESIAN_POINT ( 'NONE',  ( 21.85643539959775339, 6.533355437427212919, 10.99619876466361212 ) ) ;
#19349 = CARTESIAN_POINT ( 'NONE',  ( 21.86297326093951199, 3.431109414793612533, 3.921173740588492329 ) ) ;
#19350 = CARTESIAN_POINT ( 'NONE',  ( -64.01189449551647215, 34.81586596186931359, -7.000000000000003553 ) ) ;
#19351 = CARTESIAN_POINT ( 'NONE',  ( 81.65270467917663666, 63.44102909743362773, 3.019969592843123607 ) ) ;
#19352 = CARTESIAN_POINT ( 'NONE',  ( 87.69705646362149309, -0.3167607505441215610, 5.204154330927820205 ) ) ;
#19353 = VERTEX_POINT ( 'NONE', #24573 ) ;
#19354 = CARTESIAN_POINT ( 'NONE',  ( 2.733375749414411082, -32.91402105668144884, 7.009310105710485850 ) ) ;
#19355 = CARTESIAN_POINT ( 'NONE',  ( 14.85462441431243796, -6.141020992384870425, 2.524821418939259932 ) ) ;
#19356 = CARTESIAN_POINT ( 'NONE',  ( 37.00353525545608591, -2.736192746824828603, 5.981694629132673136 ) ) ;
#19357 = CIRCLE ( 'NONE', #230, 0.1000000000000028644 ) ;
#19358 = CIRCLE ( 'NONE', #1608, 0.1000000000000028644 ) ;
#19359 = CARTESIAN_POINT ( 'NONE',  ( 31.44233202302301677, -3.758924007052948824, 4.692007276047764464 ) ) ;
#19360 = EDGE_CURVE ( 'NONE', #23338, #20694, #27855, .T. ) ;
#19361 = CARTESIAN_POINT ( 'NONE',  ( 25.29740619394358703, 1.738824998010557676, -4.154670075282512975 ) ) ;
#19362 = CARTESIAN_POINT ( 'NONE',  ( 14.77500745536057813, -5.175466302041957789, 2.500000552286355759 ) ) ;
#19363 = B_SPLINE_CURVE_WITH_KNOTS ( 'NONE', 3,
 ( #33942, #34358, #3278, #6543 ),
 .UNSPECIFIED., .F., .F.,
 ( 4, 4 ),
 ( 0.000000000000000000, 1.000000000000000000 ),
 .UNSPECIFIED. ) ;
#19364 = CARTESIAN_POINT ( 'NONE',  ( 0.9689046511080217083, -32.99263803653528271, 7.750000000000000888 ) ) ;
#19365 = CARTESIAN_POINT ( 'NONE',  ( -16.24874870218063450, -25.49307895267003587, 6.700000000000000178 ) ) ;
#19366 = CARTESIAN_POINT ( 'NONE',  ( 2.863609035986291573, -26.26888160889163615, 7.695279973900954751 ) ) ;
#19367 = AXIS2_PLACEMENT_3D ( 'NONE', #17500, #1906, #14426 ) ;
#19368 = FACE_OUTER_BOUND ( 'NONE', #1974, .T. ) ;
#19369 = CARTESIAN_POINT ( 'NONE',  ( 29.58564408153181091, -3.738900761003516315, 4.503399178519281065 ) ) ;
#19370 = ORIENTED_EDGE ( 'NONE', *, *, #7055, .T. ) ;
#19371 = ORIENTED_EDGE ( 'NONE', *, *, #35205, .T. ) ;
#19372 = CARTESIAN_POINT ( 'NONE',  ( 37.10400457017786380, -3.125854874071246847, 5.976292952369103517 ) ) ;
#19373 = CARTESIAN_POINT ( 'NONE',  ( -1.650274565467498622, -28.99282850696639713, 7.635761828346577573 ) ) ;
#19374 = CARTESIAN_POINT ( 'NONE',  ( 66.70283438698932343, 57.92520761901871396, -3.999543855873471276 ) ) ;
#19375 = ORIENTED_EDGE ( 'NONE', *, *, #27185, .F. ) ;
#19376 = CARTESIAN_POINT ( 'NONE',  ( -17.27251170661583402, -8.656638842136340273, 6.000000000000000000 ) ) ;
#19377 = CARTESIAN_POINT ( 'NONE',  ( 4.947902983373059449, -28.56308938330872849, 6.876076431790004939 ) ) ;
#19378 = CARTESIAN_POINT ( 'NONE',  ( 2.274434078087634870, -26.11732469660939415, 7.674970859709602244 ) ) ;
#19379 = VERTEX_POINT ( 'NONE', #12420 ) ;
#19380 = CARTESIAN_POINT ( 'NONE',  ( -27.07867591359219972, -24.55319635012989110, 6.700000000000000178 ) ) ;
#19381 = EDGE_CURVE ( 'NONE', #34269, #23464, #31372, .T. ) ;
#19382 = LINE ( 'NONE', #1070, #31131 ) ;
#19383 = ORIENTED_EDGE ( 'NONE', *, *, #8570, .F. ) ;
#19384 = CARTESIAN_POINT ( 'NONE',  ( 22.67359053832636917, 4.412626292741369305, 3.229231584030726854 ) ) ;
#19385 = CARTESIAN_POINT ( 'NONE',  ( 82.04611962119285806, 65.17642557464525055, -1.633153239555407144 ) ) ;
#19386 = CIRCLE ( 'NONE', #10805, 7.744449365083023729 ) ;
#19387 = CARTESIAN_POINT ( 'NONE',  ( 2.919807535448344815, -26.39612787360452373, 7.785172627573962778 ) ) ;
#19388 = VERTEX_POINT ( 'NONE', #24991 ) ;
#19389 = CARTESIAN_POINT ( 'NONE',  ( 75.36936014427639918, 63.22485534106652949, -3.346357594022706827 ) ) ;
#19390 = CARTESIAN_POINT ( 'NONE',  ( -1.594496203247892208, -28.38936776459798139, 7.640616322432101093 ) ) ;
#19391 = CARTESIAN_POINT ( 'NONE',  ( 16.78263025183486334, 9.614103373516703854, -2.806744980977545101 ) ) ;
#19392 = EDGE_CURVE ( 'NONE', #24473, #4930, #6251, .T. ) ;
#19393 = CARTESIAN_POINT ( 'NONE',  ( 80.63945418285945266, 64.43655742540512676, -3.486376426170564979 ) ) ;
#19394 = CARTESIAN_POINT ( 'NONE',  ( 77.74497067125921035, 61.15868661831857622, 3.539370024157653116 ) ) ;
#19395 = ORIENTED_EDGE ( 'NONE', *, *, #17179, .F. ) ;
#19396 = ADVANCED_FACE ( 'NONE', ( #24784 ), #18798, .F. ) ;
#19397 = VECTOR ( 'NONE', #13389, 1000.000000000000000 ) ;
#19398 = FACE_OUTER_BOUND ( 'NONE', #28429, .T. ) ;
#19399 = CARTESIAN_POINT ( 'NONE',  ( -4.444218661349752963, -35.94265729135299381, -2.500000000000000000 ) ) ;
#19400 = CARTESIAN_POINT ( 'NONE',  ( 80.36115181822172815, 66.02274906846037084, 2.190303691588294743 ) ) ;
#19402 = CARTESIAN_POINT ( 'NONE',  ( 21.85642290860490888, 10.16974183911659146, 2.500000000000000444 ) ) ;
#19401 = CARTESIAN_POINT ( 'NONE',  ( -0.1660129358314331172, -32.53077879159856423, 6.870724624169668004 ) ) ;
#19403 = CARTESIAN_POINT ( 'NONE',  ( 29.35164812155991854, -2.438811642646435018, -5.575705495130315548 ) ) ;
#19404 = CARTESIAN_POINT ( 'NONE',  ( -1.699457623340715040, -29.60210943304089071, 7.721096864323900633 ) ) ;
#19405 = CARTESIAN_POINT ( 'NONE',  ( 3.554655459890166735, -26.72005913740336069, 6.887945620086118659 ) ) ;
#19406 = CARTESIAN_POINT ( 'NONE',  ( -0.06129048428309483154, -26.54561512989744188, 7.635761828346575797 ) ) ;
#19407 = CARTESIAN_POINT ( 'NONE',  ( 2.322191688357494677, -25.34207446254166385, 7.754798119455333705 ) ) ;
#19408 = CARTESIAN_POINT ( 'NONE',  ( 77.27679392923256785, 60.01025453254077036, 2.873255474974654167 ) ) ;
#19409 = CARTESIAN_POINT ( 'NONE',  ( -31.07867591359219617, -26.64985754041175525, 6.800000000000000711 ) ) ;
#19410 = EDGE_CURVE ( 'NONE', #11154, #23165, #18386, .T. ) ;
#19411 = CARTESIAN_POINT ( 'NONE',  ( 36.58899555212334320, -2.079458374954772815, -5.884079940498502914 ) ) ;
#19412 = CARTESIAN_POINT ( 'NONE',  ( 11.65737507970504616, -38.28842912540938670, 6.000000000000000000 ) ) ;
#19413 = DIRECTION ( 'NONE',  ( 1.000000000000000000, -2.973811673103098158E-15, 0.000000000000000000 ) ) ;
#19414 = CARTESIAN_POINT ( 'NONE',  ( 1.686887486498408029, -26.16995699532097319, 7.635761828346577573 ) ) ;
#19415 = CYLINDRICAL_SURFACE ( 'NONE', #5072, 24.28220113893567600 ) ;
#19416 = VECTOR ( 'NONE', #36023, 1000.000000000000000 ) ;
#19417 = CARTESIAN_POINT ( 'NONE',  ( -30.87867591359218977, -24.55319635012989110, 6.700000000000000178 ) ) ;
#19418 = VECTOR ( 'NONE', #10651, 1000.000000000000000 ) ;
#19419 = CARTESIAN_POINT ( 'NONE',  ( 31.82339877122853622, -2.965063844033737794, 5.173209048694666023 ) ) ;
#19421 = VERTEX_POINT ( 'NONE', #12621 ) ;
#19420 = VECTOR ( 'NONE', #8912, 1000.000000000000227 ) ;
#19422 = DIRECTION ( 'NONE',  ( 0.000000000000000000, 0.000000000000000000, 1.000000000000000000 ) ) ;
#19423 = CARTESIAN_POINT ( 'NONE',  ( 67.82906190410768943, 58.02404379074640417, -3.985511447369935123 ) ) ;
#19424 = EDGE_CURVE ( 'NONE', #18044, #28636, #37328, .T. ) ;
#19425 = EDGE_LOOP ( 'NONE', ( #28802, #16477, #29845, #7089 ) ) ;
#19426 = CARTESIAN_POINT ( 'NONE',  ( -0.9479511760676456733, -27.30154873620575984, 7.783750581861600182 ) ) ;
#19427 = CARTESIAN_POINT ( 'NONE',  ( 30.84556462519947218, -3.521365950626897945, 4.867246454883694007 ) ) ;
#19428 = CARTESIAN_POINT ( 'NONE',  ( 22.01069687017167098, 4.352078338492005649, 3.948474219383390160 ) ) ;
#19429 = CARTESIAN_POINT ( 'NONE',  ( 1.074608721727911442, -26.22801491291194864, 7.695279973900954751 ) ) ;
#19430 = CARTESIAN_POINT ( 'NONE',  ( 1.165751748339587168, -26.11099046226085107, 6.867280401193707640 ) ) ;
#19431 = EDGE_LOOP ( 'NONE', ( #28117, #36587, #6896, #14943, #15026 ) ) ;
#19432 = CARTESIAN_POINT ( 'NONE',  ( 24.75501771239566295, 3.017875978853254093, 3.356962914366536488 ) ) ;
#19433 = CARTESIAN_POINT ( 'NONE',  ( 5.698101969243359655, -32.85371976261941285, 7.695279973900954751 ) ) ;
#19434 = CARTESIAN_POINT ( 'NONE',  ( 81.24801795318221309, 61.46771992710468169, 1.817988788077155249 ) ) ;
#19435 = CARTESIAN_POINT ( 'NONE',  ( -0.9807834779648342272, -31.66069757387703731, 7.754798119455333705 ) ) ;
#19436 = ORIENTED_EDGE ( 'NONE', *, *, #6441, .T. ) ;
#19437 = CARTESIAN_POINT ( 'NONE',  ( 79.45360044721715553, 62.79974527947164376, -3.729426069516725839 ) ) ;
#19439 = CARTESIAN_POINT ( 'NONE',  ( -1.489921458977837565, -30.74547780039133116, 7.635761828346577573 ) ) ;
#19438 = CARTESIAN_POINT ( 'NONE',  ( 24.74336839167079205, 0.5919242770734765013, 4.777722238485932138 ) ) ;
#19440 = EDGE_CURVE ( 'NONE', #3076, #28543, #30771, .T. ) ;
#19441 = CARTESIAN_POINT ( 'NONE',  ( 81.60486409339017655, 61.94451848016240092, -2.198649373785569239 ) ) ;
#19442 = CARTESIAN_POINT ( 'NONE',  ( 79.21623058866053668, 63.63573840405092596, 3.765547211956732809 ) ) ;
#19443 = EDGE_CURVE ( 'NONE', #20708, #12131, #10841, .T. ) ;
#19444 = CIRCLE ( 'NONE', #1698, 10.00000000000000533 ) ;
#19445 = DIRECTION ( 'NONE',  ( -0.000000000000000000, -1.000000000000000000, -0.000000000000000000 ) ) ;
#19446 = VECTOR ( 'NONE', #14198, 1000.000000000000000 ) ;
#19447 = CARTESIAN_POINT ( 'NONE',  ( 82.10909544300281482, 65.20937546977818045, 1.165579324820864571 ) ) ;
#19448 = CARTESIAN_POINT ( 'NONE',  ( -64.08758708074093136, 43.61223004741322740, 1.000000000000000000 ) ) ;
#19449 = CARTESIAN_POINT ( 'NONE',  ( 25.48218379196744721, -4.266488024150952185, 3.117641769822204090 ) ) ;
#19450 = CARTESIAN_POINT ( 'NONE',  ( -24.97867591359219475, -24.55319635012989110, 6.700000000000000178 ) ) ;
#19451 = ORIENTED_EDGE ( 'NONE', *, *, #27615, .T. ) ;
#19452 = CARTESIAN_POINT ( 'NONE',  ( -77.08826645590907845, -4.719337535992750077, 7.895626637436674145 ) ) ;
#19453 = CARTESIAN_POINT ( 'NONE',  ( 25.40538259160478063, 0.6392885239908961958, -4.601632460917159051 ) ) ;
#19454 = ORIENTED_EDGE ( 'NONE', *, *, #21772, .F. ) ;
#19455 = AXIS2_PLACEMENT_3D ( 'NONE', #36775, #24423, #27514 ) ;
#19456 = DIRECTION ( 'NONE',  ( 0.000000000000000000, 1.000000000000000000, 0.000000000000000000 ) ) ;
#19457 = DIRECTION ( 'NONE',  ( -1.000000000000000000, 0.000000000000000000, 0.000000000000000000 ) ) ;
#19458 = CARTESIAN_POINT ( 'NONE',  ( 30.71159473002022722, -3.512327092394234018, -4.877982841742380948 ) ) ;
#19459 = CARTESIAN_POINT ( 'NONE',  ( 27.81689091006495218, 1.845377269578770685, -3.904318808813068920 ) ) ;
#19460 = CARTESIAN_POINT ( 'NONE',  ( -44.23414840393349579, -23.60493063168010153, 6.800000000000000711 ) ) ;
#19461 = CARTESIAN_POINT ( 'NONE',  ( 17.69936654701060874, 8.505593641349619816, 2.968812229095278088 ) ) ;
#19462 = CARTESIAN_POINT ( 'NONE',  ( 5.195651087393625467, -29.75204319633411743, 6.912143950357338085 ) ) ;
#19463 = B_SPLINE_CURVE_WITH_KNOTS ( 'NONE', 3,
 ( #22367, #7301, #9985, #32433 ),
 .UNSPECIFIED., .F., .F.,
 ( 4, 4 ),
 ( 1.084202172485504434E-19, 6.391136169993539061E-06 ),
 .UNSPECIFIED. ) ;
#19464 = CARTESIAN_POINT ( 'NONE',  ( -0.5741452863692977360, -26.90976311966657164, 7.670465701733756525 ) ) ;
#19465 = CARTESIAN_POINT ( 'NONE',  ( 3.465471057152984091, -32.59226193070500699, 7.750000000000000000 ) ) ;
#19466 = B_SPLINE_CURVE_WITH_KNOTS ( 'NONE', 3,
 ( #3564, #13005, #15476, #19186, #28038, #5817 ),
 .UNSPECIFIED., .F., .F.,
 ( 4, 2, 4 ),
 ( 0.0002675702395149656557, 0.0004161762349008431153, 0.0005647822302867205749 ),
 .UNSPECIFIED. ) ;
#19467 = CARTESIAN_POINT ( 'NONE',  ( -8.878675913592189772, -26.64985754041175525, 6.700000000000000178 ) ) ;
#19468 = CARTESIAN_POINT ( 'NONE',  ( 22.22682478162485964, 0.9416584759426780415, -6.596347691557129522 ) ) ;
#19469 = CARTESIAN_POINT ( 'NONE',  ( 29.51225972876092740, 1.208032713357963361, -4.232904474717664733 ) ) ;
#19470 = DIRECTION ( 'NONE',  ( 1.000000000000000000, 0.000000000000000000, 0.000000000000000000 ) ) ;
#19471 = ORIENTED_EDGE ( 'NONE', *, *, #8449, .T. ) ;
#19472 = CARTESIAN_POINT ( 'NONE',  ( 66.55613647995218685, 57.87265654107390844, 3.999745625243888547 ) ) ;
#19473 = CIRCLE ( 'NONE', #23402, 0.1000000000000028644 ) ;
#19474 = CARTESIAN_POINT ( 'NONE',  ( -2.878675913592191993, -24.55319635012989110, 6.700000000000000178 ) ) ;
#19475 = AXIS2_PLACEMENT_3D ( 'NONE', #34396, #12331, #22434 ) ;
#19476 = CARTESIAN_POINT ( 'NONE',  ( 85.51010218477300384, 1.603708918324822541, 5.381112834985590787 ) ) ;
#19477 = CYLINDRICAL_SURFACE ( 'NONE', #5750, 0.09010775117052950700 ) ;
#19478 =( BOUNDED_CURVE ( )  B_SPLINE_CURVE ( 3, ( #39136, #29086, #17108, #3989 ),
 .UNSPECIFIED., .F., .T. ) 
 B_SPLINE_CURVE_WITH_KNOTS ( ( 4, 4 ),
 ( 1.347909859412854017, 1.534781240595298746 ),
 .UNSPECIFIED. ) 
 CURVE ( )  GEOMETRIC_REPRESENTATION_ITEM ( )  RATIONAL_B_SPLINE_CURVE ( ( 1.000000000000000000, 0.9970920404276226723, 0.9970920404276226723, 1.000000000000000000 ) ) 
 REPRESENTATION_ITEM ( '' )  );
#19479 = EDGE_LOOP ( 'NONE', ( #12303, #30789, #27996, #34702 ) ) ;
#19480 = CARTESIAN_POINT ( 'NONE',  ( -79.30159439629763085, 10.34987115379732536, -7.377286748778528747 ) ) ;
#19481 = EDGE_CURVE ( 'NONE', #19773, #33743, #27654, .T. ) ;
#19482 = VECTOR ( 'NONE', #32624, 1000.000000000000000 ) ;
#19483 = CARTESIAN_POINT ( 'NONE',  ( 2.999143718241246148, -26.32260591150095763, 7.766640943994346458 ) ) ;
#19484 = DIRECTION ( 'NONE',  ( -0.000000000000000000, -0.000000000000000000, -1.000000000000000000 ) ) ;
#19485 = EDGE_LOOP ( 'NONE', ( #32163, #12571, #10101, #32214 ) ) ;
#19486 = CARTESIAN_POINT ( 'NONE',  ( -54.01549048184568846, -30.38627270959228710, 6.000000000000000000 ) ) ;
#19487 = EDGE_CURVE ( 'NONE', #16824, #2431, #11993, .T. ) ;
#19488 = ORIENTED_EDGE ( 'NONE', *, *, #3107, .F. ) ;
#19489 = CARTESIAN_POINT ( 'NONE',  ( 79.55161461803720613, 64.54397228415257359, -3.537885823842634725 ) ) ;
#19490 = CARTESIAN_POINT ( 'NONE',  ( -1.722492012567419239, -28.86192695835683253, 7.771081512783704071 ) ) ;
#19491 = CARTESIAN_POINT ( 'NONE',  ( 80.97051285240280549, 61.23143294393114644, 1.429680343938458664 ) ) ;
#19493 = EDGE_LOOP ( 'NONE', ( #34215, #4152, #2326, #31087 ) ) ;
#19492 = CARTESIAN_POINT ( 'NONE',  ( -1.699260392630454364, -29.52118006577551412, 6.894806418505346812 ) ) ;
#19494 = ADVANCED_FACE ( 'NONE', ( #34072 ), #30971, .T. ) ;
#19496 = EDGE_CURVE ( 'NONE', #2944, #39282, #12211, .T. ) ;
#19495 = CARTESIAN_POINT ( 'NONE',  ( 21.85643539959776760, 1.710603452083953179E-15, 2.500000000000000000 ) ) ;
#19497 = CARTESIAN_POINT ( 'NONE',  ( -0.5217428287191434588, -32.27402435476302145, 7.698786668945014178 ) ) ;
#19498 = DIRECTION ( 'NONE',  ( 0.8660254037844380415, 0.5000000000000009992, -0.000000000000000000 ) ) ;
#19499 = CARTESIAN_POINT ( 'NONE',  ( 33.87825334127423815, -5.339472581715918764, -1.692052827146944605 ) ) ;
#19500 = CARTESIAN_POINT ( 'NONE',  ( 24.39586660158147779, 3.158670939509748976, -3.293463392983651872 ) ) ;
#19501 = EDGE_LOOP ( 'NONE', ( #21829, #21526, #35715, #14050 ) ) ;
#19502 = CARTESIAN_POINT ( 'NONE',  ( -69.92837670882107659, -20.78299143688747819, 9.949874371066202983 ) ) ;
#19503 = EDGE_LOOP ( 'NONE', ( #25072, #10003, #3710, #12963 ) ) ;
#19504 = DIRECTION ( 'NONE',  ( -0.7660444431189725734, -0.6427876096865456912, -0.000000000000000000 ) ) ;
#19505 = DIRECTION ( 'NONE',  ( -0.9616058754224561245, 0.2744342186262705430, 0.000000000000000000 ) ) ;
#19506 = CARTESIAN_POINT ( 'NONE',  ( -73.12711914256941270, 0.2882157670163680852, -9.814792072719024318 ) ) ;
#19507 = CARTESIAN_POINT ( 'NONE',  ( 4.713418716757639793, -27.78901510573760092, 7.700536657684214248 ) ) ;
#19508 = CARTESIAN_POINT ( 'NONE',  ( -2.697268050091675118E-17, 3.729367930467589076, -6.000000000000000000 ) ) ;
#19509 = CARTESIAN_POINT ( 'NONE',  ( 80.17140661427384885, 64.93185644258201705, 3.352621494407050484 ) ) ;
#19510 = CARTESIAN_POINT ( 'NONE',  ( 87.32347380307142259, -1.421525632644524251, -4.720772940814831564 ) ) ;
#19511 = CARTESIAN_POINT ( 'NONE',  ( -0.02702267027603847890, -32.61394955640600557, 7.737115613922536106 ) ) ;
#19512 = CARTESIAN_POINT ( 'NONE',  ( -1.579542791844172900, -30.79142478763816371, 7.737115613922529000 ) ) ;
#19513 = CARTESIAN_POINT ( 'NONE',  ( -12.87867591359218977, -26.64985754041175525, 6.800000000000000711 ) ) ;
#19514 = CARTESIAN_POINT ( 'NONE',  ( 1.668210843585588687, -26.17008246681959349, 7.721096864323904185 ) ) ;
#19515 = CARTESIAN_POINT ( 'NONE',  ( 14.91179222114675085, 11.91032444678283575, -2.533743837804387056 ) ) ;
#19516 = CARTESIAN_POINT ( 'NONE',  ( -34.87867591359218977, -24.55319635012989110, 6.700000000000000178 ) ) ;
#19517 = DIRECTION ( 'NONE',  ( -0.6427876096865327016, -0.7660444431189835646, -0.000000000000000000 ) ) ;
#19518 = CARTESIAN_POINT ( 'NONE',  ( 68.74365607523500898, 58.25355655637604713, 3.970924506823473532 ) ) ;
#19519 = CARTESIAN_POINT ( 'NONE',  ( 37.04629652946467644, -2.800754724101123472, 5.988368560126969165 ) ) ;
#19520 = CARTESIAN_POINT ( 'NONE',  ( -0.4487487021806388365, -26.64985754041175525, 6.700000000000000178 ) ) ;
#19521 = EDGE_CURVE ( 'NONE', #10099, #36832, #21387, .T. ) ;
#19522 = CARTESIAN_POINT ( 'NONE',  ( 87.43837438447430088, 0.1427924124619655843, -4.444214939316114332 ) ) ;
#19523 = VERTEX_POINT ( 'NONE', #23112 ) ;
#19525 = CYLINDRICAL_SURFACE ( 'NONE', #16506, 0.1000000000000028644 ) ;
#19524 = CARTESIAN_POINT ( 'NONE',  ( 79.00945943828583040, 65.94065490460722856, -2.112861953993757425 ) ) ;
#19526 = CARTESIAN_POINT ( 'NONE',  ( -1.343377678608602688, -31.26794527077870356, 7.785344483711591934 ) ) ;
#19527 = CARTESIAN_POINT ( 'NONE',  ( -62.92837670882106238, -23.80776546975053520, 6.000000000000000000 ) ) ;
#19528 = VERTEX_POINT ( 'NONE', #13635 ) ;
#19529 = CARTESIAN_POINT ( 'NONE',  ( 21.71185578408363881, 6.328645931448866335, 3.192210964217056191 ) ) ;
#19530 = ORIENTED_EDGE ( 'NONE', *, *, #8857, .T. ) ;
#19531 = CYLINDRICAL_SURFACE ( 'NONE', #9689, 0.09010775117052841066 ) ;
#19532 = CIRCLE ( 'NONE', #38585, 2.500000000000002220 ) ;
#19533 = ORIENTED_EDGE ( 'NONE', *, *, #36136, .F. ) ;
#19534 = CARTESIAN_POINT ( 'NONE',  ( 79.60112097352363492, 64.95058993122677293, -3.372125408468116703 ) ) ;
#19535 = VECTOR ( 'NONE', #36536, 1000.000000000000000 ) ;
#19536 = CARTESIAN_POINT ( 'NONE',  ( -71.43233049654038780, 0.09072970090432713741, 5.980030958859732237 ) ) ;
#19537 = AXIS2_PLACEMENT_3D ( 'NONE', #26306, #10634, #26702 ) ;
#19538 = CARTESIAN_POINT ( 'NONE',  ( 22.99368205116111241, 2.291004117675890850, 4.722746232393920884 ) ) ;
#19540 = ORIENTED_EDGE ( 'NONE', *, *, #404, .T. ) ;
#19539 = EDGE_LOOP ( 'NONE', ( #13805, #18344, #30820, #33016 ) ) ;
#19541 = VECTOR ( 'NONE', #18904, 1000.000000000000000 ) ;
#19542 = ADVANCED_FACE ( 'NONE', ( #38533 ), #35479, .F. ) ;
#19543 = B_SPLINE_CURVE_WITH_KNOTS ( 'NONE', 3,
 ( #13610, #1078, #6834, #38311, #38716, #16490, #28862 ),
 .UNSPECIFIED., .F., .F.,
 ( 4, 3, 4 ),
 ( 0.006904927062942190462, 0.007395461772899653008, 0.008026723377514808841 ),
 .UNSPECIFIED. ) ;
#19544 = DIRECTION ( 'NONE',  ( -0.000000000000000000, -0.000000000000000000, 1.000000000000000000 ) ) ;
#19545 = ADVANCED_FACE ( 'NONE', ( #31987 ), #889, .F. ) ;
#19547 = EDGE_CURVE ( 'NONE', #17567, #26935, #34895, .T. ) ;
#19546 = FACE_OUTER_BOUND ( 'NONE', #31884, .T. ) ;
#19549 = CARTESIAN_POINT ( 'NONE',  ( 2.921324086407800280, -24.55319635012989110, 6.700000000000000178 ) ) ;
#19548 = CARTESIAN_POINT ( 'NONE',  ( 4.534632712474313543, -31.44797946402438171, 6.969307238440503482 ) ) ;
#19550 = DIRECTION ( 'NONE',  ( 0.000000000000000000, 0.000000000000000000, 1.000000000000000000 ) ) ;
#19551 = CARTESIAN_POINT ( 'NONE',  ( -63.70768058868310391, 44.39675795731058372, -0.9999999999999904521 ) ) ;
#19552 = CARTESIAN_POINT ( 'NONE',  ( 71.91282362819097784, 60.38839763785598080, 3.929231508849752252 ) ) ;
#19553 = ORIENTED_EDGE ( 'NONE', *, *, #35580, .T. ) ;
#19554 = CARTESIAN_POINT ( 'NONE',  ( 22.60213147365925934, 3.631766662821214187, -3.957887780529531163 ) ) ;
#19555 = ORIENTED_EDGE ( 'NONE', *, *, #19977, .F. ) ;
#19556 = CARTESIAN_POINT ( 'NONE',  ( -38.87867591359218977, -26.64985754041175525, 6.700000000000000178 ) ) ;
#19557 = ORIENTED_EDGE ( 'NONE', *, *, #28469, .F. ) ;
#19558 = CARTESIAN_POINT ( 'NONE',  ( 21.85643539959774628, 5.695295784951009743, -9.764639101464164028 ) ) ;
#19559 = CARTESIAN_POINT ( 'NONE',  ( 21.88804895127840311, 3.976982562632499274, 2.124131737554133537 ) ) ;
#19560 = CARTESIAN_POINT ( 'NONE',  ( 0.3842138451641537999, -32.70485417806369810, 6.876076431790004939 ) ) ;
#19561 = CARTESIAN_POINT ( 'NONE',  ( 81.74528107327201099, 62.23958694028463867, 2.368810654844612174 ) ) ;
#19562 = CARTESIAN_POINT ( 'NONE',  ( 87.20660408302002509, 0.2574974038930863407, -5.635807106906071340 ) ) ;
#19563 = ORIENTED_EDGE ( 'NONE', *, *, #26058, .T. ) ;
#19564 = CARTESIAN_POINT ( 'NONE',  ( 0.4621924864893861007, -32.73646653789152339, 7.782034975670476307 ) ) ;
#19565 = CARTESIAN_POINT ( 'NONE',  ( 15.53358838639597650, -3.613270961124078973, 2.630790167588612949 ) ) ;
#19566 = CARTESIAN_POINT ( 'NONE',  ( 37.02143117275709727, -2.763783248133810044, 5.984487719841893316 ) ) ;
#19567 = CARTESIAN_POINT ( 'NONE',  ( 5.077611659191977544, -29.17698428640678543, 6.911401339314954484 ) ) ;
#19568 = CARTESIAN_POINT ( 'NONE',  ( 36.63324149830979337, -3.079498397735149329, -5.923901332741634995 ) ) ;
#19569 = CARTESIAN_POINT ( 'NONE',  ( 5.150898290942641289, -29.04796049306044026, 7.780491323090170219 ) ) ;
#19570 = DIRECTION ( 'NONE',  ( 0.000000000000000000, 1.000000000000000000, 0.000000000000000000 ) ) ;
#19571 = VECTOR ( 'NONE', #36736, 1000.000000000000000 ) ;
#19572 = CARTESIAN_POINT ( 'NONE',  ( -73.07498068578524908, 39.58105274722134226, -12.49999999999999645 ) ) ;
#19573 = CARTESIAN_POINT ( 'NONE',  ( 2.887256171390399029, -32.85664523690996219, 7.773839561854631874 ) ) ;
#19574 = CIRCLE ( 'NONE', #18227, 0.1000000000000028644 ) ;
#19575 = CARTESIAN_POINT ( 'NONE',  ( -28.24874870218063805, -25.49307895267003587, 6.700000000000000178 ) ) ;
#19576 = CARTESIAN_POINT ( 'NONE',  ( 32.88849341148151240, -3.409024750725885955, 5.320318896896437444 ) ) ;
#19577 = ORIENTED_EDGE ( 'NONE', *, *, #38192, .T. ) ;
#19578 = EDGE_LOOP ( 'NONE', ( #28395, #39374, #6189, #12247 ) ) ;
#19579 = CARTESIAN_POINT ( 'NONE',  ( 25.73329116135044003, 2.636594892696300541, 3.521394832687038789 ) ) ;
#19580 = CARTESIAN_POINT ( 'NONE',  ( 1.717829174068238984, -33.06988673718940674, 7.750000000000000888 ) ) ;
#19581 = CARTESIAN_POINT ( 'NONE',  ( 66.58353442343859285, 57.79581178809598896, -3.999616584010542208 ) ) ;
#19582 = VERTEX_POINT ( 'NONE', #6661 ) ;
#19583 = FACE_OUTER_BOUND ( 'NONE', #18546, .T. ) ;
#19584 = CARTESIAN_POINT ( 'NONE',  ( 86.00054146471580907, 0.2529338399765344580, 5.999804812770356932 ) ) ;
#19585 = CARTESIAN_POINT ( 'NONE',  ( 2.285976816415960400, -26.11925954147043072, 7.646866513072557048 ) ) ;
#19586 = AXIS2_PLACEMENT_3D ( 'NONE', #13301, #23385, #10809 ) ;
#19587 = ORIENTED_EDGE ( 'NONE', *, *, #24736, .T. ) ;
#19588 = FACE_BOUND ( 'NONE', #8657, .T. ) ;
#19589 = PLANE ( 'NONE',  #33092 ) ;
#19590 = VERTEX_POINT ( 'NONE', #281 ) ;
#19591 = CARTESIAN_POINT ( 'NONE',  ( 82.04814969336703712, 64.78574761690806838, -2.164558651854042282 ) ) ;
#19592 = VECTOR ( 'NONE', #17386, 1000.000000000000000 ) ;
#19594 = EDGE_CURVE ( 'NONE', #32703, #1854, #12819, .T. ) ;
#19593 = CARTESIAN_POINT ( 'NONE',  ( 1.079328522417935421, -26.12547340107537863, 7.635761828346579350 ) ) ;
#19595 = VERTEX_POINT ( 'NONE', #19213 ) ;
#19596 = CARTESIAN_POINT ( 'NONE',  ( 76.07689452438883393, 60.24265224227303150, -3.527522301306114105 ) ) ;
#19597 =( BOUNDED_CURVE ( )  B_SPLINE_CURVE ( 3, ( #2173, #5655, #27067, #21509 ),
 .UNSPECIFIED., .F., .F. ) 
 B_SPLINE_CURVE_WITH_KNOTS ( ( 4, 4 ),
 ( 4.748221474220558846, 4.941946782021393147 ),
 .UNSPECIFIED. ) 
 CURVE ( )  GEOMETRIC_REPRESENTATION_ITEM ( )  RATIONAL_B_SPLINE_CURVE ( ( 1.000000000000000000, 0.9968749865767494445, 0.9968749865767494445, 1.000000000000000000 ) ) 
 REPRESENTATION_ITEM ( '' )  );
#19599 = CARTESIAN_POINT ( 'NONE',  ( 4.458039033310292609, -27.41499233908904287, 7.754798119455333705 ) ) ;
#19598 = DIRECTION ( 'NONE',  ( 1.000000000000000000, 0.000000000000000000, 0.000000000000000000 ) ) ;
#19600 = CARTESIAN_POINT ( 'NONE',  ( -70.79764455194573713, 0.2168280239975503842, 5.999999999999999112 ) ) ;
#19601 = CARTESIAN_POINT ( 'NONE',  ( 75.88202180556031351, 63.57356190189720735, 3.253266109296548247 ) ) ;
#19602 = AXIS2_PLACEMENT_3D ( 'NONE', #11681, #24257, #39695 ) ;
#19603 = PLANE ( 'NONE',  #22818 ) ;
#19604 = DIRECTION ( 'NONE',  ( 0.6502177225477889788, 0.3754033771448354040, 0.6605219282605379050 ) ) ;
#19605 = DIRECTION ( 'NONE',  ( -0.000000000000000000, -0.000000000000000000, 1.000000000000000000 ) ) ;
#19606 = CARTESIAN_POINT ( 'NONE',  ( 82.15073535245181802, 63.33429545135121685, 2.460680857248572551 ) ) ;
#19607 = CARTESIAN_POINT ( 'NONE',  ( 86.80434382515846892, 0.8549656295913086179, -5.002690157204635391 ) ) ;
#19608 = CARTESIAN_POINT ( 'NONE',  ( 29.92651255597534288, -3.613225851372795727, -4.302012675596341928 ) ) ;
#19609 = CARTESIAN_POINT ( 'NONE',  ( 2.301779523252329263, -26.22352920515988828, 7.775108481317162479 ) ) ;
#19610 = CARTESIAN_POINT ( 'NONE',  ( 33.89725028478159174, -5.465908938576614418, 0.4877600842561391481 ) ) ;
#19611 = CARTESIAN_POINT ( 'NONE',  ( 11.29080664838499182, -35.94265729135299381, 6.000000000000000000 ) ) ;
#19612 = ORIENTED_EDGE ( 'NONE', *, *, #4839, .F. ) ;
#19613 = DIRECTION ( 'NONE',  ( 0.000000000000000000, 0.000000000000000000, 1.000000000000000000 ) ) ;
#19614 = FACE_OUTER_BOUND ( 'NONE', #14468, .T. ) ;
#19615 = CARTESIAN_POINT ( 'NONE',  ( 36.46007995281161129, -3.391394755346535117, -5.869938052945382623 ) ) ;
#19616 = DIRECTION ( 'NONE',  ( -0.000000000000000000, -0.000000000000000000, -1.000000000000000000 ) ) ;
#19617 = CARTESIAN_POINT ( 'NONE',  ( 6.029691375358208205, -29.61640541118720193, 6.954324564059724878 ) ) ;
#19618 = CIRCLE ( 'NONE', #19586, 1.000000000000003109 ) ;
#19619 = DIRECTION ( 'NONE',  ( 0.000000000000000000, -0.7541618601367526820, -0.6566885781822866530 ) ) ;
#19620 = CARTESIAN_POINT ( 'NONE',  ( -69.32837670882108227, -34.30579396504363388, 1.870248747537495149E-15 ) ) ;
#19621 = EDGE_CURVE ( 'NONE', #15830, #9639, #22045, .T. ) ;
#19622 = CARTESIAN_POINT ( 'NONE',  ( 22.03648680630582746, -11.51106657129999356, -2.500000000000000000 ) ) ;
#19623 = CARTESIAN_POINT ( 'NONE',  ( -1.493583877073865862, -28.40437011329764871, 7.769368695748486431 ) ) ;
#19624 = ORIENTED_EDGE ( 'NONE', *, *, #20377, .F. ) ;
#19625 = CARTESIAN_POINT ( 'NONE',  ( 2.410368835147195021, -26.24488429107400478, 7.754798119455333705 ) ) ;
#19626 = CARTESIAN_POINT ( 'NONE',  ( 68.72765198451649837, 58.29585788764496357, -3.976359261632543163 ) ) ;
#19627 = VECTOR ( 'NONE', #28520, 1000.000000000000000 ) ;
#19628 = CARTESIAN_POINT ( 'NONE',  ( 3.069849883003687552, -26.34896937748550272, 6.989977667959442975 ) ) ;
#19629 = EDGE_CURVE ( 'NONE', #29197, #24455, #28002, .T. ) ;
#19630 = ORIENTED_EDGE ( 'NONE', *, *, #18441, .F. ) ;
#19631 = CARTESIAN_POINT ( 'NONE',  ( -1.391746016950013320, -31.20965402480746320, 7.750000000000000888 ) ) ;
#19632 = CARTESIAN_POINT ( 'NONE',  ( -2.878675913592191993, -24.55319635012989110, 6.800000000000000711 ) ) ;
#19633 = CARTESIAN_POINT ( 'NONE',  ( 24.36285579537860357, 2.875202204253215044, 3.793786480169491604 ) ) ;
#19634 = CARTESIAN_POINT ( 'NONE',  ( 0.4754575822783353445, -26.29127984263010731, 7.660770905198778458 ) ) ;
#19635 = CARTESIAN_POINT ( 'NONE',  ( 1.130236063958923509, -26.21806220515917474, 7.779495906702013741 ) ) ;
#19636 = CARTESIAN_POINT ( 'NONE',  ( 1.206567936595640100, -26.10494249544789369, 6.865482280155369210 ) ) ;
#19637 = ORIENTED_EDGE ( 'NONE', *, *, #22115, .F. ) ;
#19638 = FACE_OUTER_BOUND ( 'NONE', #31479, .T. ) ;
#19639 = CARTESIAN_POINT ( 'NONE',  ( 81.21077662890941440, 62.27078576854649583, 2.885071930847908028 ) ) ;
#19640 = VECTOR ( 'NONE', #7427, 1000.000000000000000 ) ;
#19642 = EDGE_CURVE ( 'NONE', #24852, #15453, #16315, .T. ) ;
#19641 = CARTESIAN_POINT ( 'NONE',  ( 4.826555071938813946, -30.90675198375193844, 7.013842709614101167 ) ) ;
#19643 = ORIENTED_EDGE ( 'NONE', *, *, #38488, .T. ) ;
#19644 = CARTESIAN_POINT ( 'NONE',  ( 78.45565513354563336, 64.70068626995113448, -3.258123098320685695 ) ) ;
#19646 = CARTESIAN_POINT ( 'NONE',  ( -1.656469331124993616, -30.10983836210348485, 6.892063359921931642 ) ) ;
#19645 = CARTESIAN_POINT ( 'NONE',  ( 21.79003266261817373, 0.2242721076120573753, 8.362678294596348039 ) ) ;
#19647 = CARTESIAN_POINT ( 'NONE',  ( 79.11601629524606949, 66.18432715369988273, -1.588372325568319754 ) ) ;
#19648 =( BOUNDED_SURFACE ( )  B_SPLINE_SURFACE ( 3, 2, ( 
 ( #29315, #4606, #29710 ),
 ( #16537, #17135, #920 ),
 ( #22945, #7279, #23541 ),
 ( #19843, #20432, #15072 ),
 ( #24130, #30529, #29909 ),
 ( #2338, #11157, #36695 ),
 ( #14455, #24542, #39367 ),
 ( #30324, #21059, #2132 ),
 ( #27222, #33631, #40185 ),
 ( #8679, #37099, #27628 ),
 ( #39785, #8476, #5407 ),
 ( #20839, #33011, #5002 ),
 ( #8268, #33833, #14650 ),
 ( #17946, #23921, #14858 ),
 ( #4800, #2546, #17331 ),
 ( #30742, #23728, #1724 ),
 ( #14254, #36294, #27026 ),
 ( #11557, #26826, #27428 ) ),
 .UNSPECIFIED., .F., .F., .T. ) 
 B_SPLINE_SURFACE_WITH_KNOTS ( ( 4, 2, 2, 2, 2, 2, 2, 2, 4 ),
 ( 3, 3 ),
 ( -3.897706810085388440E-17, 9.268508998302566707E-05, 0.0001853701799660903112, 0.0003707403599322195995, 0.0005561105398983489691, 0.0006487956298814135997, 0.0006951381748729458607, 0.0007183094473687120455, 0.0007414807198644782302 ),
 ( 0.000000000000000000, 1.000000000000000000 ),
 .UNSPECIFIED. ) 
 GEOMETRIC_REPRESENTATION_ITEM ( )  RATIONAL_B_SPLINE_SURFACE ( (
 ( 1.000000000000000000, 0.9970051441236879031, 1.000000000000000000),
 ( 1.000000000000000000, 0.9970378225561581376, 1.000000000000000000),
 ( 1.000000000000000000, 0.9972394906898559563, 1.000000000000000000),
 ( 1.000000000000000000, 0.9976321421133419465, 1.000000000000000000),
 ( 1.000000000000000000, 0.9978422869890333224, 1.000000000000000000),
 ( 1.000000000000000000, 0.9984523809614584966, 1.000000000000000000),
 ( 1.000000000000000000, 0.9988360290112493489, 1.000000000000000000),
 ( 1.000000000000000000, 0.9994464665223562472, 1.000000000000000000),
 ( 1.000000000000000000, 0.9996736563026237254, 1.000000000000000000),
 ( 1.000000000000000000, 0.9998843893650831705, 1.000000000000000000),
 ( 1.000000000000000000, 0.9999333845000230037, 1.000000000000000000),
 ( 1.000000000000000000, 0.9999776760172924828, 1.000000000000000000),
 ( 1.000000000000000000, 0.9999875764423735713, 1.000000000000000000),
 ( 1.000000000000000000, 0.9999962119944856287, 1.000000000000000000),
 ( 1.000000000000000000, 0.9999980683705610440, 1.000000000000000000),
 ( 1.000000000000000000, 0.9999999292169973186, 1.000000000000000000),
 ( 1.000000000000000000, 0.9999996798682928567, 1.000000000000000000),
 ( 1.000000000000000000, 0.9999997033893416321, 1.000000000000000000) ) ) 
 REPRESENTATION_ITEM ( '' )  SURFACE ( )  );
#19649 = CARTESIAN_POINT ( 'NONE',  ( 80.29582733418162377, 61.38465067277563492, 2.608847861177660210 ) ) ;
#19650 = LINE ( 'NONE', #20043, #1072 ) ;
#19651 = CARTESIAN_POINT ( 'NONE',  ( 82.35470118046110599, 62.54510421749742477, 1.103079483641125069 ) ) ;
#19653 = ORIENTED_EDGE ( 'NONE', *, *, #11786, .F. ) ;
#19652 = CARTESIAN_POINT ( 'NONE',  ( -63.70768058868310391, 44.39675795731061214, 1.000000000000000000 ) ) ;
#19654 = CARTESIAN_POINT ( 'NONE',  ( 24.33615536228354514, 0.1518143133650739496, -6.924920736309362113 ) ) ;
#19655 = CARTESIAN_POINT ( 'NONE',  ( -64.58420500176733015, 36.29544061437565716, -5.991211914497585944 ) ) ;
#19656 = VERTEX_POINT ( 'NONE', #26406 ) ;
#19657 = CARTESIAN_POINT ( 'NONE',  ( -77.36554191947220716, -6.175991868022603803, 7.662488528983584679 ) ) ;
#19658 = CARTESIAN_POINT ( 'NONE',  ( 24.11813158041969984, 0.4652598558864985967, -5.100767782630346581 ) ) ;
#19659 = EDGE_CURVE ( 'NONE', #28877, #19681, #38936, .T. ) ;
#19660 = CARTESIAN_POINT ( 'NONE',  ( -1.053369181053855463, -31.72885680097385475, 7.761113333116790969 ) ) ;
#19661 = ORIENTED_EDGE ( 'NONE', *, *, #38252, .T. ) ;
#19662 = CARTESIAN_POINT ( 'NONE',  ( 35.83212964707659154, -3.727973511289250030, -5.624487930365151378 ) ) ;
#19663 = CARTESIAN_POINT ( 'NONE',  ( 30.48436916548869391, -3.145932567401911850, -4.957248004276928910 ) ) ;
#19664 = CARTESIAN_POINT ( 'NONE',  ( 3.842201187575565502, -32.21050686967832632, 6.887041543973314361 ) ) ;
#19665 = CARTESIAN_POINT ( 'NONE',  ( 16.29348332828302048, 9.833248505471146927, 2.749390151398705573 ) ) ;
#19666 = CARTESIAN_POINT ( 'NONE',  ( -89.20959394718985891, -30.34358980514384285, 7.013842709614101167 ) ) ;
#19667 = DIRECTION ( 'NONE',  ( 1.000000000000000000, 0.000000000000000000, 0.000000000000000000 ) ) ;
#19668 = CARTESIAN_POINT ( 'NONE',  ( -60.14275962559869981, 24.84364830758654108, -9.154021781743367114 ) ) ;
#19669 = LINE ( 'NONE', #38185, #39432 ) ;
#19670 = CARTESIAN_POINT ( 'NONE',  ( 24.25735127829256399, 1.467485774236111373, -4.660622497933993635 ) ) ;
#19671 = CARTESIAN_POINT ( 'NONE',  ( 33.56666239001700092, -0.3391249266082498326, -5.044679946851483798 ) ) ;
#19672 = AXIS2_PLACEMENT_3D ( 'NONE', #24024, #30216, #4700 ) ;
#19673 = CARTESIAN_POINT ( 'NONE',  ( -40.24874870218063450, -26.64985754041175525, 6.700000000000000178 ) ) ;
#19674 = VERTEX_POINT ( 'NONE', #32589 ) ;
#19675 = EDGE_CURVE ( 'NONE', #31513, #1511, #16682, .T. ) ;
#19677 = EDGE_CURVE ( 'NONE', #34818, #5866, #18618, .T. ) ;
#19676 = CARTESIAN_POINT ( 'NONE',  ( 66.68517307240369973, 57.97439930951417608, 3.998354769216140525 ) ) ;
#19678 = EDGE_CURVE ( 'NONE', #20726, #28508, #21532, .T. ) ;
#19679 = CARTESIAN_POINT ( 'NONE',  ( 86.04767080185138184, 0.5164224212623146348, 6.001289606117265585 ) ) ;
#19680 = PLANE ( 'NONE',  #14287 ) ;
#19681 = VERTEX_POINT ( 'NONE', #15545 ) ;
#19682 = CARTESIAN_POINT ( 'NONE',  ( -76.51636512074169616, 9.210593808855891851, -9.784462033820121363 ) ) ;
#19683 = DIRECTION ( 'NONE',  ( 0.000000000000000000, 0.000000000000000000, 1.000000000000000000 ) ) ;
#19684 = CARTESIAN_POINT ( 'NONE',  ( 2.891262396755087671, -26.28021669631634438, 7.762796336881261361 ) ) ;
#19685 = DIRECTION ( 'NONE',  ( -1.000000000000000000, 0.000000000000000000, 0.000000000000000000 ) ) ;
#19686 = ORIENTED_EDGE ( 'NONE', *, *, #168, .T. ) ;
#19687 = ORIENTED_EDGE ( 'NONE', *, *, #528, .T. ) ;
#19688 = CARTESIAN_POINT ( 'NONE',  ( 78.44852601586514140, 65.88695166727248420, -1.521414672925273770 ) ) ;
#19689 = CARTESIAN_POINT ( 'NONE',  ( 78.90889979212963112, 65.37513451817271459, 2.884918531047065748 ) ) ;
#19691 = ORIENTED_EDGE ( 'NONE', *, *, #15103, .F. ) ;
#19690 = CARTESIAN_POINT ( 'NONE',  ( -39.07867591359219261, -24.55319635012989110, 6.700000000000000178 ) ) ;
#19692 = B_SPLINE_CURVE_WITH_KNOTS ( 'NONE', 3,
 ( #39336, #2304, #14826, #7850, #35873, #21026, #33600, #29676, #1903, #20203, #11527, #1488, #4970, #7652, #14022, #5374, #14423, #26992, #32787, #10930, #39538, #8442, #26595, #10724, #23509, #4578, #36073, #32980, #17301, #17497, #17914 ),
 .UNSPECIFIED., .F., .F.,
 ( 4, 3, 3, 3, 3, 3, 3, 3, 3, 3, 4 ),
 ( 3.049318610115481221E-20, 3.077658087705713937E-05, 6.152638666999062957E-05, 9.267501192706755864E-05, 0.0001241882240135204452, 0.0001556618703051673963, 0.0001866161554452218428, 0.0002167966385860980115, 0.0002463805737537775979, 0.0002758761370306525985, 0.0002847094172290031517 ),
 .UNSPECIFIED. ) ;
#19693 = CARTESIAN_POINT ( 'NONE',  ( 24.21576457907998048, 2.660053767493973265, 3.985853741681663287 ) ) ;
#19694 = AXIS2_PLACEMENT_3D ( 'NONE', #8841, #11925, #24085 ) ;
#19695 = CARTESIAN_POINT ( 'NONE',  ( 1.700390093233090871, -29.56993018339339940, 7.750000000000000888 ) ) ;
#19696 = DIRECTION ( 'NONE',  ( 0.000000000000000000, 1.000000000000000000, 0.000000000000000000 ) ) ;
#19697 = CARTESIAN_POINT ( 'NONE',  ( 21.85643539959780313, -10.31987362501297056, 12.61309593674697993 ) ) ;
#19698 = CARTESIAN_POINT ( 'NONE',  ( 23.42712317297381119, 3.762989615831232371, -3.173731162736729061 ) ) ;
#19699 = ORIENTED_EDGE ( 'NONE', *, *, #30094, .T. ) ;
#19700 = LINE ( 'NONE', #8539, #19592 ) ;
#19701 = ORIENTED_EDGE ( 'NONE', *, *, #37455, .T. ) ;
#19702 = CARTESIAN_POINT ( 'NONE',  ( -0.9384404336435322458, -31.71389406695070790, 6.889465824494253710 ) ) ;
#19703 = CARTESIAN_POINT ( 'NONE',  ( 4.283498045048843572, -27.35914579868425278, 7.670860738520329569 ) ) ;
#19704 = CARTESIAN_POINT ( 'NONE',  ( -72.84083785044238368, 2.619656753172959540, -9.875546965173446878 ) ) ;
#19705 = CARTESIAN_POINT ( 'NONE',  ( 5.141430038532381452, -28.93020829471468858, 7.670465701733746755 ) ) ;
#19706 = DIRECTION ( 'NONE',  ( 0.000000000000000000, -0.000000000000000000, -1.000000000000000000 ) ) ;
#19707 = CARTESIAN_POINT ( 'NONE',  ( 80.53345128649188212, 64.37995495044675920, 3.533418250979424968 ) ) ;
#19708 = CARTESIAN_POINT ( 'NONE',  ( 85.28844081106248609, 1.468752784057639094, 5.439171570854275828 ) ) ;
#19709 = CARTESIAN_POINT ( 'NONE',  ( -18.34874870218063947, -26.64985754041175525, 6.800000000000000711 ) ) ;
#19710 = FACE_BOUND ( 'NONE', #25573, .T. ) ;
#19711 = CARTESIAN_POINT ( 'NONE',  ( 3.936759689487521641, -26.87759828911498516, 7.750000000000000888 ) ) ;
#19712 = EDGE_CURVE ( 'NONE', #2537, #18532, #19190, .T. ) ;
#19713 = AXIS2_PLACEMENT_3D ( 'NONE', #17050, #11073, #11271 ) ;
#19714 = CARTESIAN_POINT ( 'NONE',  ( 1.730667593378961477, -26.17006499886255710, 7.782167645815905033 ) ) ;
#19715 = EDGE_CURVE ( 'NONE', #40540, #39495, #33678, .T. ) ;
#19716 = CARTESIAN_POINT ( 'NONE',  ( -0.3639226275255784682, -26.86831799423209688, 6.871394612369935651 ) ) ;
#19717 = CARTESIAN_POINT ( 'NONE',  ( 4.679472942922894063, -27.93128239903199628, 7.784476445165072533 ) ) ;
#19718 = DIRECTION ( 'NONE',  ( 0.000000000000000000, 0.000000000000000000, -1.000000000000000000 ) ) ;
#19719 =( BOUNDED_CURVE ( )  B_SPLINE_CURVE ( 3, ( #10714, #33173, #33391, #20588 ),
 .UNSPECIFIED., .F., .T. ) 
 B_SPLINE_CURVE_WITH_KNOTS ( ( 4, 4 ),
 ( 1.381924640371166690, 1.574767692156075372 ),
 .UNSPECIFIED. ) 
 CURVE ( )  GEOMETRIC_REPRESENTATION_ITEM ( )  RATIONAL_B_SPLINE_CURVE ( ( 1.000000000000000000, 0.9969033633783032089, 0.9969033633783032089, 1.000000000000000000 ) ) 
 REPRESENTATION_ITEM ( '' )  );
#19720 = CARTESIAN_POINT ( 'NONE',  ( 68.48614864092384380, 58.93304109727553453, 3.970924506823388711 ) ) ;
#19721 = CARTESIAN_POINT ( 'NONE',  ( 35.78615804230325637, -3.164549726578430811, 5.791693472641034290 ) ) ;
#19722 = EDGE_CURVE ( 'NONE', #14346, #36231, #40045, .T. ) ;
#19723 = CARTESIAN_POINT ( 'NONE',  ( 4.229427455569045868, -31.84236720560299005, 7.761597726988855861 ) ) ;
#19724 = CARTESIAN_POINT ( 'NONE',  ( 85.06715496341631422, 2.806258611057371066, -0.4571093354346482673 ) ) ;
#19725 = CIRCLE ( 'NONE', #5939, 21.28220113893567245 ) ;
#19727 = CARTESIAN_POINT ( 'NONE',  ( -0.4126339070069648951, -26.77974567795123662, 7.006908160621408754 ) ) ;
#19726 = CARTESIAN_POINT ( 'NONE',  ( 81.13325097526887930, 61.29068799862991312, -1.183438861787473151 ) ) ;
#19728 = CARTESIAN_POINT ( 'NONE',  ( -1.271367234268484081, -27.72096874884677931, 6.865482280155368322 ) ) ;
#19729 = ORIENTED_EDGE ( 'NONE', *, *, #26681, .T. ) ;
#19730 = CARTESIAN_POINT ( 'NONE',  ( 11.65737507970504439, -23.60493063168009442, 6.800000000000000711 ) ) ;
#19731 = VERTEX_POINT ( 'NONE', #8947 ) ;
#19732 = CARTESIAN_POINT ( 'NONE',  ( -75.07873864619844539, -4.847503269688606231, 9.099517967925462969 ) ) ;
#19733 = EDGE_LOOP ( 'NONE', ( #27784, #36629, #13507, #13451, #25357, #31526 ) ) ;
#19734 = ADVANCED_FACE ( 'NONE', ( #33898 ), #2612, .F. ) ;
#19735 = CARTESIAN_POINT ( 'NONE',  ( 80.33017967436555296, 63.51919597486878644, -3.679799701112255850 ) ) ;
#19736 = CARTESIAN_POINT ( 'NONE',  ( 1.121324086407811338, -26.64985754041175525, 6.700000000000000178 ) ) ;
#19737 = CARTESIAN_POINT ( 'NONE',  ( 24.25000701045975404, 1.480808258834079183, 4.656548141442817368 ) ) ;
#19738 = VERTEX_POINT ( 'NONE', #32027 ) ;
#19739 = CARTESIAN_POINT ( 'NONE',  ( 81.16688244586958945, 61.30299313749268464, -1.050153991572639667 ) ) ;
#19740 = CARTESIAN_POINT ( 'NONE',  ( -0.03413980529548706760, -32.49422506527100296, 7.784838882742139532 ) ) ;
#19742 = CARTESIAN_POINT ( 'NONE',  ( 85.14854983093479746, 2.714832032627191971, 0.8233776845609513950 ) ) ;
#19741 = CARTESIAN_POINT ( 'NONE',  ( 4.597156102822266277, -31.35005458526572752, 6.866852738645444987 ) ) ;
#19743 = DIRECTION ( 'NONE',  ( -0.000000000000000000, -0.000000000000000000, 1.000000000000000000 ) ) ;
#19744 = CARTESIAN_POINT ( 'NONE',  ( -64.08758708074094557, 42.81038502649571598, -3.275296300469149546 ) ) ;
#19745 = CARTESIAN_POINT ( 'NONE',  ( 70.96793116520528599, 59.41887718710786714, 3.976054184260645386 ) ) ;
#19746 = CARTESIAN_POINT ( 'NONE',  ( 23.42844204553037102, 3.310894996220114184, -3.716253240727860785 ) ) ;
#19747 = EDGE_LOOP ( 'NONE', ( #15676, #30934, #22501, #8250 ) ) ;
#19748 = DIRECTION ( 'NONE',  ( 1.000000000000000000, -1.189524669241239263E-14, 0.000000000000000000 ) ) ;
#19749 = ORIENTED_EDGE ( 'NONE', *, *, #6152, .T. ) ;
#19750 = CARTESIAN_POINT ( 'NONE',  ( 21.85643539959775694, 2.837881715527333260, -11.82040581148825353 ) ) ;
#19751 = AXIS2_PLACEMENT_3D ( 'NONE', #20810, #18121, #33406 ) ;
#19752 = CARTESIAN_POINT ( 'NONE',  ( 18.14195397311783964, 13.68994309133305975, 3.806916816956696259 ) ) ;
#19753 = CARTESIAN_POINT ( 'NONE',  ( 0.3572758658287483180, -32.69339687477079082, 6.903372536218454592 ) ) ;
#19754 = CARTESIAN_POINT ( 'NONE',  ( 78.68583465488319462, 66.05536144407729182, 1.071687152257635667 ) ) ;
#19755 = CARTESIAN_POINT ( 'NONE',  ( 86.86561140461988373, 0.2703162379016064154, -5.930766725306959586 ) ) ;
#19756 = CARTESIAN_POINT ( 'NONE',  ( -1.786444507892435585, -29.53457013502913497, 7.783750581861600182 ) ) ;
#19757 = ORIENTED_EDGE ( 'NONE', *, *, #2396, .F. ) ;
#19758 = CARTESIAN_POINT ( 'NONE',  ( 15.55097496540485302, -3.641916182646045996, 2.633503763738948233 ) ) ;
#19759 = FACE_OUTER_BOUND ( 'NONE', #30792, .T. ) ;
#19760 = CARTESIAN_POINT ( 'NONE',  ( 30.51576791750731488, -0.1387227150358968375, -4.969121628799780588 ) ) ;
#19761 = DIRECTION ( 'NONE',  ( -0.000000000000000000, -0.000000000000000000, -1.000000000000000000 ) ) ;
#19762 = CARTESIAN_POINT ( 'NONE',  ( 84.09810771740265523, 3.020293266994594994, 0.2534269013960862016 ) ) ;
#19763 = CARTESIAN_POINT ( 'NONE',  ( -73.56224669261729332, -0.9187133512700828009, 10.86667021741267369 ) ) ;
#19764 = EDGE_LOOP ( 'NONE', ( #5259, #12367, #24945, #21506 ) ) ;
#19765 = DIRECTION ( 'NONE',  ( 0.000000000000000000, -0.000000000000000000, -1.000000000000000000 ) ) ;
#19766 = EDGE_CURVE ( 'NONE', #20836, #2808, #37855, .T. ) ;
#19768 = ADVANCED_FACE ( 'NONE', ( #932 ), #23150, .F. ) ;
#19767 = AXIS2_PLACEMENT_3D ( 'NONE', #5232, #5644, #27858 ) ;
#19769 = EDGE_CURVE ( 'NONE', #8458, #13946, #26248, .T. ) ;
#19770 = CARTESIAN_POINT ( 'NONE',  ( 3.429035706983251774, -32.49769360082827063, 7.670860738520329569 ) ) ;
#19771 = EDGE_CURVE ( 'NONE', #9354, #8785, #34924, .T. ) ;
#19772 = CARTESIAN_POINT ( 'NONE',  ( 29.51363873213982103, -3.424872186366097360, 4.784073270833150815 ) ) ;
#19773 = VERTEX_POINT ( 'NONE', #35520 ) ;
#19774 = ORIENTED_EDGE ( 'NONE', *, *, #35777, .T. ) ;
#19775 = CARTESIAN_POINT ( 'NONE',  ( 20.91912723174414523, 4.580704557862071979, 2.655339189496692232 ) ) ;
#19776 = CYLINDRICAL_SURFACE ( 'NONE', #9336, 0.09010775117052885475 ) ;
#19777 = CARTESIAN_POINT ( 'NONE',  ( 66.27376694609004915, 57.73522568913436004, -4.000000000000000000 ) ) ;
#19778 = CARTESIAN_POINT ( 'NONE',  ( 87.48590409800530665, -1.976339587909113016, 3.594369327898899513 ) ) ;
#19779 = ORIENTED_EDGE ( 'NONE', *, *, #16662, .F. ) ;
#19780 = CIRCLE ( 'NONE', #31634, 1.000000000000003997 ) ;
#19781 = CARTESIAN_POINT ( 'NONE',  ( 5.143311846931861275, -28.94039731499685786, 7.743886751744253338 ) ) ;
#19782 = FACE_OUTER_BOUND ( 'NONE', #18392, .T. ) ;
#19783 = ORIENTED_EDGE ( 'NONE', *, *, #29069, .F. ) ;
#19784 = CARTESIAN_POINT ( 'NONE',  ( -58.07367359896441172, 31.71941035118960883, -4.399945119674323557 ) ) ;
#19785 = DIRECTION ( 'NONE',  ( -0.3420201433256601087, -0.9396926207859114255, -0.000000000000000000 ) ) ;
#19786 = ORIENTED_EDGE ( 'NONE', *, *, #35268, .T. ) ;
#19787 = CARTESIAN_POINT ( 'NONE',  ( 80.64785791202326948, 66.17610879001705371, -1.553473047276890284 ) ) ;
#19788 = CARTESIAN_POINT ( 'NONE',  ( -22.97867591359219119, -24.55319635012989110, 6.700000000000000178 ) ) ;
#19789 = DIRECTION ( 'NONE',  ( -0.000000000000000000, -0.000000000000000000, 1.000000000000000000 ) ) ;
#19790 = ORIENTED_EDGE ( 'NONE', *, *, #7898, .F. ) ;
#19791 = CARTESIAN_POINT ( 'NONE',  ( 74.91689101425367880, 62.74844471888589226, -3.527522301306301511 ) ) ;
#19793 = CARTESIAN_POINT ( 'NONE',  ( 4.390852040715039983, -27.34879134089963415, 7.781480525794719050 ) ) ;
#19792 = CARTESIAN_POINT ( 'NONE',  ( -1.600265505308078318, -28.40559435941229438, 7.678495282201406980 ) ) ;
#19794 = CARTESIAN_POINT ( 'NONE',  ( -69.95447152169636240, -0.5205953579843026757, 5.920650877785231359 ) ) ;
#19795 = CARTESIAN_POINT ( 'NONE',  ( 77.22142874756848130, 60.78359660874929915, 3.498861892161886811 ) ) ;
#19796 = ORIENTED_EDGE ( 'NONE', *, *, #39824, .F. ) ;
#19797 = ORIENTED_EDGE ( 'NONE', *, *, #40713, .F. ) ;
#19798 = DIRECTION ( 'NONE',  ( 0.000000000000000000, 1.000000000000000000, 0.000000000000000000 ) ) ;
#19799 = VECTOR ( 'NONE', #15898, 1000.000000000000000 ) ;
#19800 = CYLINDRICAL_SURFACE ( 'NONE', #26734, 2.500000000000000000 ) ;
#19801 = CARTESIAN_POINT ( 'NONE',  ( 24.20448666664697868, 2.666065671757310795, -3.984093550689149055 ) ) ;
#19802 = DIRECTION ( 'NONE',  ( 0.000000000000000000, 0.000000000000000000, 1.000000000000000000 ) ) ;
#19803 = CARTESIAN_POINT ( 'NONE',  ( 81.69611827519081260, 64.99316753419206805, 2.512558077907662391 ) ) ;
#19804 = CARTESIAN_POINT ( 'NONE',  ( -0.1945137394687337096, -32.51260574566864392, 6.895394898881673562 ) ) ;
#19805 = CARTESIAN_POINT ( 'NONE',  ( 30.10774373291980766, -4.462292185204852046, -2.031966353365944666 ) ) ;
#19806 = CARTESIAN_POINT ( 'NONE',  ( -1.699587041002557086, -29.58345656395455592, 7.755436452974803885 ) ) ;
#19807 = LINE ( 'NONE', #1292, #37332 ) ;
#19808 = CARTESIAN_POINT ( 'NONE',  ( -63.96695182803194513, 19.27020452292901709, 8.800414904976364028 ) ) ;
#19809 = CARTESIAN_POINT ( 'NONE',  ( 0.7267180850964402028, -26.31232708533429232, 6.997764925645182821 ) ) ;
#19810 = DIRECTION ( 'NONE',  ( -1.000000000000000000, 0.000000000000000000, 0.000000000000000000 ) ) ;
#19811 = CARTESIAN_POINT ( 'NONE',  ( 36.29305064575918038, -2.016329881244163680, -5.862899224838821866 ) ) ;
#19812 = DIRECTION ( 'NONE',  ( 0.000000000000000000, 1.000000000000000000, 0.000000000000000000 ) ) ;
#19813 = DIRECTION ( 'NONE',  ( 0.000000000000000000, 0.000000000000000000, 1.000000000000000000 ) ) ;
#19814 = CARTESIAN_POINT ( 'NONE',  ( 3.374101601209122059, -32.52943855271229268, 7.782167645815905033 ) ) ;
#19815 = CARTESIAN_POINT ( 'NONE',  ( -63.48446588846724836, 43.17223388165376718, -3.327560541823090023 ) ) ;
#19816 = CARTESIAN_POINT ( 'NONE',  ( 23.06591706423118637, -8.086835649431872497, -2.500000000000005773 ) ) ;
#19817 = CARTESIAN_POINT ( 'NONE',  ( -0.4595759649632789601, -32.19567977424306093, 7.670860738520322464 ) ) ;
#19818 = EDGE_CURVE ( 'NONE', #36134, #1678, #4222, .T. ) ;
#19819 = CARTESIAN_POINT ( 'NONE',  ( -70.92837670882107659, 15.04836564048558500, 3.784187430299790211 ) ) ;
#19820 = VERTEX_POINT ( 'NONE', #16743 ) ;
#19821 = CARTESIAN_POINT ( 'NONE',  ( 37.10281511974962854, -2.625417964323302211, 5.990186448831483546 ) ) ;
#19822 = CARTESIAN_POINT ( 'NONE',  ( 2.835023152515760980, -26.35730453524175942, 7.257242401810562349 ) ) ;
#19823 = CARTESIAN_POINT ( 'NONE',  ( 67.14845837397145090, 58.06767444754134289, -3.999036733496184048 ) ) ;
#19824 = CARTESIAN_POINT ( 'NONE',  ( 4.718801410692444520, -27.79814376769215301, 7.651421919295145813 ) ) ;
#19825 = VERTEX_POINT ( 'NONE', #532 ) ;
#19826 = CARTESIAN_POINT ( 'NONE',  ( 4.733915118986097958, -28.03444136281207832, 7.013842709614101167 ) ) ;
#19827 = CARTESIAN_POINT ( 'NONE',  ( -24.24874870218063450, -25.49307895267003587, 6.800000000000000711 ) ) ;
#19828 = CARTESIAN_POINT ( 'NONE',  ( 23.00813552179332788, 3.484112554442508003, 3.810651395707427724 ) ) ;
#19829 = CARTESIAN_POINT ( 'NONE',  ( 0.9267304714826859469, -32.88073836111571779, 7.013842709614101167 ) ) ;
#19830 = SHAPE_REPRESENTATION ( 'Press Handle', ( #30744 ), #18224 ) ;
#19831 = CARTESIAN_POINT ( 'NONE',  ( -32.97867591359219119, -24.55319635012989110, 6.800000000000000711 ) ) ;
#19832 = CARTESIAN_POINT ( 'NONE',  ( 4.404516770028685357, -31.79202354683301834, 7.686927408461905031 ) ) ;
#19833 = VERTEX_POINT ( 'NONE', #726 ) ;
#19834 = CARTESIAN_POINT ( 'NONE',  ( 21.71193631872560559, 6.329239510039562866, 3.192900200192605897 ) ) ;
#19835 = FACE_OUTER_BOUND ( 'NONE', #33716, .T. ) ;
#19836 = CARTESIAN_POINT ( 'NONE',  ( 16.86712048606784009, -3.293910290563445198, 2.810174632765468417 ) ) ;
#19837 = CARTESIAN_POINT ( 'NONE',  ( 80.75501959326771839, 63.35152955421530407, 3.552238747020031617 ) ) ;
#19838 = AXIS2_PLACEMENT_3D ( 'NONE', #11304, #24079, #5155 ) ;
#19839 = CARTESIAN_POINT ( 'NONE',  ( 19.23826442257826841, -6.969287627455325485, -2.500000000000009326 ) ) ;
#19840 = VERTEX_POINT ( 'NONE', #32230 ) ;
#19841 = CARTESIAN_POINT ( 'NONE',  ( 79.88607388276625443, 61.09294650314146935, -2.551779361026688342 ) ) ;
#19843 = CARTESIAN_POINT ( 'NONE',  ( 14.62029201251024446, -4.585632647846321852, -2.500000000000095035 ) ) ;
#19842 = CARTESIAN_POINT ( 'NONE',  ( 21.98032544390349940, 0.2298825911022993052, 7.706387622467548937 ) ) ;
#19844 = CARTESIAN_POINT ( 'NONE',  ( 79.64807995745978531, 65.91648781525297807, -2.476693319882547151 ) ) ;
#19845 = ADVANCED_FACE ( 'NONE', ( #13067 ), #27552, .F. ) ;
#19846 = CARTESIAN_POINT ( 'NONE',  ( 78.07232077886961008, 65.35672112437505632, 2.431999527814446171 ) ) ;
#19847 = CARTESIAN_POINT ( 'NONE',  ( 82.07069543531883937, 65.18928443706822407, 1.480606629405690544 ) ) ;
#19849 = ORIENTED_EDGE ( 'NONE', *, *, #37936, .T. ) ;
#19848 = CARTESIAN_POINT ( 'NONE',  ( 8.290806648384990041, -33.63722727088462250, -6.000000000000001776 ) ) ;
#19850 = CARTESIAN_POINT ( 'NONE',  ( 23.92064240948634790, 4.179079982057642972, -0.5982227118658990372 ) ) ;
#19851 = CARTESIAN_POINT ( 'NONE',  ( -32.24874870218063450, -26.64985754041175525, 6.800000000000000711 ) ) ;
#19852 = EDGE_LOOP ( 'NONE', ( #13517, #38850, #16383, #27673, #29733, #9429, #9792, #23033, #40144, #3727, #4033, #18911 ) ) ;
#19853 = CARTESIAN_POINT ( 'NONE',  ( -80.19506747669507263, -6.650235582408308588, 3.780597760675498353 ) ) ;
#19854 = CARTESIAN_POINT ( 'NONE',  ( 0.2535576206106768815, -26.37550602218658469, 7.501983001166817822 ) ) ;
#19855 = CARTESIAN_POINT ( 'NONE',  ( -0.1539201161049026934, -32.53808085965915353, 7.754798119455333705 ) ) ;
#19856 = DIRECTION ( 'NONE',  ( 1.047444401652940007E-14, -1.000000000000000000, -0.000000000000000000 ) ) ;
#19857 = CARTESIAN_POINT ( 'NONE',  ( 36.88765961127775483, -3.350445860750347560, -5.910858986277842675 ) ) ;
#19858 = DIRECTION ( 'NONE',  ( 1.000000000000000000, 0.000000000000000000, 0.000000000000000000 ) ) ;
#19859 = CARTESIAN_POINT ( 'NONE',  ( -1.015903543171244650, -31.77713404367212746, 6.875671892026059773 ) ) ;
#19860 = DIRECTION ( 'NONE',  ( 1.000000000000000000, 0.000000000000000000, 0.000000000000000000 ) ) ;
#19861 = CARTESIAN_POINT ( 'NONE',  ( -16.87867591359218977, -26.64985754041175525, 6.700000000000000178 ) ) ;
#19862 = CARTESIAN_POINT ( 'NONE',  ( 2.748053412748273860, -32.80449376584813592, 7.754798119455333705 ) ) ;
#19863 = FACE_OUTER_BOUND ( 'NONE', #10360, .T. ) ;
#19864 = DIRECTION ( 'NONE',  ( -0.9396926207859005453, -0.3420201433256903067, 0.000000000000000000 ) ) ;
#19865 = EDGE_CURVE ( 'NONE', #36812, #28074, #36419, .T. ) ;
#19866 = CARTESIAN_POINT ( 'NONE',  ( 2.225035496018605841, -33.03038495138792285, 6.865554069792297653 ) ) ;
#19867 = ORIENTED_EDGE ( 'NONE', *, *, #11604, .T. ) ;
#19868 = ORIENTED_EDGE ( 'NONE', *, *, #30483, .T. ) ;
#19869 = CARTESIAN_POINT ( 'NONE',  ( 66.55222248544532704, 57.88363434508141125, 3.999616584014993759 ) ) ;
#19870 = VECTOR ( 'NONE', #44, 1000.000000000000000 ) ;
#19871 = CARTESIAN_POINT ( 'NONE',  ( 84.36871573755720988, 2.689384369868815128, -2.914620128191189874 ) ) ;
#19872 = DIRECTION ( 'NONE',  ( 1.000000000000000000, 0.000000000000000000, -0.000000000000000000 ) ) ;
#19873 = ORIENTED_EDGE ( 'NONE', *, *, #5683, .T. ) ;
#19874 = CARTESIAN_POINT ( 'NONE',  ( 26.55823958201730761, 1.660274760599077526, 4.322293138832669079 ) ) ;
#19875 = FACE_OUTER_BOUND ( 'NONE', #35649, .T. ) ;
#19876 = CARTESIAN_POINT ( 'NONE',  ( 1.111970077971375481, -26.12859514599353972, 7.778495531946297170 ) ) ;
#19877 = EDGE_CURVE ( 'NONE', #34412, #273, #1187, .T. ) ;
#19878 = ORIENTED_EDGE ( 'NONE', *, *, #10757, .F. ) ;
#19879 = CARTESIAN_POINT ( 'NONE',  ( 21.85643539959777115, -33.54387950140291963, 2.500000000000000000 ) ) ;
#19880 = ORIENTED_EDGE ( 'NONE', *, *, #877, .T. ) ;
#19881 = CARTESIAN_POINT ( 'NONE',  ( 79.30508931962887686, 64.72973333162801168, -3.449595662144194108 ) ) ;
#19882 = B_SPLINE_CURVE_WITH_KNOTS ( 'NONE', 3,
 ( #9530, #38139, #9745, #29090, #28478, #28687, #26004, #13233, #16318, #19623, #34689, #31992, #6465, #13032, #25799, #19017, #10134, #892, #31578, #38333, #32197, #9325, #3404, #15917, #285 ),
 .UNSPECIFIED., .F., .F.,
 ( 4, 3, 3, 3, 3, 3, 3, 3, 4 ),
 ( 6.468151674593778733E-05, 9.076621574722025119E-05, 0.0001210204262068008668, 0.0001512763324577457336, 0.0001815301820994240595, 0.0002117781465860724675, 0.0002420274594459785687, 0.0002722905548971212095, 0.0002816827545175671905 ),
 .UNSPECIFIED. ) ;
#19883 = CARTESIAN_POINT ( 'NONE',  ( 33.89348300072561671, -5.437596492814196658, 0.9556765382706865486 ) ) ;
#19884 = CARTESIAN_POINT ( 'NONE',  ( 2.294856720451861953, -26.12078399496891734, 7.635761828346576685 ) ) ;
#19885 = LINE ( 'NONE', #16582, #33742 ) ;
#19886 = CARTESIAN_POINT ( 'NONE',  ( 0.9084830412599044225, -32.97916797363021857, 6.925313231306333250 ) ) ;
#19887 = CARTESIAN_POINT ( 'NONE',  ( -10.44874870218064089, -26.64985754041175525, 6.700000000000000178 ) ) ;
#19888 = ADVANCED_FACE ( 'NONE', ( #26877 ), #29759, .T. ) ;
#19889 = EDGE_CURVE ( 'NONE', #30246, #30686, #39218, .T. ) ;
#19890 = CARTESIAN_POINT ( 'NONE',  ( 21.85643539959779602, 6.788858854521340191, -12.70575755685024610 ) ) ;
#19891 = CARTESIAN_POINT ( 'NONE',  ( 3.369155479471896530, -26.60763004909045293, 7.695279973900954751 ) ) ;
#19892 = ORIENTED_EDGE ( 'NONE', *, *, #22004, .T. ) ;
#19893 = CARTESIAN_POINT ( 'NONE',  ( -57.16504416091206053, 33.41445838748276742, 4.000000000000000000 ) ) ;
#19894 = AXIS2_PLACEMENT_3D ( 'NONE', #33257, #26863, #36738 ) ;
#19895 = ADVANCED_FACE ( 'NONE', ( #16349 ), #28922, .F. ) ;
#19896 = CARTESIAN_POINT ( 'NONE',  ( 14.76364886281816702, -5.161460284205085181, -2.499999999999998668 ) ) ;
#19897 = CARTESIAN_POINT ( 'NONE',  ( -0.6366397171544941891, -32.17424313428438865, 7.761113333116783863 ) ) ;
#19898 = CARTESIAN_POINT ( 'NONE',  ( -72.17181076888959979, 5.281718996255664322, -9.923482759818879728 ) ) ;
#19899 = CARTESIAN_POINT ( 'NONE',  ( 4.713718104732327774, -27.78952162317270691, 7.710604733652627552 ) ) ;
#19900 = PLANE ( 'NONE',  #26102 ) ;
#19901 = CARTESIAN_POINT ( 'NONE',  ( 79.79486853628225163, 65.42109455898983583, 3.057227112800002367 ) ) ;
#19902 = CARTESIAN_POINT ( 'NONE',  ( 4.921324086407802056, -24.55319635012989110, 6.700000000000000178 ) ) ;
#19903 = CARTESIAN_POINT ( 'NONE',  ( 3.871457482660439986, -26.95335486619629606, 7.748216051605115950 ) ) ;
#19904 = CARTESIAN_POINT ( 'NONE',  ( -0.8827178585826440660, -31.78071456810256734, 7.670860738520331346 ) ) ;
#19905 = CYLINDRICAL_SURFACE ( 'NONE', #14021, 0.09010775117053081151 ) ;
#19906 = VERTEX_POINT ( 'NONE', #25227 ) ;
#19907 = CARTESIAN_POINT ( 'NONE',  ( -42.83131703149249603, -29.56993018339339940, 6.800000000000000711 ) ) ;
#19908 = CARTESIAN_POINT ( 'NONE',  ( 21.29222209659852538, 5.334569642440764703, -3.529564231148301090 ) ) ;
#19909 = CARTESIAN_POINT ( 'NONE',  ( 4.934953675687837382, -28.52226686387824373, 7.754798119455333705 ) ) ;
#19910 = CYLINDRICAL_SURFACE ( 'NONE', #4976, 0.09010775117052882699 ) ;
#19911 = EDGE_CURVE ( 'NONE', #10365, #25891, #15945, .T. ) ;
#19912 = ORIENTED_EDGE ( 'NONE', *, *, #34604, .F. ) ;
#19913 = CARTESIAN_POINT ( 'NONE',  ( 69.05402862303502332, 59.18504256499077343, 3.962610901733955693 ) ) ;
#19914 = CARTESIAN_POINT ( 'NONE',  ( 33.46257264326497705, -3.087412692527623737, 5.429041774995859271 ) ) ;
#19915 = AXIS2_PLACEMENT_3D ( 'NONE', #17187, #20279, #32459 ) ;
#19916 = DIRECTION ( 'NONE',  ( 0.9267318687906771491, -0.3757233601570964532, -0.000000000000000000 ) ) ;
#19917 = CARTESIAN_POINT ( 'NONE',  ( 85.06055580697953644, 2.762169973306998205, -2.784126402610546780 ) ) ;
#19919 = CARTESIAN_POINT ( 'NONE',  ( -0.4362586782667852714, -26.79779526112715615, 6.875780273367529283 ) ) ;
#19918 = CARTESIAN_POINT ( 'NONE',  ( 79.44789965344524774, 65.49939714349790165, -2.911438267503722699 ) ) ;
#19920 = CARTESIAN_POINT ( 'NONE',  ( -63.08758708074093136, 38.13199975834722011, -3.043809435734137647 ) ) ;
#19921 = CARTESIAN_POINT ( 'NONE',  ( 88.07494619931479463, -0.5722352634876846089, -2.741974656063581595 ) ) ;
#19922 = ORIENTED_EDGE ( 'NONE', *, *, #1938, .F. ) ;
#19923 = DIRECTION ( 'NONE',  ( 0.000000000000000000, 0.000000000000000000, -1.000000000000000000 ) ) ;
#19924 = EDGE_LOOP ( 'NONE', ( #14850, #15167, #36617, #306, #22089, #23531, #15814, #10888 ) ) ;
#19925 = EDGE_LOOP ( 'NONE', ( #39398, #29953, #33788, #16991 ) ) ;
#19926 = CARTESIAN_POINT ( 'NONE',  ( 80.02704812380972044, 64.10187485077996428, -3.679799701112256738 ) ) ;
#19927 = CARTESIAN_POINT ( 'NONE',  ( 20.40287464304303100, 10.75613383955523616, -2.500000000000000000 ) ) ;
#19928 = CARTESIAN_POINT ( 'NONE',  ( 80.74944977059911366, 62.67191958473371471, 3.380189700376619921 ) ) ;
#19929 = CARTESIAN_POINT ( 'NONE',  ( 23.04464813533367007, 1.997931949779890193, 4.910482787407937089 ) ) ;
#19930 = ORIENTED_EDGE ( 'NONE', *, *, #27893, .T. ) ;
#19931 = CIRCLE ( 'NONE', #6164, 3.499999999999999556 ) ;
#19932 = EDGE_CURVE ( 'NONE', #22200, #33808, #2290, .T. ) ;
#19933 = PLANE ( 'NONE',  #28556 ) ;
#19935 = CARTESIAN_POINT ( 'NONE',  ( 85.36928332665556240, 2.466893693589887082, 2.452742180977539821 ) ) ;
#19934 = CARTESIAN_POINT ( 'NONE',  ( 4.534639009953071564, -31.44797187246948411, 6.939395833800439561 ) ) ;
#19936 = CARTESIAN_POINT ( 'NONE',  ( 6.173121028034443292, -31.06824956420287975, 7.754798119455333705 ) ) ;
#19937 = CARTESIAN_POINT ( 'NONE',  ( -63.53001610672649946, 43.42049052265932829, -3.126256110287076062 ) ) ;
#19938 = CARTESIAN_POINT ( 'NONE',  ( 72.33948634203015615, 59.36795819651598549, 3.882941974771883853 ) ) ;
#19939 = CARTESIAN_POINT ( 'NONE',  ( 22.73709572080239028, 4.093838367243191279, -3.481645627490313810 ) ) ;
#19940 = ORIENTED_EDGE ( 'NONE', *, *, #2688, .T. ) ;
#19941 = CARTESIAN_POINT ( 'NONE',  ( 1.700390093233090871, -29.56993018339339940, 7.750000000000000888 ) ) ;
#19942 = ADVANCED_FACE ( 'NONE', ( #6893 ), #3230, .F. ) ;
#19943 = CARTESIAN_POINT ( 'NONE',  ( 21.85643539959777115, 3.923092093126210322, -11.21220060410217734 ) ) ;
#19944 = CARTESIAN_POINT ( 'NONE',  ( 21.75859177104565489, 5.853256811527690395, 2.474032597377961856E-12 ) ) ;
#19945 = CARTESIAN_POINT ( 'NONE',  ( 0.3691700977291238472, -32.69849508640032099, 6.887945620086118659 ) ) ;
#19946 = CARTESIAN_POINT ( 'NONE',  ( 79.06287735989729981, 66.15384612319691371, 1.644402879622035574 ) ) ;
#19947 = CARTESIAN_POINT ( 'NONE',  ( 87.20660408302002509, 0.2574974038930863407, -5.635807106906071340 ) ) ;
#19948 =( BOUNDED_CURVE ( )  B_SPLINE_CURVE ( 3, ( #24161, #30972, #17766, #1961 ),
 .UNSPECIFIED., .F., .T. ) 
 B_SPLINE_CURVE_WITH_KNOTS ( ( 4, 4 ),
 ( 1.381924640371167579, 1.574767692156076260 ),
 .UNSPECIFIED. ) 
 CURVE ( )  GEOMETRIC_REPRESENTATION_ITEM ( )  RATIONAL_B_SPLINE_CURVE ( ( 1.000000000000000000, 0.9969033633783032089, 0.9969033633783032089, 1.000000000000000000 ) ) 
 REPRESENTATION_ITEM ( '' )  );
#19949 = CARTESIAN_POINT ( 'NONE',  ( 29.25459127448231911, -9.786627965178412936, 2.499999999999995115 ) ) ;
#19950 = ORIENTED_EDGE ( 'NONE', *, *, #13576, .F. ) ;
#19951 = CARTESIAN_POINT ( 'NONE',  ( 14.83772866404364166, -6.147680757941134999, 2.522184428484549823 ) ) ;
#19952 = CARTESIAN_POINT ( 'NONE',  ( -40.24874870218063450, -25.49307895267003587, 6.700000000000000178 ) ) ;
#19953 = CARTESIAN_POINT ( 'NONE',  ( 17.01156838727278497, -3.085974904712485589, -2.861464691806836491 ) ) ;
#19954 = CARTESIAN_POINT ( 'NONE',  ( 36.64531717283165335, -2.463042617044940652, -5.925786033801909269 ) ) ;
#19955 = DIRECTION ( 'NONE',  ( -0.000000000000000000, -0.000000000000000000, 1.000000000000000000 ) ) ;
#19956 = FACE_OUTER_BOUND ( 'NONE', #14958, .T. ) ;
#19957 = B_SPLINE_CURVE_WITH_KNOTS ( 'NONE', 3,
 ( #35130, #6907, #10389, #19464, #10180, #1155, #23158, #32037, #3844, #16361 ),
 .UNSPECIFIED., .F., .F.,
 ( 4, 3, 3, 4 ),
 ( 0.0002170292169044849180, 0.0002420761345915980437, 0.0002723302478207024254, 0.0002816811360866880226 ),
 .UNSPECIFIED. ) ;
#19958 = CARTESIAN_POINT ( 'NONE',  ( 3.743426330989782169, -26.71972442647873081, 7.501983001166817822 ) ) ;
#19959 = ORIENTED_EDGE ( 'NONE', *, *, #24625, .T. ) ;
#19960 = LINE ( 'NONE', #13791, #38809 ) ;
#19961 = DIRECTION ( 'NONE',  ( -0.000000000000000000, -1.000000000000000000, -0.000000000000000000 ) ) ;
#19962 = VECTOR ( 'NONE', #21096, 1000.000000000000000 ) ;
#19963 = CARTESIAN_POINT ( 'NONE',  ( -1.146144745493847150, -27.71056485836612637, 7.013842709614101167 ) ) ;
#19964 = ORIENTED_EDGE ( 'NONE', *, *, #16673, .F. ) ;
#19965 = VERTEX_POINT ( 'NONE', #15542 ) ;
#19966 = CARTESIAN_POINT ( 'NONE',  ( 34.14231943393395596, -3.847370251764138604, 5.235623355854905014 ) ) ;
#19967 = CARTESIAN_POINT ( 'NONE',  ( -1.643700780054958566, -30.60291583957470607, 7.009310105710485850 ) ) ;
#19968 = CARTESIAN_POINT ( 'NONE',  ( 2.187796539937281182, -33.03559314236433408, 7.754798119455333705 ) ) ;
#19969 = CARTESIAN_POINT ( 'NONE',  ( 87.46548545408306552, -1.950952776479559558, 3.668367378035980675 ) ) ;
#19970 = ADVANCED_FACE ( 'NONE', ( #34508 ), #13264, .F. ) ;
#19971 = ORIENTED_EDGE ( 'NONE', *, *, #3566, .T. ) ;
#19972 = DIRECTION ( 'NONE',  ( -0.000000000000000000, 0.000000000000000000, 1.000000000000000000 ) ) ;
#19973 =( NAMED_UNIT ( * ) PLANE_ANGLE_UNIT ( ) SI_UNIT ( $, .RADIAN. ) );
#19974 = ORIENTED_EDGE ( 'NONE', *, *, #40454, .T. ) ;
#19975 = CARTESIAN_POINT ( 'NONE',  ( -58.37631287976133621, 28.09510535829620537, -3.265447219236182974 ) ) ;
#19976 = ORIENTED_EDGE ( 'NONE', *, *, #29566, .T. ) ;
#19977 = EDGE_CURVE ( 'NONE', #37652, #18339, #16711, .T. ) ;
#19978 = CARTESIAN_POINT ( 'NONE',  ( 24.37212372168754726, 2.938878590626362808, 3.724495982890795975 ) ) ;
#19979 = CARTESIAN_POINT ( 'NONE',  ( 81.16926347961613430, 61.30386509772021242, -1.017094602978584117 ) ) ;
#19980 = EDGE_CURVE ( 'NONE', #28082, #13946, #25831, .T. ) ;
#19981 = CARTESIAN_POINT ( 'NONE',  ( -1.319585150783705307, -31.33904616602695015, 7.743886751744247121 ) ) ;
#19982 = VERTEX_POINT ( 'NONE', #40650 ) ;
#19983 = CARTESIAN_POINT ( 'NONE',  ( 76.68479537131440793, 60.43247505492704619, -3.462570962778662942 ) ) ;
#19985 = CARTESIAN_POINT ( 'NONE',  ( 4.407950444472939822, -27.37556883494658777, 7.785593909369613819 ) ) ;
#19984 = CARTESIAN_POINT ( 'NONE',  ( 2.415456923980280557, -26.14375455631804712, 6.864673517077424236 ) ) ;
#19986 = CARTESIAN_POINT ( 'NONE',  ( 4.542910857356968535, -31.44822479237316415, 7.386948897581447682 ) ) ;
#19987 = CARTESIAN_POINT ( 'NONE',  ( 75.23821009641450530, 63.49083772021887739, 3.097219288951023053 ) ) ;
#19988 = EDGE_LOOP ( 'NONE', ( #33094, #26277, #499, #16644 ) ) ;
#19989 = CARTESIAN_POINT ( 'NONE',  ( -62.81463675898083210, 36.67811266762162603, 4.600311178732274797 ) ) ;
#19990 = EDGE_CURVE ( 'NONE', #20522, #25319, #32024, .T. ) ;
#19991 = DIRECTION ( 'NONE',  ( -1.000000000000000000, 0.000000000000000000, 0.000000000000000000 ) ) ;
#19992 = VECTOR ( 'NONE', #15840, 1000.000000000000000 ) ;
#19993 = EDGE_CURVE ( 'NONE', #35883, #32059, #9474, .T. ) ;
#19994 = CYLINDRICAL_SURFACE ( 'NONE', #24294, 0.1000000000000028644 ) ;
#19995 = DIRECTION ( 'NONE',  ( 0.000000000000000000, -1.000000000000000000, 0.000000000000000000 ) ) ;
#19996 = CARTESIAN_POINT ( 'NONE',  ( 81.97757951650707753, 62.12693032551453598, 1.780213741554580453 ) ) ;
#19997 = CARTESIAN_POINT ( 'NONE',  ( -38.34874870218063592, -25.49307895267003587, 6.700000000000000178 ) ) ;
#19998 = CARTESIAN_POINT ( 'NONE',  ( 33.87650332550894916, -5.319205609767368337, 2.014658837789633949 ) ) ;
#19999 = CARTESIAN_POINT ( 'NONE',  ( 2.256618981523600631, -26.21573644513852841, 7.712764235869103757 ) ) ;
#20000 = CARTESIAN_POINT ( 'NONE',  ( -69.92837670882107659, -20.78299143688747819, 9.949874371066202983 ) ) ;
#20001 = VECTOR ( 'NONE', #13229, 1000.000000000000000 ) ;
#20002 = LINE ( 'NONE', #35673, #30085 ) ;
#20003 = DIRECTION ( 'NONE',  ( -0.6427876096865328126, -0.7660444431189835646, -0.000000000000000000 ) ) ;
#20004 = CARTESIAN_POINT ( 'NONE',  ( 3.939786388318850641, -26.88011527646091992, 7.635761828346575797 ) ) ;
#20005 = CARTESIAN_POINT ( 'NONE',  ( 27.67015415078466845, 1.632010242488362239, -4.348995382990432645 ) ) ;
#20006 = AXIS2_PLACEMENT_3D ( 'NONE', #2497, #25114, #37644 ) ;
#20007 = CARTESIAN_POINT ( 'NONE',  ( 1.138852870224363656, -32.92323963771860207, 7.730758795053805699 ) ) ;
#20008 = CARTESIAN_POINT ( 'NONE',  ( 4.708129185550455453, -31.35978672175994930, 6.880608371227951992 ) ) ;
#20009 = CARTESIAN_POINT ( 'NONE',  ( -1.799554507848646789, -29.58965135258283041, 7.746913345081743785 ) ) ;
#20010 = CARTESIAN_POINT ( 'NONE',  ( -63.63850063552979464, 44.01514332744383040, -2.406330881576853820 ) ) ;
#20011 = CARTESIAN_POINT ( 'NONE',  ( 22.03819786145127324, -11.49891975756862905, -2.500000000000000444 ) ) ;
#20012 = DIRECTION ( 'NONE',  ( 1.000000000000000000, 0.000000000000000000, 0.000000000000000000 ) ) ;
#20013 = EDGE_LOOP ( 'NONE', ( #9803, #37290, #32457, #24919 ) ) ;
#20014 = CARTESIAN_POINT ( 'NONE',  ( 35.61922268405216130, -1.517313264732231826, 5.701820347972824443 ) ) ;
#20015 = CARTESIAN_POINT ( 'NONE',  ( -64.08758708074093136, 38.76906266698302517, -3.000000000000000000 ) ) ;
#20016 = CARTESIAN_POINT ( 'NONE',  ( 67.21949607617069944, 57.87245792367627928, -3.992323350375291291 ) ) ;
#20017 = DIRECTION ( 'NONE',  ( 1.000000000000000000, 0.000000000000000000, -0.000000000000000000 ) ) ;
#20018 = VECTOR ( 'NONE', #7450, 1000.000000000000000 ) ;
#20019 = EDGE_LOOP ( 'NONE', ( #17314, #38105, #18239, #35835, #17929 ) ) ;
#20020 = CIRCLE ( 'NONE', #22010, 0.1000000000000028644 ) ;
#20021 = CARTESIAN_POINT ( 'NONE',  ( -1.494034067973715851, -31.01676265601582827, 7.501983001166817822 ) ) ;
#20022 = CARTESIAN_POINT ( 'NONE',  ( -1.596034042910392747, -28.39366076309272202, 7.743886751744253338 ) ) ;
#20023 = CARTESIAN_POINT ( 'NONE',  ( 84.68233004218363646, 2.293814140821111014, -4.096401400287722261 ) ) ;
#20024 = CARTESIAN_POINT ( 'NONE',  ( 0.4886831474300012412, -26.28636952045412301, 7.638132480492516585 ) ) ;
#20025 = CARTESIAN_POINT ( 'NONE',  ( -1.465062676656003982, -28.32899958033718590, 6.870716933885663735 ) ) ;
#20026 = CARTESIAN_POINT ( 'NONE',  ( 0.3427083762866449668, -32.79587364754041090, 7.010186378901971160 ) ) ;
#20027 = CARTESIAN_POINT ( 'NONE',  ( 4.400537936023037666, -31.79685841314351080, 7.660770905198780234 ) ) ;
#20028 = ORIENTED_EDGE ( 'NONE', *, *, #39934, .T. ) ;
#20029 = CARTESIAN_POINT ( 'NONE',  ( 21.71407365845957216, 6.310579482064422763, 3.199499156096070163 ) ) ;
#20030 = PLANE ( 'NONE',  #25446 ) ;
#20031 = AXIS2_PLACEMENT_3D ( 'NONE', #50, #31948, #22877 ) ;
#20032 = CARTESIAN_POINT ( 'NONE',  ( 80.30248525907988721, 64.25517361537380623, 3.614389211669656543 ) ) ;
#20033 = CARTESIAN_POINT ( 'NONE',  ( -63.08758708074093136, 41.04287353446839148, 4.000000000000000000 ) ) ;
#20034 = EDGE_LOOP ( 'NONE', ( #17890, #7386 ) ) ;
#20035 = CARTESIAN_POINT ( 'NONE',  ( 79.57354641881573798, 61.78191946445392091, -3.317372267376139661 ) ) ;
#20036 = B_SPLINE_CURVE_WITH_KNOTS ( 'NONE', 3,
 ( #40122, #27567, #39503, #24474, #37031, #33977, #5752, #18291, #33147, #4931 ),
 .UNSPECIFIED., .F., .F.,
 ( 4, 3, 3, 4 ),
 ( 0.0002170292169044788736, 0.0002420761345915969052, 0.0002723302478206991186, 0.0002816811360866808668 ),
 .UNSPECIFIED. ) ;
#20038 = CARTESIAN_POINT ( 'NONE',  ( -1.721192392427412843, -28.83312752697541015, 6.869019495930281494 ) ) ;
#20037 = CARTESIAN_POINT ( 'NONE',  ( 24.74144660671096929, 0.6009092516020706487, 4.778017222739464387 ) ) ;
#20039 = CARTESIAN_POINT ( 'NONE',  ( 80.25728969399251866, 65.34460247849949610, -3.089171411835852865 ) ) ;
#20040 = CARTESIAN_POINT ( 'NONE',  ( 80.18735707129573598, 62.48858554017570555, 3.489618106120242036 ) ) ;
#20041 = B_SPLINE_CURVE_WITH_KNOTS ( 'NONE', 3,
 ( #27180, #36452, #4960, #35864, #8030, #32971, #4756 ),
 .UNSPECIFIED., .F., .F.,
 ( 4, 3, 4 ),
 ( 0.006764200096651864190, 0.007395461704374725088, 0.007885996417624047475 ),
 .UNSPECIFIED. ) ;
#20042 = EDGE_CURVE ( 'NONE', #33142, #3556, #25425, .T. ) ;
#20043 = CARTESIAN_POINT ( 'NONE',  ( 6.366197675807956813, -31.52662935008911660, 6.894806418505347700 ) ) ;
#20044 = EDGE_CURVE ( 'NONE', #29402, #863, #28557, .T. ) ;
#20045 = ORIENTED_EDGE ( 'NONE', *, *, #3905, .T. ) ;
#20046 = CARTESIAN_POINT ( 'NONE',  ( 82.25590015743745198, 64.89408798057375805, 1.328060019257126356 ) ) ;
#20048 = ORIENTED_EDGE ( 'NONE', *, *, #26551, .T. ) ;
#20047 = CARTESIAN_POINT ( 'NONE',  ( -64.08758708074095978, 44.07191801957395683, 1.393174556440925249 ) ) ;
#20049 = CARTESIAN_POINT ( 'NONE',  ( 25.40259394636483137, -3.746514978370850457, -4.387842602613081233 ) ) ;
#20050 = DIRECTION ( 'NONE',  ( -0.9267318687906771491, 0.3757233601570964532, 0.000000000000000000 ) ) ;
#20051 = ORIENTED_EDGE ( 'NONE', *, *, #27237, .T. ) ;
#20052 = CARTESIAN_POINT ( 'NONE',  ( -76.75188302604665580, -5.916639119592683294, 8.138648572045363849 ) ) ;
#20053 = CARTESIAN_POINT ( 'NONE',  ( 23.59259267867648191, 0.4263748119163079386, -5.522675619391560708 ) ) ;
#20054 = CARTESIAN_POINT ( 'NONE',  ( -28.44874870218064444, -25.49307895267003587, 6.700000000000000178 ) ) ;
#20055 = AXIS2_PLACEMENT_3D ( 'NONE', #1851, #17657, #21180 ) ;
#20056 = CIRCLE ( 'NONE', #2320, 1.000000000000000888 ) ;
#20057 = CARTESIAN_POINT ( 'NONE',  ( 21.79480611247224786, 6.321165038070731157, 2.729589078629726551 ) ) ;
#20058 = ORIENTED_EDGE ( 'NONE', *, *, #35541, .F. ) ;
#20059 = CARTESIAN_POINT ( 'NONE',  ( 36.68492070182102083, -1.915863264778755237, -5.803701069252491962 ) ) ;
#20060 = FILL_AREA_STYLE_COLOUR ( '', #6254 ) ;
#20061 = VECTOR ( 'NONE', #11820, 1000.000000000000000 ) ;
#20062 = CARTESIAN_POINT ( 'NONE',  ( -2.995288454638185272, -28.68415433521490954, 7.013842709614101167 ) ) ;
#20063 = CARTESIAN_POINT ( 'NONE',  ( -64.94969918204330384, 34.86787045525706219, -6.612452343231766783 ) ) ;
#20064 = DIRECTION ( 'NONE',  ( 0.000000000000000000, -0.000000000000000000, -1.000000000000000000 ) ) ;
#20065 = CARTESIAN_POINT ( 'NONE',  ( -79.95330471031414277, 33.71485196875532608, 21.52833696633422988 ) ) ;
#20066 = AXIS2_PLACEMENT_3D ( 'NONE', #35046, #25964, #9903 ) ;
#20067 = CARTESIAN_POINT ( 'NONE',  ( -30.24874870218063805, -26.64985754041175525, 6.800000000000000711 ) ) ;
#20068 = VERTEX_POINT ( 'NONE', #18615 ) ;
#20069 =( BOUNDED_SURFACE ( )  B_SPLINE_SURFACE ( 3, 2, ( 
 ( #31314, #431, #12559 ),
 ( #9462, #9677, #16257 ),
 ( #6399, #22856, #12971 ),
 ( #38279, #28829, #220 ) ),
 .UNSPECIFIED., .F., .F., .T. ) 
 B_SPLINE_SURFACE_WITH_KNOTS ( ( 4, 4 ),
 ( 3, 3 ),
 ( 0.000000000000000000, 0.0008754244208269470464 ),
 ( 0.000000000000000000, 1.000000000000000000 ),
 .UNSPECIFIED. ) 
 GEOMETRIC_REPRESENTATION_ITEM ( )  RATIONAL_B_SPLINE_SURFACE ( (
 ( 1.000000000000000000, 0.9970051441236887912, 1.000000000000000000),
 ( 1.000000000000000000, 0.9987001331027990370, 1.000000000000000000),
 ( 1.000000000000000000, 0.9999578578055167144, 1.000000000000000000),
 ( 1.000000000000000000, 1.000000000000000000, 1.000000000000000000) ) ) 
 REPRESENTATION_ITEM ( '' )  SURFACE ( )  );
#20070 = CARTESIAN_POINT ( 'NONE',  ( 66.87706763805377363, 57.90143666482605056, 3.999241724014405364 ) ) ;
#20071 = CARTESIAN_POINT ( 'NONE',  ( 71.19973236181560594, 58.84349373463830091, -3.887826097256417146 ) ) ;
#20072 = CARTESIAN_POINT ( 'NONE',  ( 84.85978623402763787, 2.253055191119315737, -4.296636491436513161 ) ) ;
#20073 = B_SPLINE_SURFACE_WITH_KNOTS ( 'NONE', 5, 3, ( 
 ( #38319, #22704, #35272, #19607, #13619, #26194, #3978, #29074, #38726, #35668, #39534, #17907, #29871, #39948, #30489, #20801, #2295, #33394, #4963, #20591, #10923, #26987, #39743, #14419, #11315, #39126, #11724, #14821, #23881, #33176, #36657, #4759, #11522, #36256, #1897, #30280, #29669, #32974, #8436, #30082, #17293, #36455, #39331, #8230, #14015, #35867, #27387, #7645 ),
 ( #5166, #20194, #17702, #14217, #2095, #32780, #1687, #14611, #36066, #23499, #27183, #24089, #26792, #21018, #20392, #33595, #11121, #4569, #5369, #23690, #17096, #1481, #26587, #8033, #7844, #17489, #24715, #21633, #37462, #33791, #37658, #18947, #34214, #217, #2919, #27790, #3336, #30704, #18733, #24926, #5984, #9460, #31107, #9258, #15853, #15440, #12556, #28410 ),
 ( #28000, #40543, #21838, #15652, #18523, #2510, #31312, #3135, #34415, #12354, #6188, #22046, #28198, #27595, #31512, #28, #25128, #21220, #24506, #34623, #30908, #37058, #6396, #24299, #36860, #8645, #11930, #5571, #18110, #15034, #37263, #40148, #8846, #21431, #34005, #5779, #18317, #2716, #15237, #40345, #12140, #9056, #1040, #12757, #22455, #32138, #31714, #9674 ),
 ( #19947, #10475, #832, #3938, #29029, #25336, #35225, #16847, #37870, #3530, #22259, #429, #16054, #35024, #633, #35426, #10276, #28625, #34827, #38079, #13174, #6603, #38678, #25734, #19148, #6798, #12969, #4326, #25535, #9881, #19352, #13363, #7393, #16455, #25938, #31924, #22657, #3732, #23056, #38277, #22854, #28827, #32526, #7195, #10073, #6997, #13572, #19562 ),
 ( #38472, #26144, #19755, #32333, #16642, #29227, #35621, #36406, #11265, #8386, #39685, #30027, #33125, #17437, #17854, #23638, #5320, #1243, #32728, #13779, #29623, #20148, #10872, #29818, #23829, #39478, #4524, #10671, #26538, #1630, #23252, #27134, #14169, #7596, #23448, #17044, #33544, #1437, #35818, #8177, #20343, #20749, #26347, #36013, #5114, #13970, #39073, #17650 ),
 ( #36205, #7791, #30231, #32922, #38880, #2045, #4713, #14559, #17246, #11469, #26741, #4905, #24037, #39280, #11068, #14365, #7984, #36608, #20963, #20540, #1842, #26933, #33953, #9408, #36810, #24874, #31057, #12086, #15600, #37212, #2868, #21996, #21585, #18679, #34573, #37612, #9005, #34167, #5933, #15391, #21789, #24660, #8595, #37413, #9209, #27947, #18472, #40489 ),
 ( #5728, #12301, #21173, #6347, #12507, #30435, #24453, #8792, #34367, #2245, #37010, #6137, #30651, #33738, #31264, #3081, #21374, #28152, #14984, #40706, #40097, #14766, #25082, #18266, #27338, #39898, #11672, #30858, #24246, #5518, #2665, #27743, #18060, #2463, #27544, #11878, #40296, #15184, #38227, #22407, #38633, #25286, #13313, #19510, #586, #4083, #25684, #32085 ),
 ( #7148, #23007, #26095, #10024, #22607, #35175, #3890, #10226, #13125, #37817, #25886, #38425, #16405, #6948, #28979, #16597, #22809, #22209, #13524, #783, #35379, #15809, #19099, #19708, #25483, #31668, #32283, #10432, #29179, #988, #6554, #28779, #35574, #18897, #19302, #31464, #28363, #3287, #176, #12712, #381, #9622, #34776, #3484, #16009, #28574, #12917, #38029 ) ),
 .UNSPECIFIED., .F., .T., .F.,
 ( 6, 2, 6 ),
 ( 4, 1, 1, 1, 1, 1, 1, 1, 1, 1, 1, 1, 1, 1, 1, 1, 1, 1, 1, 1, 1, 1, 1, 1, 1, 1, 1, 1, 1, 1, 1, 1, 1, 1, 1, 1, 1, 1, 1, 1, 1, 1, 1, 1, 1, 4 ),
 ( 0.000000000000000000, 0.5000000000000000000, 1.000000000000000000 ),
 ( 0.02319993227479018663, 0.02338707809474536645, 0.02357422391470053238, 0.02376136973465571220, 0.02401089749459594039, 0.02432280719452123083, 0.02469709883443158005, 0.02507139047434192580, 0.02557044599422238565, 0.02619426539407297347, 0.02694284867389366844, 0.02769143195371436342, 0.02844001523353506186, 0.02918859851335575684, 0.02993718179317645181, 0.03068576507299715025, 0.03143434835281785217, 0.03218293163263854367, 0.03293151491245924212, 0.03355533431230981606, 0.03405438983219027937, 0.03442868147210063207, 0.03480297311201098476, 0.03511488281193627520, 0.03536441057187650339, 0.03555155639183167626, 0.03573870221178684914, 0.03598822997172709121, 0.03630013967165238165, 0.03667443131156272740, 0.03704872295147307315, 0.03754777847135353647, 0.03817159787120411735, 0.03892018115102481579, 0.03966876443084551424, 0.04041734771066620574, 0.04141545875042713931, 0.04241356979018806594, 0.04341168082994899952, 0.04416026410976969102, 0.04490884738959038947, 0.04553266678944096341, 0.04603172230932142672, 0.04640601394923177248, 0.04678030558914212517, 0.04715459722905247786 ),
 .UNSPECIFIED. ) ;
#20074 = CARTESIAN_POINT ( 'NONE',  ( -80.26960040814950048, 10.48563383736161114, -5.954513432128944572 ) ) ;
#20075 = APPLICATION_PROTOCOL_DEFINITION ( 'draft international standard', 'automotive_design', 1998, #25032 ) ;
#20076 = CARTESIAN_POINT ( 'NONE',  ( 3.005752271882382587, -26.32336525051885090, 7.761113333116789192 ) ) ;
#20077 = DIRECTION ( 'NONE',  ( 0.4999999999999927836, 0.8660254037844429265, 0.000000000000000000 ) ) ;
#20078 = ORIENTED_EDGE ( 'NONE', *, *, #6153, .T. ) ;
#20079 = CARTESIAN_POINT ( 'NONE',  ( -1.749215324041719422, -28.97813421761779296, 7.638991368224663958 ) ) ;
#20080 = VECTOR ( 'NONE', #24045, 1000.000000000000000 ) ;
#20081 = AXIS2_PLACEMENT_3D ( 'NONE', #38860, #10254, #39051 ) ;
#20082 = ORIENTED_EDGE ( 'NONE', *, *, #16324, .F. ) ;
#20083 = CARTESIAN_POINT ( 'NONE',  ( 80.75607764207482830, 61.50646045904603199, -2.414331286641652419 ) ) ;
#20084 = CARTESIAN_POINT ( 'NONE',  ( 36.96348058853109819, -2.193283099190300511, 5.898309123131363130 ) ) ;
#20085 = CARTESIAN_POINT ( 'NONE',  ( 79.20958446297085231, 65.00485465208082303, 3.275607309966509284 ) ) ;
#20086 = CARTESIAN_POINT ( 'NONE',  ( -17.27251170661583402, -8.656638842136340273, 6.000000000000000000 ) ) ;
#20087 = PLANE ( 'NONE',  #13995 ) ;
#20088 = EDGE_CURVE ( 'NONE', #37655, #5466, #24580, .T. ) ;
#20089 = CARTESIAN_POINT ( 'NONE',  ( 3.995286705358532586, -27.06125532609220485, 6.868387053540521592 ) ) ;
#20090 = CYLINDRICAL_SURFACE ( 'NONE', #32757, 0.09010775117052950700 ) ;
#20091 = CARTESIAN_POINT ( 'NONE',  ( 33.79284613923667990, -4.878148420886379455, -3.390896070728523615 ) ) ;
#20092 = VERTEX_POINT ( 'NONE', #12452 ) ;
#20093 = CARTESIAN_POINT ( 'NONE',  ( -1.238631071793920509E-17, 0.000000000000000000, 0.000000000000000000 ) ) ;
#20094 = CYLINDRICAL_SURFACE ( 'NONE', #27398, 1.000000000000000000 ) ;
#20095 = CARTESIAN_POINT ( 'NONE',  ( -72.17666250106589132, -0.4381958982661475765, -9.922884124630229508 ) ) ;
#20096 = CARTESIAN_POINT ( 'NONE',  ( -0.03065438358791758300, -26.64358689880297248, 7.695279973900954751 ) ) ;
#20097 = CARTESIAN_POINT ( 'NONE',  ( -17.69482985384421880, -29.56993018339339940, 6.000000000000000000 ) ) ;
#20098 = CARTESIAN_POINT ( 'NONE',  ( 80.61469348477540109, 64.03810969304559819, 3.562450064734659527 ) ) ;
#20099 = CARTESIAN_POINT ( 'NONE',  ( -1.486040044270929616, -30.75597321790062821, 7.740055089680402567 ) ) ;
#20100 = FACE_OUTER_BOUND ( 'NONE', #14172, .T. ) ;
#20101 = CARTESIAN_POINT ( 'NONE',  ( -1.281659060280029294, -27.76124872452957604, 7.782861076432732617 ) ) ;
#20102 = CARTESIAN_POINT ( 'NONE',  ( -1.641531228027346412, -30.19567924397617631, 7.692469944509197965 ) ) ;
#20103 = AXIS2_PLACEMENT_3D ( 'NONE', #2592, #12435, #40029 ) ;
#20104 = B_SPLINE_CURVE_WITH_KNOTS ( 'NONE', 3,
 ( #14203, #38507, #10308, #8020, #20182, #4555, #23484, #36051, #4745, #35851 ),
 .UNSPECIFIED., .F., .F.,
 ( 4, 3, 3, 4 ),
 ( 8.940560153363745023E-19, 3.025570593003372205E-05, 6.051145698343924614E-05, 6.468151674593483288E-05 ),
 .UNSPECIFIED. ) ;
#20105 = CARTESIAN_POINT ( 'NONE',  ( -64.12095013931764242, 35.34012592920250739, 4.384900748508816726 ) ) ;
#20106 = DIRECTION ( 'NONE',  ( 0.000000000000000000, 0.000000000000000000, 1.000000000000000000 ) ) ;
#20107 = CARTESIAN_POINT ( 'NONE',  ( 5.013900471082111565, -30.36275040796179425, 7.386948897581450346 ) ) ;
#20108 = CARTESIAN_POINT ( 'NONE',  ( -1.003736583562490070, -27.34783681995376270, 7.695279973900954751 ) ) ;
#20109 = CARTESIAN_POINT ( 'NONE',  ( 35.86903479493524571, -2.086569765857306358, 5.804628394271051484 ) ) ;
#20110 = EDGE_CURVE ( 'NONE', #6415, #16350, #21934, .T. ) ;
#20111 = AXIS2_PLACEMENT_3D ( 'NONE', #37313, #31156, #28462 ) ;
#20112 = CARTESIAN_POINT ( 'NONE',  ( -64.08758708074093136, 43.61223004741322740, -1.000000000000000000 ) ) ;
#20113 = CARTESIAN_POINT ( 'NONE',  ( 84.82990711808488982, 3.023024660489734394, 1.086629044751433293 ) ) ;
#20114 = CARTESIAN_POINT ( 'NONE',  ( 79.28289924135638955, 65.69038102574751292, -2.688322534164182542 ) ) ;
#20115 = EDGE_CURVE ( 'NONE', #486, #9636, #9738, .T. ) ;
#20116 = CARTESIAN_POINT ( 'NONE',  ( 4.370230286903631800, -27.30675615745736806, 7.640616322432101981 ) ) ;
#20117 = CARTESIAN_POINT ( 'NONE',  ( -58.98400447371446376, 28.74159977738611715, 6.613141227606677219 ) ) ;
#20118 = ORIENTED_EDGE ( 'NONE', *, *, #6943, .F. ) ;
#20119 = CARTESIAN_POINT ( 'NONE',  ( -80.93510526298557295, 11.45401881227207497, 0.2075866020563601477 ) ) ;
#20120 = CARTESIAN_POINT ( 'NONE',  ( 24.86584501937821301, -5.834624453299285030, -2.864450365913323360 ) ) ;
#20121 = ORIENTED_EDGE ( 'NONE', *, *, #12229, .T. ) ;
#20122 = CARTESIAN_POINT ( 'NONE',  ( 5.628486912222185445, -26.20317660986373909, 7.695279973900954751 ) ) ;
#20123 = EDGE_CURVE ( 'NONE', #31083, #28028, #10790, .T. ) ;
#20125 = EDGE_LOOP ( 'NONE', ( #34254, #29653, #3337, #29341, #37871 ) ) ;
#20124 = ORIENTED_EDGE ( 'NONE', *, *, #32336, .T. ) ;
#20126 = CARTESIAN_POINT ( 'NONE',  ( 79.95665241583039062, 64.06168528317456889, -3.692178340560190897 ) ) ;
#20127 = CARTESIAN_POINT ( 'NONE',  ( -17.27251170661583402, -8.656638842136340273, 6.000000000000000000 ) ) ;
#20128 = CARTESIAN_POINT ( 'NONE',  ( 80.78100857081943786, 62.68361397997274054, 3.372125408468113594 ) ) ;
#20129 = CARTESIAN_POINT ( 'NONE',  ( 24.10439548121549436, 0.6331765145075038959, 5.082944852415793413 ) ) ;
#20130 = ORIENTED_EDGE ( 'NONE', *, *, #19771, .F. ) ;
#20131 = CARTESIAN_POINT ( 'NONE',  ( -1.614537886288068158, -25.59834652758622653, 7.635761828346577573 ) ) ;
#20132 = CARTESIAN_POINT ( 'NONE',  ( 0.02181676014757850252, -32.52668967079699769, 7.740055089680399902 ) ) ;
#20133 = EDGE_CURVE ( 'NONE', #19316, #29188, #3432, .T. ) ;
#20135 = CARTESIAN_POINT ( 'NONE',  ( 85.76501473881677384, 2.022389388904533902, 3.835323685118464443 ) ) ;
#20134 = CARTESIAN_POINT ( 'NONE',  ( 63.05383694556373797, -7.271989087314214117, 6.000000000000000000 ) ) ;
#20136 = CARTESIAN_POINT ( 'NONE',  ( 0.04278369059588756074, -26.60137143983851615, 6.894806418505345924 ) ) ;
#20137 = CARTESIAN_POINT ( 'NONE',  ( -64.08758708074093136, 42.48851732723078811, -2.660621165554523326 ) ) ;
#20138 = CYLINDRICAL_SURFACE ( 'NONE', #35727, 0.1000000000000028644 ) ;
#20139 = CARTESIAN_POINT ( 'NONE',  ( 22.68981863355961082, 4.343343972393600261, -3.284089849446835352 ) ) ;
#20140 = ORIENTED_EDGE ( 'NONE', *, *, #480, .T. ) ;
#20141 = CARTESIAN_POINT ( 'NONE',  ( 5.122500503061667487, -30.26926087503160190, 7.776484688137387025 ) ) ;
#20142 = AXIS2_PLACEMENT_3D ( 'NONE', #5161, #14606, #26786 ) ;
#20143 = CARTESIAN_POINT ( 'NONE',  ( 22.75155763331752112, -5.137713618528696458, -6.528071535057289765 ) ) ;
#20144 = CARTESIAN_POINT ( 'NONE',  ( 21.83106932671411471, 5.061056560965798035, 3.908462188293328587 ) ) ;
#20145 = CARTESIAN_POINT ( 'NONE',  ( 20.41154445963425701, 10.73873515079988294, 2.500000000000000444 ) ) ;
#20146 = CARTESIAN_POINT ( 'NONE',  ( 0.3487507780706524674, -32.68971722127069768, 6.988553391373221402 ) ) ;
#20147 = CARTESIAN_POINT ( 'NONE',  ( 81.55137728095093053, 62.42468454963330515, 2.710336141772879959 ) ) ;
#20148 = CARTESIAN_POINT ( 'NONE',  ( 85.36258410344761671, 2.204690851838579047, 4.549306268726941660 ) ) ;
#20149 = CARTESIAN_POINT ( 'NONE',  ( -0.5005001391084890061, -26.97838111740712463, 7.643333865083954848 ) ) ;
#20150 = ORIENTED_EDGE ( 'NONE', *, *, #24932, .F. ) ;
#20151 = ADVANCED_FACE ( 'NONE', ( #35517 ), #23434, .T. ) ;
#20152 = CARTESIAN_POINT ( 'NONE',  ( 23.84450253662037866, -2.668400562688592714, 3.927909320949413807 ) ) ;
#20153 = DIRECTION ( 'NONE',  ( 1.000000000000000000, -0.000000000000000000, 0.000000000000000000 ) ) ;
#20154 = CARTESIAN_POINT ( 'NONE',  ( 35.78593763082197654, -3.161148606490439050, -5.791659072098707561 ) ) ;
#20155 = LINE ( 'NONE', #13580, #8213 ) ;
#20156 = CARTESIAN_POINT ( 'NONE',  ( 84.48228160770625550, 2.547494559575964157, -3.385513399219323372 ) ) ;
#20157 = DIRECTION ( 'NONE',  ( 0.000000000000000000, 1.000000000000000000, 0.000000000000000000 ) ) ;
#20158 = LINE ( 'NONE', #4139, #3358 ) ;
#20159 = DIRECTION ( 'NONE',  ( -0.000000000000000000, -1.000000000000000000, -0.000000000000000000 ) ) ;
#20160 = AXIS2_PLACEMENT_3D ( 'NONE', #14514, #27088, #1580 ) ;
#20161 = CARTESIAN_POINT ( 'NONE',  ( -1.133858823486877165, -27.69188849431729693, 6.939395833800444002 ) ) ;
#20162 = ORIENTED_EDGE ( 'NONE', *, *, #34538, .F. ) ;
#20163 = VERTEX_POINT ( 'NONE', #19851 ) ;
#20164 = CARTESIAN_POINT ( 'NONE',  ( 36.49352434727311589, -3.559963790946740758, 5.796433071289773586 ) ) ;
#20165 = CARTESIAN_POINT ( 'NONE',  ( 16.40512227804392609, -3.237279488405499617, 2.766814109507098163 ) ) ;
#20166 = EDGE_CURVE ( 'NONE', #7424, #20092, #17885, .T. ) ;
#20167 = CIRCLE ( 'NONE', #21511, 0.9999999999999996669 ) ;
#20168 = ADVANCED_FACE ( 'NONE', ( #10573 ), #23147, .T. ) ;
#20169 = CARTESIAN_POINT ( 'NONE',  ( 66.27376694609004915, 57.73522568913436004, -4.000000000000000000 ) ) ;
#20170 = CARTESIAN_POINT ( 'NONE',  ( 86.05032028231427432, 0.1565332958781914807, 6.000000348367978908 ) ) ;
#20171 = ADVANCED_FACE ( 'NONE', ( #11368 ), #24350, .F. ) ;
#20172 = ORIENTED_EDGE ( 'NONE', *, *, #28208, .T. ) ;
#20173 = ORIENTED_EDGE ( 'NONE', *, *, #29343, .F. ) ;
#20174 = DIRECTION ( 'NONE',  ( -0.000000000000000000, -1.000000000000000000, -0.000000000000000000 ) ) ;
#20175 = EDGE_LOOP ( 'NONE', ( #17856, #25144, #37903, #25853, #2038 ) ) ;
#20176 = CARTESIAN_POINT ( 'NONE',  ( -57.13133194381637736, 29.70675091384814337, -4.151468609674966004 ) ) ;
#20178 = CARTESIAN_POINT ( 'NONE',  ( 1.700390093233090871, -29.56993018339339940, 7.750000000000000888 ) ) ;
#20177 = DIRECTION ( 'NONE',  ( -0.9975640502598243087, 0.06975647374412531632, 0.000000000000000000 ) ) ;
#20179 = ORIENTED_EDGE ( 'NONE', *, *, #37591, .T. ) ;
#20180 = CARTESIAN_POINT ( 'NONE',  ( 24.25095726714989297, 3.112089687977687369, 3.515329813937853043 ) ) ;
#20181 = CARTESIAN_POINT ( 'NONE',  ( 79.30570723442072278, 66.28915683679505833, -1.250621450094244080 ) ) ;
#20182 = CARTESIAN_POINT ( 'NONE',  ( -1.227373324201784355, -31.29857579714354898, 7.670860738520331346 ) ) ;
#20183 = ORIENTED_EDGE ( 'NONE', *, *, #24404, .T. ) ;
#20184 = DIRECTION ( 'NONE',  ( -0.000000000000000000, 1.000000000000000000, -0.000000000000000000 ) ) ;
#20185 = DIRECTION ( 'NONE',  ( 0.000000000000000000, 0.000000000000000000, 1.000000000000000000 ) ) ;
#20186 = CARTESIAN_POINT ( 'NONE',  ( 76.81167355577598244, 60.15069890908834083, 3.230144225296844418 ) ) ;
#20187 = CARTESIAN_POINT ( 'NONE',  ( 23.19159090904956599, 2.549548122309488907, -4.431069449850736142 ) ) ;
#20188 = CARTESIAN_POINT ( 'NONE',  ( -0.8786759135921904385, -26.64985754041175525, 6.700000000000000178 ) ) ;
#20189 = CARTESIAN_POINT ( 'NONE',  ( 16.13271431945180723, 15.26109421794535059, -1.496401833041691720 ) ) ;
#20190 = CARTESIAN_POINT ( 'NONE',  ( 24.38023270008697097, 2.574825574644751924, -4.011522969641340808 ) ) ;
#20191 = LINE ( 'NONE', #26583, #40668 ) ;
#20192 = DIRECTION ( 'NONE',  ( -0.000000000000000000, -0.000000000000000000, -1.000000000000000000 ) ) ;
#20193 = CARTESIAN_POINT ( 'NONE',  ( 81.76431320972403682, 64.63772642544205382, 2.665107514500538066 ) ) ;
#20194 = CARTESIAN_POINT ( 'NONE',  ( 87.05466826895010968, 0.5737893332097195875, -5.097061431219924721 ) ) ;
#20195 = CARTESIAN_POINT ( 'NONE',  ( 31.96905077431594933, -4.633974458378385286, -3.035954366531696369 ) ) ;
#20196 = AXIS2_PLACEMENT_3D ( 'NONE', #18033, #39655, #2214 ) ;
#20197 = LINE ( 'NONE', #1291, #24041 ) ;
#20198 = AXIS2_PLACEMENT_3D ( 'NONE', #14066, #10973, #33026 ) ;
#20199 = CARTESIAN_POINT ( 'NONE',  ( -64.85784325972052500, 34.81586596186941307, 6.466735817496045868 ) ) ;
#20200 = AXIS2_PLACEMENT_3D ( 'NONE', #21099, #40225, #12007 ) ;
#20201 = CARTESIAN_POINT ( 'NONE',  ( -81.33601108014657655, -5.640736238038894790, -3.433968290496116182 ) ) ;
#20202 = CARTESIAN_POINT ( 'NONE',  ( 0.6935492931484148471, -26.32241729325343016, 6.876076431790004939 ) ) ;
#20203 = CARTESIAN_POINT ( 'NONE',  ( 0.05125347100749116230, -26.48280394670751647, 6.865482280155369210 ) ) ;
#20204 = CARTESIAN_POINT ( 'NONE',  ( 34.13174693812651839, -3.213397211757874850, -5.533482607768558381 ) ) ;
#20205 = CARTESIAN_POINT ( 'NONE',  ( 1.060496565001608493, -32.90918720382173746, 7.785868773668302545 ) ) ;
#20206 = DIRECTION ( 'NONE',  ( 1.000000000000000000, 0.000000000000000000, 0.000000000000000000 ) ) ;
#20207 = CARTESIAN_POINT ( 'NONE',  ( -63.24191987307168006, 41.86289664080484840, -3.933528212093161169 ) ) ;
#20208 = EDGE_CURVE ( 'NONE', #9480, #39964, #7528, .T. ) ;
#20209 = CARTESIAN_POINT ( 'NONE',  ( -0.4654086415465331639, -32.19087087841436556, 7.652160403243379427 ) ) ;
#20210 = ADVANCED_FACE ( 'NONE', ( #36707 ), #20645, .T. ) ;
#20211 = ORIENTED_EDGE ( 'NONE', *, *, #3167, .F. ) ;
#20213 = CARTESIAN_POINT ( 'NONE',  ( 36.84686803492319029, -3.231021363853832540, 5.943776631324515058 ) ) ;
#20212 = B_SPLINE_CURVE_WITH_KNOTS ( 'NONE', 3,
 ( #29944, #38598, #27068, #21301, #20886, #30366, #11193, #15112, #37138, #8927, #21510, #37342, #3004, #21914, #22333, #16133, #25605, #40631, #34490, #13851, #22928, #4785, #7267, #10549, #20025, #38348, #32806, #33203, #17516, #36888, #39559 ),
 .UNSPECIFIED., .F., .F.,
 ( 4, 3, 3, 3, 3, 3, 3, 3, 3, 3, 4 ),
 ( 0.000000000000000000, 2.999644130997770587E-05, 6.002588995694883557E-05, 8.960886084588016163E-05, 0.0001190604700446482121, 0.0001489538463052730757, 0.0001796139255493973941, 0.0002109707048517075394, 0.0002426195318110314805, 0.0002740640997890032566, 0.0002849778069099877806 ),
 .UNSPECIFIED. ) ;
#20214 = FACE_OUTER_BOUND ( 'NONE', #6972, .T. ) ;
#20215 = CARTESIAN_POINT ( 'NONE',  ( 67.16030903438456789, 58.03511467963866011, -3.999036733496184048 ) ) ;
#20216 = EDGE_CURVE ( 'NONE', #3101, #30906, #5419, .T. ) ;
#20217 = CARTESIAN_POINT ( 'NONE',  ( 3.072552236484260124, -26.35012101938563944, 6.980586498568965403 ) ) ;
#20218 = ORIENTED_EDGE ( 'NONE', *, *, #11795, .T. ) ;
#20219 = CARTESIAN_POINT ( 'NONE',  ( -1.238631071793920509E-17, 0.000000000000000000, 0.000000000000000000 ) ) ;
#20220 = CARTESIAN_POINT ( 'NONE',  ( 86.14847104707970971, -0.02438626603933686729, -5.973875385969918739 ) ) ;
#20221 = CARTESIAN_POINT ( 'NONE',  ( 78.69038500580361983, 66.05859403932463181, 1.083698948140488394 ) ) ;
#20222 = CARTESIAN_POINT ( 'NONE',  ( 5.043330201822981529, -28.53322799357174588, 7.013842709614101167 ) ) ;
#20223 = DIRECTION ( 'NONE',  ( -0.6834397476448853537, 0.000000000000000000, 0.7300069255418715208 ) ) ;
#20224 = AXIS2_PLACEMENT_3D ( 'NONE', #9287, #3165, #28230 ) ;
#20225 = CIRCLE ( 'NONE', #10934, 2.500000000000002220 ) ;
#20226 = DIRECTION ( 'NONE',  ( 1.000000000000000000, 4.956352788505163465E-15, 0.000000000000000000 ) ) ;
#20227 = ORIENTED_EDGE ( 'NONE', *, *, #14160, .F. ) ;
#20228 = CARTESIAN_POINT ( 'NONE',  ( 24.05520612681470993, 3.340626845478275264, 3.238600984571303520 ) ) ;
#20229 = CARTESIAN_POINT ( 'NONE',  ( 78.95300076920055687, 65.89750638847961284, 2.156541836018599501 ) ) ;
#20230 = CARTESIAN_POINT ( 'NONE',  ( 20.42004053729723978, -3.555855083337302158, -2.499999999979800158 ) ) ;
#20231 = ORIENTED_EDGE ( 'NONE', *, *, #15714, .F. ) ;
#20232 = CARTESIAN_POINT ( 'NONE',  ( 78.07544678589873399, 65.62285883043881540, -1.832491541757240494 ) ) ;
#20234 = FACE_OUTER_BOUND ( 'NONE', #24419, .T. ) ;
#20233 = CARTESIAN_POINT ( 'NONE',  ( 24.12423001070950690, 0.5003150286851053563, 5.094044111947246378 ) ) ;
#20235 = CARTESIAN_POINT ( 'NONE',  ( 80.97210443045602801, 64.61276409570730550, -3.292658836668131084 ) ) ;
#20236 = CARTESIAN_POINT ( 'NONE',  ( 78.95339491453125902, 64.13176242216603384, 3.627744115730410002 ) ) ;
#20237 = DIRECTION ( 'NONE',  ( 0.4999999999999980016, 0.8660254037844398178, -0.000000000000000000 ) ) ;
#20238 = CARTESIAN_POINT ( 'NONE',  ( 82.53033050081238287, 64.25366301186838314, 1.161365684106807850 ) ) ;
#20240 = ORIENTED_EDGE ( 'NONE', *, *, #37643, .F. ) ;
#20239 = DIRECTION ( 'NONE',  ( -0.000000000000000000, -0.000000000000000000, -1.000000000000000000 ) ) ;
#20241 = AXIS2_PLACEMENT_3D ( 'NONE', #20481, #7734, #4654 ) ;
#20242 = CARTESIAN_POINT ( 'NONE',  ( 28.93850508814251299, -1.888738275646064668, -5.863986819262115624 ) ) ;
#20243 = CARTESIAN_POINT ( 'NONE',  ( -64.52806261857494974, 36.37942767234955710, -5.858659361856752845 ) ) ;
#20244 = ORIENTED_EDGE ( 'NONE', *, *, #2738, .F. ) ;
#20245 = CARTESIAN_POINT ( 'NONE',  ( -75.89283711940969113, -3.900305280487442516, 10.11395962696834872 ) ) ;
#20246 = CARTESIAN_POINT ( 'NONE',  ( 24.74436007370645285, 0.5872009258416482913, -4.777575718694301088 ) ) ;
#20247 = AXIS2_PLACEMENT_3D ( 'NONE', #25788, #13415, #25582 ) ;
#20248 = CARTESIAN_POINT ( 'NONE',  ( -0.9695225508750403565, -31.83301800158153227, 7.749999999999998224 ) ) ;
#20249 = ORIENTED_EDGE ( 'NONE', *, *, #29961, .T. ) ;
#20250 = CARTESIAN_POINT ( 'NONE',  ( 36.49292402375851196, -3.557488610187057532, -5.797583871770345176 ) ) ;
#20251 = CARTESIAN_POINT ( 'NONE',  ( -63.08379346057678561, 18.80112958435940840, -9.800414904976365804 ) ) ;
#20252 = CARTESIAN_POINT ( 'NONE',  ( 3.286904077270082603, -32.68970154976867803, 6.921725064902947366 ) ) ;
#20253 = CARTESIAN_POINT ( 'NONE',  ( 5.110221463921440055, -30.35927082751544859, 6.989977667959444751 ) ) ;
#20254 = PLANE ( 'NONE',  #25881 ) ;
#20255 = CYLINDRICAL_SURFACE ( 'NONE', #31923, 0.09010775117052841066 ) ;
#20256 = DIRECTION ( 'NONE',  ( 0.000000000000000000, 0.000000000000000000, 1.000000000000000000 ) ) ;
#20257 = AXIS2_PLACEMENT_3D ( 'NONE', #26693, #32475, #11218 ) ;
#20258 = CARTESIAN_POINT ( 'NONE',  ( 21.53656876454488156, 7.496978015852163502, 2.849741189840151456 ) ) ;
#20259 = EDGE_LOOP ( 'NONE', ( #34995, #27526, #20179, #3097 ) ) ;
#20260 = CARTESIAN_POINT ( 'NONE',  ( 66.27376694608996388, 57.73522568913447373, 4.000000000000000000 ) ) ;
#20261 = CARTESIAN_POINT ( 'NONE',  ( 71.99851445618389789, 60.18445664521269123, -3.955776929956313470 ) ) ;
#20262 = EDGE_CURVE ( 'NONE', #2057, #16321, #29213, .T. ) ;
#20263 = EDGE_CURVE ( 'NONE', #10252, #38102, #39048, .T. ) ;
#20264 = ORIENTED_EDGE ( 'NONE', *, *, #10593, .T. ) ;
#20265 = CARTESIAN_POINT ( 'NONE',  ( 84.32222422711384979, 2.914578286995431977, 1.930349914595605343 ) ) ;
#20266 = EDGE_CURVE ( 'NONE', #3811, #4425, #20020, .T. ) ;
#20267 = CARTESIAN_POINT ( 'NONE',  ( 4.715819433959782536, -31.34677736058242559, 6.894806418505347700 ) ) ;
#20268 = CIRCLE ( 'NONE', #2557, 3.784187430299790211 ) ;
#20269 = DIRECTION ( 'NONE',  ( 0.9594800004753906153, 0.2817767355331954326, 0.000000000000000000 ) ) ;
#20270 = CARTESIAN_POINT ( 'NONE',  ( 2.315096682381391435, -32.91390549881585059, 7.740055089680399902 ) ) ;
#20271 = CARTESIAN_POINT ( 'NONE',  ( -34.87867591359218977, -26.64985754041175525, 6.700000000000000178 ) ) ;
#20272 = CARTESIAN_POINT ( 'NONE',  ( 2.853712549240934315, -26.25820597416272051, 7.255881584735163869 ) ) ;
#20273 = VERTEX_POINT ( 'NONE', #30542 ) ;
#20274 = CARTESIAN_POINT ( 'NONE',  ( 80.70428644432419674, 61.65645308977152439, -2.679976076788562089 ) ) ;
#20275 = CARTESIAN_POINT ( 'NONE',  ( 36.86034836333212894, -2.080661969557957125, 5.862916021703864722 ) ) ;
#20276 = CARTESIAN_POINT ( 'NONE',  ( 79.50008710437312232, 64.50769319364337662, 3.547878946066072015 ) ) ;
#20277 = DIRECTION ( 'NONE',  ( 0.3754033771448366252, -0.6502177225477857592, -0.6605219282605403475 ) ) ;
#20278 = VECTOR ( 'NONE', #27501, 1000.000000000000000 ) ;
#20279 = DIRECTION ( 'NONE',  ( 1.000000000000000000, -0.000000000000000000, 0.000000000000000000 ) ) ;
#20280 = FACE_OUTER_BOUND ( 'NONE', #17590, .T. ) ;
#20281 = CARTESIAN_POINT ( 'NONE',  ( 2.908949165453299734, -26.39197723079101010, 6.894806418505348589 ) ) ;
#20282 = CARTESIAN_POINT ( 'NONE',  ( 21.85643539959777470, 9.109670159223330899, 10.09094178405049647 ) ) ;
#20283 = DIRECTION ( 'NONE',  ( 0.000000000000000000, 1.000000000000000000, 0.000000000000000000 ) ) ;
#20284 = ORIENTED_EDGE ( 'NONE', *, *, #40617, .F. ) ;
#20285 = CARTESIAN_POINT ( 'NONE',  ( 73.85882785809795337, 62.69890035364841907, -3.253129289162608906 ) ) ;
#20286 = CARTESIAN_POINT ( 'NONE',  ( 14.66162177708395653, -4.890547631111535232, 2.500000000000003109 ) ) ;
#20287 = CARTESIAN_POINT ( 'NONE',  ( -75.52298870755240046, -5.187903949434842232, -8.883779244834281386 ) ) ;
#20288 = CLOSED_SHELL ( 'NONE', ( #23755, #36569, #16364, #12410, #13490, #22873, #31635, #590, #40530, #5293, #31195, #3619, #15618 ) ) ;
#20289 = DIRECTION ( 'NONE',  ( 1.000000000000000000, 0.000000000000000000, 0.000000000000000000 ) ) ;
#20290 = LINE ( 'NONE', #13522, #21515 ) ;
#20291 = CARTESIAN_POINT ( 'NONE',  ( 78.67160034737365493, 66.04525015085647510, 1.145133111591879471 ) ) ;
#20292 = DIRECTION ( 'NONE',  ( 0.000000000000000000, 1.000000000000000000, 0.000000000000000000 ) ) ;
#20293 =( BOUNDED_CURVE ( )  B_SPLINE_CURVE ( 3, ( #23884, #11524, #4965, #14823 ),
 .UNSPECIFIED., .F., .F. ) 
 B_SPLINE_CURVE_WITH_KNOTS ( ( 4, 4 ),
 ( 1.396263401595456477, 1.534781240595298524 ),
 .UNSPECIFIED. ) 
 CURVE ( )  GEOMETRIC_REPRESENTATION_ITEM ( )  RATIONAL_B_SPLINE_CURVE ( ( 1.000000000000000000, 0.9984017064007808528, 0.9984017064007808528, 1.000000000000000000 ) ) 
 REPRESENTATION_ITEM ( '' )  );
#20294 = FACE_OUTER_BOUND ( 'NONE', #14297, .T. ) ;
#20295 = DIRECTION ( 'NONE',  ( -0.000000000000000000, -0.000000000000000000, -1.000000000000000000 ) ) ;
#20296 = CARTESIAN_POINT ( 'NONE',  ( -1.641525177248355227, -30.19571155489859393, 7.695279973900954751 ) ) ;
#20297 = CARTESIAN_POINT ( 'NONE',  ( -69.92837670882109080, -0.6508471542538479815, 9.949874371066202983 ) ) ;
#20298 = CARTESIAN_POINT ( 'NONE',  ( 4.441298539795110578, -27.39334439880510530, 6.863805608295729499 ) ) ;
#20299 = CARTESIAN_POINT ( 'NONE',  ( 15.11713524669251107, 11.51833089347275774, -2.565792583180644293 ) ) ;
#20300 = DIRECTION ( 'NONE',  ( 0.000000000000000000, -0.000000000000000000, -1.000000000000000000 ) ) ;
#20301 = CARTESIAN_POINT ( 'NONE',  ( 4.190466207346752903, -31.88499410171630188, 6.882085323592687764 ) ) ;
#20302 = CARTESIAN_POINT ( 'NONE',  ( 67.76947924466990969, 58.18518750870053680, 3.996132678073308853 ) ) ;
#20303 = CARTESIAN_POINT ( 'NONE',  ( 36.99348654919808155, -2.718276929309134449, 5.980126285492262994 ) ) ;
#20304 = ORIENTED_EDGE ( 'NONE', *, *, #27883, .F. ) ;
#20305 = DIRECTION ( 'NONE',  ( -0.000000000000000000, -1.000000000000000000, -0.000000000000000000 ) ) ;
#20306 = CARTESIAN_POINT ( 'NONE',  ( 88.66415851257785619, -1.234066499448195131, -0.8261491842984883816 ) ) ;
#20307 = EDGE_CURVE ( 'NONE', #18355, #10861, #36914, .T. ) ;
#20309 = CARTESIAN_POINT ( 'NONE',  ( 4.820177131110392921, -30.92156949855583292, 6.988553391373219625 ) ) ;
#20308 = CARTESIAN_POINT ( 'NONE',  ( 80.54296318544950850, 63.62250603730376497, -3.633989118465182688 ) ) ;
#20310 = PRODUCT ( 'Hinge', 'Hinge', '', ( #20468 ) ) ;
#20311 = CARTESIAN_POINT ( 'NONE',  ( 4.369049338451901576, -27.30536447825076252, 7.643192810543822269 ) ) ;
#20312 = CARTESIAN_POINT ( 'NONE',  ( 2.408393318269669514, -26.14704807759288840, 7.771081512783700518 ) ) ;
#20313 = ORIENTED_EDGE ( 'NONE', *, *, #21544, .T. ) ;
#20314 = CARTESIAN_POINT ( 'NONE',  ( -79.58467717747977588, 11.50090110917795450, -5.024625831181132263 ) ) ;
#20315 = CARTESIAN_POINT ( 'NONE',  ( -9.078675913592196167, -26.64985754041175525, 6.700000000000000178 ) ) ;
#20316 = ORIENTED_EDGE ( 'NONE', *, *, #5773, .T. ) ;
#20317 = DIRECTION ( 'NONE',  ( 0.000000000000000000, 0.000000000000000000, 1.000000000000000000 ) ) ;
#20318 = VECTOR ( 'NONE', #32910, 1000.000000000000000 ) ;
#20319 = ORIENTED_EDGE ( 'NONE', *, *, #21407, .T. ) ;
#20320 = CARTESIAN_POINT ( 'NONE',  ( 80.47318323629822601, 63.22351390842185737, -3.619557188109181922 ) ) ;
#20321 = LINE ( 'NONE', #4692, #27952 ) ;
#20322 = CARTESIAN_POINT ( 'NONE',  ( 79.10907727509496112, 65.55534887285796231, 2.778975589575228167 ) ) ;
#20323 = CARTESIAN_POINT ( 'NONE',  ( 26.46424199157858226, 1.161643656104778488, 4.368481250744165933 ) ) ;
#20325 = VERTEX_POINT ( 'NONE', #39799 ) ;
#20324 = DIRECTION ( 'NONE',  ( -0.000000000000000000, 1.000000000000000000, -0.000000000000000000 ) ) ;
#20326 = CARTESIAN_POINT ( 'NONE',  ( -0.02576358332172043811, -32.49916105256644983, 7.782167645815905033 ) ) ;
#20328 = CARTESIAN_POINT ( 'NONE',  ( -16.87867591359218977, -26.64985754041175525, 6.800000000000000711 ) ) ;
#20327 = CARTESIAN_POINT ( 'NONE',  ( 91.69672933337632514, -4.640393979863029372, 6.000000000000001776 ) ) ;
#20329 = DIRECTION ( 'NONE',  ( -0.5000000000000039968, 0.8660254037844363761, -0.000000000000000000 ) ) ;
#20330 = CARTESIAN_POINT ( 'NONE',  ( 4.657599813362783614, -31.24770399340489746, 7.652160403243380316 ) ) ;
#20331 = EDGE_CURVE ( 'NONE', #3667, #11806, #18655, .T. ) ;
#20332 = CARTESIAN_POINT ( 'NONE',  ( 22.45719325378483333, 4.667233400556632716, -3.240875079928056568 ) ) ;
#20333 = ORIENTED_EDGE ( 'NONE', *, *, #39543, .F. ) ;
#20334 = CARTESIAN_POINT ( 'NONE',  ( -12.34874870218063947, -25.49307895267003587, 6.800000000000000711 ) ) ;
#20335 = ORIENTED_EDGE ( 'NONE', *, *, #12467, .F. ) ;
#20336 = VECTOR ( 'NONE', #12709, 1000.000000000000000 ) ;
#20337 = CARTESIAN_POINT ( 'NONE',  ( 22.73811350958456501, -4.924115162416450531, 6.814090253401713149 ) ) ;
#20338 = CARTESIAN_POINT ( 'NONE',  ( 21.88804895128980021, 3.976982562626299345, -2.124131737561591127 ) ) ;
#20339 = CARTESIAN_POINT ( 'NONE',  ( 16.50401484676293506, 9.937674364320209008, 2.500000000000111466 ) ) ;
#20340 = VERTEX_POINT ( 'NONE', #40000 ) ;
#20341 = CARTESIAN_POINT ( 'NONE',  ( -70.42837670882107659, -36.87473357531881391, 0.8660254037844411501 ) ) ;
#20342 = CARTESIAN_POINT ( 'NONE',  ( 79.42963897888203917, 66.02853703564775856, 2.226826180281127332 ) ) ;
#20343 = CARTESIAN_POINT ( 'NONE',  ( 88.55280947256005675, -1.781472883390815110, -2.828200999223334566 ) ) ;
#20344 = DIRECTION ( 'NONE',  ( -0.000000000000000000, -0.000000000000000000, -1.000000000000000000 ) ) ;
#20345 = VERTEX_POINT ( 'NONE', #40199 ) ;
#20346 = PLANE ( 'NONE',  #36541 ) ;
#20347 = DIRECTION ( 'NONE',  ( 1.000000000000000000, 0.000000000000000000, 0.000000000000000000 ) ) ;
#20348 = ADVANCED_FACE ( 'NONE', ( #24144 ), #8694, .F. ) ;
#20349 = CARTESIAN_POINT ( 'NONE',  ( 4.516786734692483485, -27.65257114232802493, 7.505001789837628223 ) ) ;
#20350 = AXIS2_PLACEMENT_3D ( 'NONE', #19399, #28457, #16101 ) ;
#20351 = CARTESIAN_POINT ( 'NONE',  ( 15.20539192819301633, -3.834574542907454475, -2.579567172824699828 ) ) ;
#20352 = CARTESIAN_POINT ( 'NONE',  ( 36.42048812037058525, -3.112390500302440355, -5.890696022654337227 ) ) ;
#20353 = CARTESIAN_POINT ( 'NONE',  ( -40.24874870218063450, -25.49307895267003587, 6.800000000000000711 ) ) ;
#20354 = CARTESIAN_POINT ( 'NONE',  ( 84.11387586591480670, 3.001218439285060047, 0.7410103870498383483 ) ) ;
#20355 = CARTESIAN_POINT ( 'NONE',  ( 28.97886027966445610, -3.943940219105989353, -4.212134838613624588 ) ) ;
#20356 = ORIENTED_EDGE ( 'NONE', *, *, #27216, .F. ) ;
#20357 = CARTESIAN_POINT ( 'NONE',  ( -34.24874870218063450, -25.49307895267003587, 6.700000000000000178 ) ) ;
#20358 = PLANE ( 'NONE',  #21120 ) ;
#20359 = CARTESIAN_POINT ( 'NONE',  ( -1.201486998515826743, -27.79817699957155597, 6.870716933885664623 ) ) ;
#20360 = EDGE_CURVE ( 'NONE', #32730, #4993, #37093, .T. ) ;
#20361 = ORIENTED_EDGE ( 'NONE', *, *, #1649, .F. ) ;
#20362 = ORIENTED_EDGE ( 'NONE', *, *, #34488, .F. ) ;
#20363 = CARTESIAN_POINT ( 'NONE',  ( 36.88795034744942569, -3.350989778144811471, 5.910704712194680965 ) ) ;
#20364 = CARTESIAN_POINT ( 'NONE',  ( -0.5265381365170317407, -32.27007802618333443, 7.660770905198784675 ) ) ;
#20365 = CARTESIAN_POINT ( 'NONE',  ( 33.45832265597695709, -3.170157842402876014, 5.428378461693221801 ) ) ;
#20366 = VECTOR ( 'NONE', #29628, 1000.000000000000000 ) ;
#20367 = ORIENTED_EDGE ( 'NONE', *, *, #14400, .T. ) ;
#20368 = CARTESIAN_POINT ( 'NONE',  ( 5.140791489254627145, -28.92678305073006584, 7.695279973900954751 ) ) ;
#20369 = VERTEX_POINT ( 'NONE', #30758 ) ;
#20370 = DIRECTION ( 'NONE',  ( -0.000000000000000000, 0.000000000000000000, 1.000000000000000000 ) ) ;
#20372 = FACE_OUTER_BOUND ( 'NONE', #27718, .T. ) ;
#20371 = FILL_AREA_STYLE_COLOUR ( '', #13365 ) ;
#20373 = ORIENTED_EDGE ( 'NONE', *, *, #865, .F. ) ;
#20374 = CARTESIAN_POINT ( 'NONE',  ( 23.41989428638003901, 3.663279710099765385, 3.339762963842272558 ) ) ;
#20375 = CARTESIAN_POINT ( 'NONE',  ( 80.30118292188586793, 66.27423127454432006, -1.564050819714060792 ) ) ;
#20376 = LINE ( 'NONE', #1272, #545 ) ;
#20377 = EDGE_CURVE ( 'NONE', #38144, #3709, #13929, .T. ) ;
#20378 = AXIS2_PLACEMENT_3D ( 'NONE', #34250, #6023, #34044 ) ;
#20379 = LINE ( 'NONE', #4158, #21983 ) ;
#20380 = VERTEX_POINT ( 'NONE', #2560 ) ;
#20382 = CARTESIAN_POINT ( 'NONE',  ( 18.07512871310107982, -2.861803080523624754, -3.027459002956025103 ) ) ;
#20381 = DIRECTION ( 'NONE',  ( 1.000000000000000000, 0.000000000000000000, -0.000000000000000000 ) ) ;
#20383 = CARTESIAN_POINT ( 'NONE',  ( 22.17093972887607478, 4.944255074668806316, -3.666709369531458318 ) ) ;
#20384 = CARTESIAN_POINT ( 'NONE',  ( 74.16083781478751291, 62.90537518464178390, 3.184487947857685519 ) ) ;
#20385 = CARTESIAN_POINT ( 'NONE',  ( 23.78275041547294677, 2.837768902955438932, -3.973267813322601150 ) ) ;
#20386 = CARTESIAN_POINT ( 'NONE',  ( -62.89172142731288062, 37.18122596373011390, 4.326867315595950281 ) ) ;
#20387 = FACE_OUTER_BOUND ( 'NONE', #19247, .T. ) ;
#20388 = LINE ( 'NONE', #1285, #15101 ) ;
#20389 = CARTESIAN_POINT ( 'NONE',  ( -62.81463675898083210, 36.67811266762162603, 4.600311178732273021 ) ) ;
#20390 = DIRECTION ( 'NONE',  ( 0.000000000000000000, 1.000000000000000000, 0.000000000000000000 ) ) ;
#20391 = CARTESIAN_POINT ( 'NONE',  ( 82.07485033897428650, 63.29559580402029439, 2.558871340112365278 ) ) ;
#20392 = CARTESIAN_POINT ( 'NONE',  ( 85.06715496341631422, 2.806258611057371066, -0.4571093354346482673 ) ) ;
#20393 = CARTESIAN_POINT ( 'NONE',  ( 29.23504802441905071, -0.3867851007456850065, 5.903809272860179647 ) ) ;
#20394 = EDGE_CURVE ( 'NONE', #29514, #22775, #21070, .T. ) ;
#20395 = ADVANCED_FACE ( 'NONE', ( #18372 ), #33447, .T. ) ;
#20396 = CARTESIAN_POINT ( 'NONE',  ( -63.08758708074094557, 43.61223004741322740, 1.000000000000000000 ) ) ;
#20397 = CARTESIAN_POINT ( 'NONE',  ( 4.662690227536057996, -31.23869556963216354, 7.695279973900954751 ) ) ;
#20398 = ADVANCED_FACE ( 'NONE', ( #33226 ), #18129, .F. ) ;
#20399 = VECTOR ( 'NONE', #27903, 1000.000000000000000 ) ;
#20400 = CARTESIAN_POINT ( 'NONE',  ( -75.26792576154856818, -3.339667509723542427, -10.38202132129838162 ) ) ;
#20401 = DIRECTION ( 'NONE',  ( 1.000000000000000000, 0.000000000000000000, 0.000000000000000000 ) ) ;
#20402 = FACE_OUTER_BOUND ( 'NONE', #935, .T. ) ;
#20403 = CARTESIAN_POINT ( 'NONE',  ( 35.91729403143805399, -1.971504941976118364, -5.812160415281375947 ) ) ;
#20404 = PRESENTATION_STYLE_ASSIGNMENT (( #24514 ) ) ;
#20405 = CARTESIAN_POINT ( 'NONE',  ( -70.92837670882107659, 28.72470171467712063, 0.000000000000000000 ) ) ;
#20406 = FACE_OUTER_BOUND ( 'NONE', #8259, .T. ) ;
#20407 = DIRECTION ( 'NONE',  ( -0.3757233601570931225, -0.9267318687906784813, 0.000000000000000000 ) ) ;
#20408 = AXIS2_PLACEMENT_3D ( 'NONE', #22466, #18745, #438 ) ;
#20409 = EDGE_CURVE ( 'NONE', #33969, #15938, #19358, .T. ) ;
#20410 = VERTEX_POINT ( 'NONE', #28463 ) ;
#20411 = CARTESIAN_POINT ( 'NONE',  ( 35.35512691508515104, -3.679868515684123320, 5.594709844209936556 ) ) ;
#20412 = FACE_OUTER_BOUND ( 'NONE', #27163, .T. ) ;
#20413 = CARTESIAN_POINT ( 'NONE',  ( 67.68985761519660116, 58.40038676363953840, -3.993918888840240822 ) ) ;
#20414 = CARTESIAN_POINT ( 'NONE',  ( 3.049102248865016129, -26.34022061302200868, 6.887547729233688187 ) ) ;
#20415 = EDGE_LOOP ( 'NONE', ( #35499, #19119, #11963, #39271 ) ) ;
#20416 = CARTESIAN_POINT ( 'NONE',  ( 1.686887486498432676, -33.27093018339341768, 7.635761828346577573 ) ) ;
#20417 = CARTESIAN_POINT ( 'NONE',  ( 3.908224997449445848, -32.15555842136866005, 7.730758795053810140 ) ) ;
#20418 = CARTESIAN_POINT ( 'NONE',  ( 84.63963357584157166, 2.348532213434630034, -3.962486329823844855 ) ) ;
#20419 = CARTESIAN_POINT ( 'NONE',  ( 5.050066951568335405, -28.55520611019255028, 6.951256099901589103 ) ) ;
#20420 = CARTESIAN_POINT ( 'NONE',  ( 0.3240269795377119233, -32.78794596868797839, 6.955226052476382925 ) ) ;
#20421 = CARTESIAN_POINT ( 'NONE',  ( 1.282397997787059651, -26.09497943095427175, 6.941203072598478130 ) ) ;
#20422 = ORIENTED_EDGE ( 'NONE', *, *, #28504, .T. ) ;
#20423 = CARTESIAN_POINT ( 'NONE',  ( 21.99062700448786600, 5.603250647612985524, 3.098096661096519266 ) ) ;
#20424 = VECTOR ( 'NONE', #26804, 1000.000000000000000 ) ;
#20425 = CARTESIAN_POINT ( 'NONE',  ( 17.93053216672853623, -3.172292528566667880, 2.962912945814812016 ) ) ;
#20426 = ADVANCED_FACE ( 'NONE', ( #4129 ), #18571, .T. ) ;
#20427 = CARTESIAN_POINT ( 'NONE',  ( 78.83705574937599181, 66.00318003113706311, 1.852607187800926036 ) ) ;
#20428 = CARTESIAN_POINT ( 'NONE',  ( -63.38847523777653237, 42.65083663216248766, 3.660712078102464684 ) ) ;
#20429 = ORIENTED_EDGE ( 'NONE', *, *, #21440, .T. ) ;
#20430 = CARTESIAN_POINT ( 'NONE',  ( 78.25991397077976330, 61.55280089391294496, -3.597602401604586220 ) ) ;
#20432 = CARTESIAN_POINT ( 'NONE',  ( 14.68921137941172717, -4.582243837930176866, -2.500000000000645262 ) ) ;
#20431 = CARTESIAN_POINT ( 'NONE',  ( 21.78052297937427539, 0.2074298702781548209, 8.415602729882047939 ) ) ;
#20433 = CARTESIAN_POINT ( 'NONE',  ( 80.36688112371665227, 65.40474626848705952, -3.015199126117773964 ) ) ;
#20434 = CARTESIAN_POINT ( 'NONE',  ( 78.53692321045886615, 63.86140601108343873, 3.670385203786641348 ) ) ;
#20435 = ADVANCED_FACE ( 'NONE', ( #26145 ), #7394, .T. ) ;
#20436 = CARTESIAN_POINT ( 'NONE',  ( 34.83208863909184316, -3.836908605833605712, -5.388068011310329197 ) ) ;
#20437 = EDGE_CURVE ( 'NONE', #4122, #33687, #34817, .T. ) ;
#20438 = AXIS2_PLACEMENT_3D ( 'NONE', #24563, #34064, #36711 ) ;
#20439 = CARTESIAN_POINT ( 'NONE',  ( 82.50386574309253263, 63.87755912629621236, 1.586031901069098193 ) ) ;
#20441 = EDGE_LOOP ( 'NONE', ( #25753, #33758, #24335, #3206, #36285, #37757 ) ) ;
#20440 = LINE ( 'NONE', #4808, #5829 ) ;
#20442 = CARTESIAN_POINT ( 'NONE',  ( 26.92542807167190944, 1.449366069832211279, 5.022290288739529984 ) ) ;
#20443 = CARTESIAN_POINT ( 'NONE',  ( -64.62035675220391795, 36.25855371424816553, -6.071883532252270399 ) ) ;
#20444 = VERTEX_POINT ( 'NONE', #4327 ) ;
#20445 = LINE ( 'NONE', #1736, #6464 ) ;
#20446 = CARTESIAN_POINT ( 'NONE',  ( 21.97771708808641478, 0.2279745448313108547, -7.713837705808137990 ) ) ;
#20447 = EDGE_CURVE ( 'NONE', #25213, #21312, #29234, .T. ) ;
#20448 = ORIENTED_EDGE ( 'NONE', *, *, #4514, .F. ) ;
#20449 = CARTESIAN_POINT ( 'NONE',  ( 0.000000000000000000, 0.5999999999999995337, -3.730072921939604047 ) ) ;
#20450 = CARTESIAN_POINT ( 'NONE',  ( 36.44423773317367932, -1.734327446880802093, -5.731973242487343079 ) ) ;
#20451 = DIRECTION ( 'NONE',  ( 1.000000000000000000, 1.165409145176970240E-16, 0.000000000000000000 ) ) ;
#20452 = CARTESIAN_POINT ( 'NONE',  ( -0.8786759135921904385, -26.64985754041175525, 6.700000000000000178 ) ) ;
#20453 = CARTESIAN_POINT ( 'NONE',  ( -78.45330471031414277, 33.71485196875532608, 12.50000000000000000 ) ) ;
#20454 = DIRECTION ( 'NONE',  ( -0.9396926207859104263, 0.3420201433256631063, -0.000000000000000000 ) ) ;
#20455 = CARTESIAN_POINT ( 'NONE',  ( -4.890026461918814071, -8.228598103685714525E-16, 2.500000000000000000 ) ) ;
#20456 = CARTESIAN_POINT ( 'NONE',  ( 5.094875594170104272, -29.76361320768288365, 7.006423389747792108 ) ) ;
#20457 = CARTESIAN_POINT ( 'NONE',  ( 1.794850636712705283, -26.07119012505348721, 6.863805608295729499 ) ) ;
#20458 = CARTESIAN_POINT ( 'NONE',  ( 2.133537915284704045, -33.04303106982295901, 6.903112506833890549 ) ) ;
#20459 = ORIENTED_EDGE ( 'NONE', *, *, #19124, .F. ) ;
#20460 = CARTESIAN_POINT ( 'NONE',  ( 66.58157743075884127, 57.80130068828511014, 3.999688274311175906 ) ) ;
#20461 = CARTESIAN_POINT ( 'NONE',  ( 72.46216784064273497, 59.07243765930573431, -3.784404822033881288 ) ) ;
#20462 = B_SPLINE_CURVE_WITH_KNOTS ( 'NONE', 3,
 ( #12350, #28194, #426, #15647, #23, #37458, #5776, #15849, #28619, #37867, #34619, #37260, #6393, #34411, #6184, #15435, #27787, #3130, #9671 ),
 .UNSPECIFIED., .F., .F.,
 ( 4, 3, 3, 3, 3, 3, 4 ),
 ( 0.000000000000000000, 2.546128104244751558E-05, 5.711050680484040440E-05, 8.113074941675670992E-05, 0.0001053129305727009795, 0.0001360598016347053458, 0.0001612931755701967431 ),
 .UNSPECIFIED. ) ;
#20463 = ORIENTED_EDGE ( 'NONE', *, *, #36430, .T. ) ;
#20464 = CARTESIAN_POINT ( 'NONE',  ( 85.50109956362166486, 1.391598633704343113, -5.555888502831813902 ) ) ;
#20465 = CIRCLE ( 'NONE', #23133, 3.499999999999999556 ) ;
#20466 = CARTESIAN_POINT ( 'NONE',  ( 0.1793115737041967861, -26.52915394410386796, 6.988553391373222290 ) ) ;
#20467 = CARTESIAN_POINT ( 'NONE',  ( 4.746899557684813864, -27.84691535960167030, 6.894806418505347700 ) ) ;
#20468 = PRODUCT_CONTEXT ( 'NONE', #35030, 'mechanical' ) ;
#20469 = CARTESIAN_POINT ( 'NONE',  ( 0.2020707124235944507, -34.04266111819475782, 7.754798119455333705 ) ) ;
#20470 = DIRECTION ( 'NONE',  ( 1.000000000000000000, 0.000000000000000000, 0.000000000000000000 ) ) ;
#20471 = CARTESIAN_POINT ( 'NONE',  ( -1.749066892114814253, -28.97726900121085336, 7.637894019485643504 ) ) ;
#20472 = EDGE_CURVE ( 'NONE', #18231, #29781, #40395, .T. ) ;
#20473 = ORIENTED_EDGE ( 'NONE', *, *, #3117, .T. ) ;
#20474 = CARTESIAN_POINT ( 'NONE',  ( 80.80164418317316688, 61.17044828488888442, -1.584170212883418305 ) ) ;
#20475 = DIRECTION ( 'NONE',  ( -0.000000000000000000, -0.000000000000000000, 1.000000000000000000 ) ) ;
#20476 = CARTESIAN_POINT ( 'NONE',  ( 78.96152850399714396, 65.10675657659960791, 3.115013800517340670 ) ) ;
#20478 = EDGE_LOOP ( 'NONE', ( #31439, #2472, #19873, #24686, #35001, #12526, #6696, #372 ) ) ;
#20477 = CARTESIAN_POINT ( 'NONE',  ( 33.45749450797183044, -3.829747548865578555, 5.093667367007288505 ) ) ;
#20479 = CYLINDRICAL_SURFACE ( 'NONE', #29127, 0.1000000000000028644 ) ;
#20480 = CARTESIAN_POINT ( 'NONE',  ( 15.36714913374379599, 11.54288649379375009, -2.576984622127588054 ) ) ;
#20481 = CARTESIAN_POINT ( 'NONE',  ( -18.97867591359219475, -24.55319635012989110, 6.700000000000000178 ) ) ;
#20482 = CARTESIAN_POINT ( 'NONE',  ( 21.85643539959776760, 7.606201961588627825, -9.696886732879795190 ) ) ;
#20483 = ORIENTED_EDGE ( 'NONE', *, *, #1888, .T. ) ;
#20484 = CARTESIAN_POINT ( 'NONE',  ( -78.64259192827009315, 10.18527460795026940, 8.122084567072173300 ) ) ;
#20485 = EDGE_CURVE ( 'NONE', #7709, #33117, #18064, .T. ) ;
#20486 = CARTESIAN_POINT ( 'NONE',  ( 14.75755952713405428, -4.578576653438560129, 2.509474734851031119 ) ) ;
#20487 = VECTOR ( 'NONE', #22033, 1000.000000000000000 ) ;
#20488 = ADVANCED_FACE ( 'NONE', ( #9516 ), #6450, .F. ) ;
#20489 = CARTESIAN_POINT ( 'NONE',  ( -77.68233785927705526, 11.14461418698115125, -7.385558889936151949 ) ) ;
#20490 = CARTESIAN_POINT ( 'NONE',  ( 1.501176615848605289, -32.96409121586394519, 6.997764925645181933 ) ) ;
#20491 = DIRECTION ( 'NONE',  ( 0.000000000000000000, 0.000000000000000000, 1.000000000000000000 ) ) ;
#20492 = CARTESIAN_POINT ( 'NONE',  ( 81.34759249528946157, 61.83023590116508217, 2.361823859647546264 ) ) ;
#20493 = DIRECTION ( 'NONE',  ( 1.000000000000000000, 5.786005779812646808E-17, 0.000000000000000000 ) ) ;
#20494 = CARTESIAN_POINT ( 'NONE',  ( -20.24874870218063805, -26.64985754041175525, 6.700000000000000178 ) ) ;
#20495 = DIRECTION ( 'NONE',  ( 0.000000000000000000, 0.000000000000000000, 1.000000000000000000 ) ) ;
#20496 = CARTESIAN_POINT ( 'NONE',  ( 0.6832822253045948147, -26.22097430988279498, 6.931070083220555844 ) ) ;
#20497 = CARTESIAN_POINT ( 'NONE',  ( -64.08758708074093136, 36.14363715547680300, 3.800414904976363140 ) ) ;
#20498 = LINE ( 'NONE', #23992, #4854 ) ;
#20499 = DIRECTION ( 'NONE',  ( -0.000000000000000000, 0.000000000000000000, -1.000000000000000000 ) ) ;
#20500 = CARTESIAN_POINT ( 'NONE',  ( 67.98336428835678191, 58.50351186300884621, 3.992939643064463695 ) ) ;
#20501 = CARTESIAN_POINT ( 'NONE',  ( 29.10269789033915444, 0.3625583223530568500, 4.748577875832423523 ) ) ;
#20502 = CARTESIAN_POINT ( 'NONE',  ( 2.271049717768559351, -33.00993214001371712, 7.783750581861600182 ) ) ;
#20503 = CARTESIAN_POINT ( 'NONE',  ( 88.00102923632725549, -0.4892082223494365611, 4.076460784956554839 ) ) ;
#20505 = CARTESIAN_POINT ( 'NONE',  ( 33.61415416546452661, -1.222806787721765431, -5.452699737548062586 ) ) ;
#20504 = CARTESIAN_POINT ( 'NONE',  ( 81.08836214216864846, 62.22329742272083308, -2.932725070486247532 ) ) ;
#20506 = CARTESIAN_POINT ( 'NONE',  ( -1.386427062873444971, -31.21787257485771860, 7.761113333116786528 ) ) ;
#20507 = B_SPLINE_CURVE_WITH_KNOTS ( 'NONE', 3,
 ( #3960, #6625, #19172, #29050, #18758, #453, #6823, #31738, #12580, #34644, #31536, #3552, #3360, #15877, #28434, #242, #19377, #16081, #28645, #12781, #25356, #12992, #38299, #29254, #4737, #7621, #35843, #16874, #29648, #26962, #23475 ),
 .UNSPECIFIED., .F., .F.,
 ( 4, 3, 3, 3, 3, 3, 3, 3, 3, 3, 4 ),
 ( 8.673617379884035472E-19, 2.999644130997489372E-05, 6.002588995694583369E-05, 8.960886084587896901E-05, 0.0001190604700446460436, 0.0001489538463052678444, 0.0001796139255493967978, 0.0002109707048517057775, 0.0002426195318110350042, 0.0002740640997890026061, 0.0002849778069099786191 ),
 .UNSPECIFIED. ) ;
#20508 = CARTESIAN_POINT ( 'NONE',  ( -1.606535956885630778, -28.77983680501876051, 6.920489980334479263 ) ) ;
#20509 = CARTESIAN_POINT ( 'NONE',  ( -59.00096901216079459, 28.68090462335501201, 7.030006629679628638 ) ) ;
#20510 = ORIENTED_EDGE ( 'NONE', *, *, #34982, .T. ) ;
#20511 = CARTESIAN_POINT ( 'NONE',  ( -17.27251170661583402, -8.656638842136340273, -6.000000000000000000 ) ) ;
#20512 = EDGE_LOOP ( 'NONE', ( #36621, #29423, #3754, #10066, #31749, #34549, #17463, #6913, #23661, #9913, #807, #22234, #21609, #39515, #37809, #39448, #30653, #21818, #3370, #18520, #30029, #8521, #32494, #15403, #10765, #7699, #9614, #1075, #32251, #36248, #32092, #15450, #37306, #26199, #32148, #40228, #36987, #21095, #30420, #4556, #6340, #13306, #31082, #39010, #16070, #9821, #23619, #25125, #27100, #4059, #27016, #40413, #29105, #29967, #30882, #26556, #11201, #9041, #13141 ) ) ;
#20513 = ORIENTED_EDGE ( 'NONE', *, *, #1780, .F. ) ;
#20514 = ORIENTED_EDGE ( 'NONE', *, *, #20917, .T. ) ;
#20515 = CARTESIAN_POINT ( 'NONE',  ( 80.91173626137313590, 62.16536564854128954, -2.996423812020329258 ) ) ;
#20516 = DIRECTION ( 'NONE',  ( 1.000000000000000000, 0.000000000000000000, 0.000000000000000000 ) ) ;
#20517 = PRODUCT_RELATED_PRODUCT_CATEGORY ( 'part', '', ( #22464 ) ) ;
#20518 = CARTESIAN_POINT ( 'NONE',  ( 79.12626349118839642, 65.57005066984849861, 2.769656700700049878 ) ) ;
#20519 = CARTESIAN_POINT ( 'NONE',  ( 26.31986897742153886, 1.795161610767696203, 4.274183613285711836 ) ) ;
#20522 = VERTEX_POINT ( 'NONE', #5321 ) ;
#20521 = CARTESIAN_POINT ( 'NONE',  ( 4.747863368183087296, -27.87906903544868342, 7.785593909369613819 ) ) ;
#20520 = VECTOR ( 'NONE', #22725, 1000.000000000000000 ) ;
#20523 = FACE_OUTER_BOUND ( 'NONE', #33294, .T. ) ;
#20524 = CARTESIAN_POINT ( 'NONE',  ( 3.351130934865960587, -32.54231216990946507, 6.887041543973314361 ) ) ;
#20525 =( BOUNDED_CURVE ( )  B_SPLINE_CURVE ( 3, ( #34894, #13036, #26009, #38540 ),
 .UNSPECIFIED., .F., .T. ) 
 B_SPLINE_CURVE_WITH_KNOTS ( ( 4, 4 ),
 ( 1.381924640371167801, 1.574767692156076482 ),
 .UNSPECIFIED. ) 
 CURVE ( )  GEOMETRIC_REPRESENTATION_ITEM ( )  RATIONAL_B_SPLINE_CURVE ( ( 1.000000000000000000, 0.9969033633783032089, 0.9969033633783032089, 1.000000000000000000 ) ) 
 REPRESENTATION_ITEM ( '' )  );
#20527 = CARTESIAN_POINT ( 'NONE',  ( 20.40287464734031531, 10.75613383782063970, 2.500000000000000000 ) ) ;
#20526 = CARTESIAN_POINT ( 'NONE',  ( -69.32837670882108227, -31.30579396504363388, 1.870248747537495149E-15 ) ) ;
#20528 = CARTESIAN_POINT ( 'NONE',  ( -1.218628611532051265, -27.82653379209746092, 7.785868773668303433 ) ) ;
#20529 = DIRECTION ( 'NONE',  ( 1.000000000000000000, 0.000000000000000000, 0.000000000000000000 ) ) ;
#20530 = CARTESIAN_POINT ( 'NONE',  ( 21.94264646427332366, 5.218753353571838893, -3.467988951643584006 ) ) ;
#20531 = ORIENTED_EDGE ( 'NONE', *, *, #19487, .T. ) ;
#20532 = CARTESIAN_POINT ( 'NONE',  ( -71.05911450274722085, 0.2170085631127137149, 6.000000000000031974 ) ) ;
#20533 = ADVANCED_FACE ( 'NONE', ( #30232 ), #11069, .F. ) ;
#20534 = CARTESIAN_POINT ( 'NONE',  ( 22.59998850301547790, -2.767621054697568361, -8.672491381162554802 ) ) ;
#20536 = ADVANCED_FACE ( 'NONE', ( #11470 ), #28618, .T. ) ;
#20535 = CARTESIAN_POINT ( 'NONE',  ( 21.90687190820672470, 4.042035482290116555, 2.582324705332042310E-12 ) ) ;
#20537 = DIRECTION ( 'NONE',  ( 0.000000000000000000, 0.000000000000000000, 1.000000000000000000 ) ) ;
#20538 = DIRECTION ( 'NONE',  ( -0.000000000000000000, -0.000000000000000000, 1.000000000000000000 ) ) ;
#20539 = CARTESIAN_POINT ( 'NONE',  ( 80.30538902757352560, 65.37113732873363858, 3.059106349699973304 ) ) ;
#20540 = CARTESIAN_POINT ( 'NONE',  ( 84.71993633203089757, 2.603525311087758531, 3.468835001793752593 ) ) ;
#20541 = CARTESIAN_POINT ( 'NONE',  ( -70.92837670882107659, -60.53509472482660669, 0.000000000000000000 ) ) ;
#20542 = ORIENTED_EDGE ( 'NONE', *, *, #27726, .F. ) ;
#20543 = DIRECTION ( 'NONE',  ( -0.000000000000000000, 1.000000000000000000, -0.000000000000000000 ) ) ;
#20544 = CARTESIAN_POINT ( 'NONE',  ( -81.28678620492023299, -5.643235788115313234, 3.601638239438431199 ) ) ;
#20545 = VERTEX_POINT ( 'NONE', #14560 ) ;
#20546 = FACE_OUTER_BOUND ( 'NONE', #3406, .T. ) ;
#20547 = CARTESIAN_POINT ( 'NONE',  ( 14.96457931905862004, -6.087096554337192877, -2.529921590516770458 ) ) ;
#20548 = CARTESIAN_POINT ( 'NONE',  ( 37.04325894773570838, -2.892658674496945359, -5.987894472034057891 ) ) ;
#20549 = DIRECTION ( 'NONE',  ( 0.1736481776669127897, 0.9848077530122111289, 0.000000000000000000 ) ) ;
#20550 = CARTESIAN_POINT ( 'NONE',  ( 22.37006418220767046, 0.3113197332365596481, -6.949876465829976979 ) ) ;
#20551 = CARTESIAN_POINT ( 'NONE',  ( -0.5039490865542369802, -26.98131590518362088, 7.740055089680398126 ) ) ;
#20552 = ORIENTED_EDGE ( 'NONE', *, *, #27458, .F. ) ;
#20553 = CARTESIAN_POINT ( 'NONE',  ( 36.99180085876906787, -2.719722283181335687, 5.979863192732237209 ) ) ;
#20554 = CIRCLE ( 'NONE', #2850, 0.9999999999999976685 ) ;
#20555 = DIRECTION ( 'NONE',  ( -0.000000000000000000, -1.000000000000000000, -0.000000000000000000 ) ) ;
#20556 = CARTESIAN_POINT ( 'NONE',  ( -1.174035473898453752, -27.75395182900487612, 6.865312560952603782 ) ) ;
#20557 = ORIENTED_EDGE ( 'NONE', *, *, #34299, .F. ) ;
#20558 = ORIENTED_EDGE ( 'NONE', *, *, #28540, .F. ) ;
#20559 = CARTESIAN_POINT ( 'NONE',  ( 23.38648198192572636, 3.560659895774239025, 3.090151982821246701 ) ) ;
#20560 = CARTESIAN_POINT ( 'NONE',  ( -0.5300021044395021308, -32.26722227524986408, 7.651421919295148477 ) ) ;
#20561 = CARTESIAN_POINT ( 'NONE',  ( -38.24874870218063450, -25.49307895267003587, 6.800000000000000711 ) ) ;
#20562 = DIRECTION ( 'NONE',  ( 1.000000000000000000, 0.000000000000000000, 0.000000000000000000 ) ) ;
#20563 = ORIENTED_EDGE ( 'NONE', *, *, #18630, .F. ) ;
#20564 = CARTESIAN_POINT ( 'NONE',  ( 4.713340623123058570, -27.78888299018493058, 7.695279973900954751 ) ) ;
#20565 = ORIENTED_EDGE ( 'NONE', *, *, #35580, .F. ) ;
#20566 = ORIENTED_EDGE ( 'NONE', *, *, #25915, .F. ) ;
#20567 = CARTESIAN_POINT ( 'NONE',  ( -75.45330471031414277, 33.71485196875532608, 8.800414904976364028 ) ) ;
#20568 = CARTESIAN_POINT ( 'NONE',  ( -57.76433750236255804, 32.39122475941741186, -4.160719226838292428 ) ) ;
#20569 = CARTESIAN_POINT ( 'NONE',  ( -71.92837670882106238, -42.87473357531881391, 1.732050807568877637 ) ) ;
#20570 = ORIENTED_EDGE ( 'NONE', *, *, #8811, .F. ) ;
#20571 = CARTESIAN_POINT ( 'NONE',  ( 21.76873572098353549, 5.759726986437556207, 3.412036244753165359 ) ) ;
#20572 = CARTESIAN_POINT ( 'NONE',  ( 80.42596214810023980, 66.05751922670441445, -2.080779877698640590 ) ) ;
#20573 = LINE ( 'NONE', #23864, #31420 ) ;
#20574 = EDGE_CURVE ( 'NONE', #40124, #39495, #3401, .T. ) ;
#20575 = LINE ( 'NONE', #13606, #18661 ) ;
#20576 = ORIENTED_EDGE ( 'NONE', *, *, #25965, .F. ) ;
#20578 = LINE ( 'NONE', #23487, #13083 ) ;
#20577 = LINE ( 'NONE', #8425, #4866 ) ;
#20579 = CARTESIAN_POINT ( 'NONE',  ( -1.794389567730132695, -29.37881818594272687, 6.971170733404102648 ) ) ;
#20580 = CARTESIAN_POINT ( 'NONE',  ( 73.70000790436553473, 62.44749314232890924, 3.395557233589456825 ) ) ;
#20581 = AXIS2_PLACEMENT_3D ( 'NONE', #28438, #2950, #28027 ) ;
#20582 = CARTESIAN_POINT ( 'NONE',  ( 23.35463534039838862, 2.791180645285405326, -4.165794450420091444 ) ) ;
#20583 = ORIENTED_EDGE ( 'NONE', *, *, #16662, .T. ) ;
#20584 = DIRECTION ( 'NONE',  ( -1.000000000000000000, 0.000000000000000000, 0.000000000000000000 ) ) ;
#20585 = CARTESIAN_POINT ( 'NONE',  ( -56.34850605459113382, 30.68671187671608536, -2.749655849400832963 ) ) ;
#20587 = EDGE_CURVE ( 'NONE', #24867, #26610, #39686, .T. ) ;
#20586 = DIRECTION ( 'NONE',  ( -1.000000000000000000, 0.000000000000000000, 0.000000000000000000 ) ) ;
#20588 = CARTESIAN_POINT ( 'NONE',  ( 4.313599969017027469, -31.74504722509605159, 7.635761828346577573 ) ) ;
#20589 = DIRECTION ( 'NONE',  ( -1.000000000000000000, 0.000000000000000000, 0.000000000000000000 ) ) ;
#20590 = CARTESIAN_POINT ( 'NONE',  ( 78.90307038293786945, 66.16006992971016132, 1.301239782962659852 ) ) ;
#20591 = CARTESIAN_POINT ( 'NONE',  ( 85.52484820210342775, 2.292155841932438154, 3.149942891487422791 ) ) ;
#20592 = CARTESIAN_POINT ( 'NONE',  ( 28.29523375420085074, 1.184784106264966219, 4.843441543353563361 ) ) ;
#20593 = LINE ( 'NONE', #33178, #2397 ) ;
#20594 = CYLINDRICAL_SURFACE ( 'NONE', #7731, 0.09010775117052938210 ) ;
#20595 = CARTESIAN_POINT ( 'NONE',  ( -73.82579051696868078, -1.443931487737144304, -10.81507813807952090 ) ) ;
#20596 = CARTESIAN_POINT ( 'NONE',  ( 0.5857718112008674094, -26.35782306785393203, 6.892063359921932530 ) ) ;
#20597 = AXIS2_PLACEMENT_3D ( 'NONE', #28934, #735, #16556 ) ;
#20598 = VECTOR ( 'NONE', #38356, 1000.000000000000000 ) ;
#20599 = FACE_OUTER_BOUND ( 'NONE', #30689, .T. ) ;
#20600 = CARTESIAN_POINT ( 'NONE',  ( 36.83726977465116903, -2.495954238268284886, -5.955744879707230766 ) ) ;
#20601 = CARTESIAN_POINT ( 'NONE',  ( 4.656309160454404683, -31.44410799460488448, 6.875780273367530171 ) ) ;
#20602 = DIRECTION ( 'NONE',  ( -0.6427876096865328126, -0.7660444431189835646, -0.000000000000000000 ) ) ;
#20603 = CARTESIAN_POINT ( 'NONE',  ( 1.574364539997139767, -33.06766052747819629, 7.750000000000000888 ) ) ;
#20604 = DIRECTION ( 'NONE',  ( -0.000000000000000000, -0.000000000000000000, 1.000000000000000000 ) ) ;
#20605 = ORIENTED_EDGE ( 'NONE', *, *, #20967, .T. ) ;
#20606 = CARTESIAN_POINT ( 'NONE',  ( 36.98479848736133846, -3.196135743401947504, 5.957709319320976249 ) ) ;
#20607 = DIRECTION ( 'NONE',  ( 0.8660254037844380415, 0.5000000000000009992, -0.000000000000000000 ) ) ;
#20608 = ADVANCED_FACE ( 'NONE', ( #24038 ), #30028, .F. ) ;
#20609 = CARTESIAN_POINT ( 'NONE',  ( 67.63028434841179148, 58.56128740577801750, -3.979762160777184477 ) ) ;
#20610 = B_SPLINE_CURVE_WITH_KNOTS ( 'NONE', 3,
 ( #20248, #1147, #3838, #6901, #35719, #13682, #38372, #26251, #10171, #10580, #22763, #3635, #16160, #35329, #23151, #28724, #7098, #19660, #7494 ),
 .UNSPECIFIED., .F., .F.,
 ( 4, 3, 3, 3, 3, 3, 4 ),
 ( 1.893477691975264912E-18, 2.546128104244556401E-05, 5.711050680483675877E-05, 8.113074941675210206E-05, 0.0001053129305726940135, 0.0001360598016346985153, 0.0001612931755713739156 ),
 .UNSPECIFIED. ) ;
#20611 = CARTESIAN_POINT ( 'NONE',  ( -0.6444488087166562185, -32.16833941288422238, 7.750000000000000888 ) ) ;
#20612 = VERTEX_POINT ( 'NONE', #23830 ) ;
#20613 = PLANE ( 'NONE',  #26580 ) ;
#20614 = CARTESIAN_POINT ( 'NONE',  ( 2.259918937511053105, -26.20908457450270745, 7.257242401810562349 ) ) ;
#20615 = CARTESIAN_POINT ( 'NONE',  ( 85.24784528485831459, 1.525343023627036221, -5.365780758369952608 ) ) ;
#20616 = CARTESIAN_POINT ( 'NONE',  ( 0.9874470777302929436, -32.89435814851245254, 6.863904403958575706 ) ) ;
#20617 = ADVANCED_FACE ( 'NONE', ( #39074 ), #7985, .T. ) ;
#20618 = CARTESIAN_POINT ( 'NONE',  ( -33.07867591359219972, -26.64985754041175525, 6.700000000000000178 ) ) ;
#20619 = DIRECTION ( 'NONE',  ( 0.000000000000000000, 1.000000000000000000, 0.000000000000000000 ) ) ;
#20620 = ORIENTED_EDGE ( 'NONE', *, *, #23652, .T. ) ;
#20621 = EDGE_CURVE ( 'NONE', #22624, #32358, #37755, .T. ) ;
#20622 = CARTESIAN_POINT ( 'NONE',  ( 22.38585600833290812, 4.919343847142990001, 3.067110144847137843 ) ) ;
#20623 = CARTESIAN_POINT ( 'NONE',  ( 81.62248346935345467, 65.70993096190730398, -1.153249692834613427 ) ) ;
#20624 = EDGE_CURVE ( 'NONE', #31321, #35289, #22379, .T. ) ;
#20626 = AXIS2_PLACEMENT_3D ( 'NONE', #36168, #2203, #8344 ) ;
#20625 = CARTESIAN_POINT ( 'NONE',  ( 80.57402935197536920, 63.63785766202913408, 3.625945587094185463 ) ) ;
#20627 = VERTEX_POINT ( 'NONE', #23253 ) ;
#20628 = CARTESIAN_POINT ( 'NONE',  ( 77.25588627614904169, 64.91391695767343606, -2.512892981323163077 ) ) ;
#20630 = CARTESIAN_POINT ( 'NONE',  ( 2.265556469525966232, -26.21722959230298144, 7.652160403243383868 ) ) ;
#20629 = CARTESIAN_POINT ( 'NONE',  ( 21.96835430550240531, 0.2152734445375746875, 7.743662324112909445 ) ) ;
#20631 = CARTESIAN_POINT ( 'NONE',  ( 81.06025503660893605, 64.27053461118835287, -3.341858160548295320 ) ) ;
#20632 = CARTESIAN_POINT ( 'NONE',  ( -18.44874870218064089, -25.49307895267003587, 6.700000000000000178 ) ) ;
#20633 = CARTESIAN_POINT ( 'NONE',  ( 77.50572060368776306, 65.09508644891811002, 2.418543376929332744 ) ) ;
#20634 = VECTOR ( 'NONE', #9136, 1000.000000000000000 ) ;
#20635 = CARTESIAN_POINT ( 'NONE',  ( -0.9271279775035500270, -27.41211907304282036, 7.695279973900954751 ) ) ;
#20636 = ADVANCED_FACE ( 'NONE', ( #35819 ), #33339, .T. ) ;
#20637 = VECTOR ( 'NONE', #36244, 1000.000000000000000 ) ;
#20638 = B_SPLINE_CURVE_WITH_KNOTS ( 'NONE', 3,
 ( #5112, #8593, #18264, #37008, #2043, #2243, #8790, #39683, #40095, #5318 ),
 .UNSPECIFIED., .F., .F.,
 ( 4, 3, 3, 4 ),
 ( 0.0002170292169044841320, 0.0002420761345916009981, 0.0002723302478207072501, 0.0002816811360866829810 ),
 .UNSPECIFIED. ) ;
#20639 = CARTESIAN_POINT ( 'NONE',  ( 82.29396208789067657, 62.51418980721558682, 1.483157530538788516 ) ) ;
#20642 = ORIENTED_EDGE ( 'NONE', *, *, #21498, .F. ) ;
#20641 = LINE ( 'NONE', #5212, #28845 ) ;
#20640 = CARTESIAN_POINT ( 'NONE',  ( 3.485436849364648815, -26.67619661698708100, 7.774064877406524410 ) ) ;
#20643 = CARTESIAN_POINT ( 'NONE',  ( 30.10774373291980766, -4.462292185204852046, -2.031966353365944666 ) ) ;
#20644 = CARTESIAN_POINT ( 'NONE',  ( -1.774127509761148858, -29.99150749123047532, 6.980586498568968956 ) ) ;
#20645 = CYLINDRICAL_SURFACE ( 'NONE', #34514, 7.538952224936807056 ) ;
#20646 = VERTEX_POINT ( 'NONE', #17247 ) ;
#20647 = CARTESIAN_POINT ( 'NONE',  ( -80.58170359628198298, -5.694316091744713759, 2.641081141217533457 ) ) ;
#20648 = CARTESIAN_POINT ( 'NONE',  ( 27.43026218121176996, 0.9933767425001067686, -4.487545422184641808 ) ) ;
#20649 = FACE_OUTER_BOUND ( 'NONE', #21056, .T. ) ;
#20650 = VERTEX_POINT ( 'NONE', #4714 ) ;
#20651 = CARTESIAN_POINT ( 'NONE',  ( -4.890026461918812295, -8.951974136083761024, -6.000000000000000000 ) ) ;
#20652 = CARTESIAN_POINT ( 'NONE',  ( 5.173052788776492328, -29.13333318653474890, 7.009310105710487626 ) ) ;
#20653 = CARTESIAN_POINT ( 'NONE',  ( -70.92837670882107659, -23.80776546975053520, 0.000000000000000000 ) ) ;
#20654 = CARTESIAN_POINT ( 'NONE',  ( 33.45079413477735386, -3.771336813828650936, -5.158274019676979627 ) ) ;
#20655 = CARTESIAN_POINT ( 'NONE',  ( 8.290806648384990041, 0.000000000000000000, -6.000000000000000000 ) ) ;
#20656 = CARTESIAN_POINT ( 'NONE',  ( 0.3896649785617538608, -32.81498557016907114, 7.754798119455333705 ) ) ;
#20657 = CARTESIAN_POINT ( 'NONE',  ( -1.096489673827657274, -31.67408406764383955, 6.921725064902951807 ) ) ;
#20658 = CARTESIAN_POINT ( 'NONE',  ( 5.001045691774267610, -30.73426600737448311, 7.678495282201405203 ) ) ;
#20659 = CARTESIAN_POINT ( 'NONE',  ( 2.793730807323614229, -32.78935575605969888, 6.874555630061442990 ) ) ;
#20660 = CARTESIAN_POINT ( 'NONE',  ( 2.875937710231030398, -32.76024173560432473, 7.635761828346577573 ) ) ;
#20661 = EDGE_CURVE ( 'NONE', #422, #28877, #3904, .T. ) ;
#20662 = CARTESIAN_POINT ( 'NONE',  ( -69.08758708074093136, 36.88538962427716683, -8.800414904976364028 ) ) ;
#20663 = ORIENTED_EDGE ( 'NONE', *, *, #29479, .T. ) ;
#20664 = CARTESIAN_POINT ( 'NONE',  ( 66.42891085676512830, 57.77139747978236528, 4.000000000000007994 ) ) ;
#20665 = CARTESIAN_POINT ( 'NONE',  ( 73.01418189060618147, 60.96508932706621664, -3.894134109168989610 ) ) ;
#20666 = VECTOR ( 'NONE', #38888, 1000.000000000000000 ) ;
#20667 = EDGE_LOOP ( 'NONE', ( #14495, #28234, #37624, #6223, #21808 ) ) ;
#20668 = DIRECTION ( 'NONE',  ( -0.000000000000000000, -0.000000000000000000, 1.000000000000000000 ) ) ;
#20669 = CARTESIAN_POINT ( 'NONE',  ( 0.1760639294348596007, -26.53077541110940629, 6.911401339314955372 ) ) ;
#20670 = CARTESIAN_POINT ( 'NONE',  ( 3.016566341302053811, -26.43500618872311492, 6.876076431790005827 ) ) ;
#20671 = EDGE_CURVE ( 'NONE', #3377, #18355, #16089, .T. ) ;
#20672 = CARTESIAN_POINT ( 'NONE',  ( -0.8789792430839086235, -27.20414525822329566, 6.880828092187095457 ) ) ;
#20673 = APPLICATION_PROTOCOL_DEFINITION ( 'draft international standard', 'automotive_design', 1998, #12393 ) ;
#20674 = PLANE ( 'NONE',  #4140 ) ;
#20675 = EDGE_CURVE ( 'NONE', #31321, #6597, #26742, .T. ) ;
#20676 = DIRECTION ( 'NONE',  ( 1.000000000000000000, 0.000000000000000000, 0.000000000000000000 ) ) ;
#20677 = CARTESIAN_POINT ( 'NONE',  ( -1.752215393550915268, -28.99588619853886229, 7.674970859709603133 ) ) ;
#20678 = CARTESIAN_POINT ( 'NONE',  ( 28.96720929824785884, -3.478576898793518613, 4.535785375070108927 ) ) ;
#20679 = ORIENTED_EDGE ( 'NONE', *, *, #2921, .T. ) ;
#20680 = CARTESIAN_POINT ( 'NONE',  ( 78.76746739705249922, 65.24896075961403596, -2.948506306558722478 ) ) ;
#20681 = CARTESIAN_POINT ( 'NONE',  ( 18.62546884766482336, 11.49410693564760244, -2.500000000000005773 ) ) ;
#20682 = CARTESIAN_POINT ( 'NONE',  ( 78.54017873204453792, 65.73972836631979533, 2.148686496494747633 ) ) ;
#20683 = CARTESIAN_POINT ( 'NONE',  ( 0.5324193565422453700, -26.37682618861159511, 7.763628509615287498 ) ) ;
#20684 = VECTOR ( 'NONE', #10726, 1000.000000000000114 ) ;
#20685 = CIRCLE ( 'NONE', #31864, 2.681419499219045655 ) ;
#20686 = DIRECTION ( 'NONE',  ( 0.000000000000000000, 0.000000000000000000, -1.000000000000000000 ) ) ;
#20687 = CIRCLE ( 'NONE', #15439, 0.1000000000000028644 ) ;
#20688 = EDGE_CURVE ( 'NONE', #32700, #21196, #8596, .T. ) ;
#20689 = CARTESIAN_POINT ( 'NONE',  ( 14.78132966858819408, 12.96967853271529592, -2.500000000000170530 ) ) ;
#20690 = CARTESIAN_POINT ( 'NONE',  ( 17.06909365960932234, 14.52075518970088019, 2.500000000000000000 ) ) ;
#20691 = CARTESIAN_POINT ( 'NONE',  ( 21.85643539959775339, -6.841675198209371977, -12.88699694080538549 ) ) ;
#20692 = ORIENTED_EDGE ( 'NONE', *, *, #9150, .T. ) ;
#20693 = CARTESIAN_POINT ( 'NONE',  ( -81.74866560783399905, 10.46844104627007610, 1.587951278892896001 ) ) ;
#20694 = VERTEX_POINT ( 'NONE', #2246 ) ;
#20695 = VECTOR ( 'NONE', #32162, 1000.000000000000114 ) ;
#20696 = CARTESIAN_POINT ( 'NONE',  ( 14.77552075046116542, -5.164772903469535770, 2.499999999999999556 ) ) ;
#20697 = CARTESIAN_POINT ( 'NONE',  ( -76.45633091588946684, 10.63030786891022217, -8.341557872600688484 ) ) ;
#20698 = CARTESIAN_POINT ( 'NONE',  ( 1.496541690888591569, -32.96381487152982004, 6.920489980334477487 ) ) ;
#20699 = CARTESIAN_POINT ( 'NONE',  ( 2.495801789269033399, -26.26427930321180071, 6.939395833800443114 ) ) ;
#20700 = CARTESIAN_POINT ( 'NONE',  ( 80.21507364257671213, 64.59331366548808262, 3.526329879082135577 ) ) ;
#20701 = CARTESIAN_POINT ( 'NONE',  ( -1.521215565022806082, -30.65682612155753262, 7.782034975670475418 ) ) ;
#20702 = CARTESIAN_POINT ( 'NONE',  ( -88.78960668556791802, 4.298224710795182091, 15.50000000000000000 ) ) ;
#20703 = DIRECTION ( 'NONE',  ( 0.000000000000000000, 1.000000000000000000, 0.000000000000000000 ) ) ;
#20704 = CARTESIAN_POINT ( 'NONE',  ( 31.23832812783138735, -0.3864266517737607876, 5.081894624805558536 ) ) ;
#20705 = CARTESIAN_POINT ( 'NONE',  ( -64.13386656030947108, 35.23920786735105537, 4.488055666952388556 ) ) ;
#20706 = CARTESIAN_POINT ( 'NONE',  ( 87.89830269644372152, -0.3738208970565018441, 3.381280162731604033 ) ) ;
#20707 = CARTESIAN_POINT ( 'NONE',  ( -1.751698146652124866, -30.14706689514045479, 6.894806418505347700 ) ) ;
#20708 = VERTEX_POINT ( 'NONE', #34168 ) ;
#20709 = CARTESIAN_POINT ( 'NONE',  ( 68.03141654933527604, 58.37504561612195886, 3.996230182412892074 ) ) ;
#20710 = CARTESIAN_POINT ( 'NONE',  ( 36.63374877720352174, -3.081660063073488942, 5.923980505881594638 ) ) ;
#20711 = ADVANCED_FACE ( 'NONE', ( #21174 ), #21375, .F. ) ;
#20712 = VERTEX_POINT ( 'NONE', #9409 ) ;
#20713 = DIRECTION ( 'NONE',  ( 0.000000000000000000, 1.000000000000000000, 0.000000000000000000 ) ) ;
#20714 = AXIS2_PLACEMENT_3D ( 'NONE', #30675, #33565, #8009 ) ;
#20716 = ADVANCED_FACE ( 'NONE', ( #18473 ), #15601, .F. ) ;
#20715 = CARTESIAN_POINT ( 'NONE',  ( 85.02283808163620904, 2.856037436078923797, 1.058370034767218248 ) ) ;
#20718 = CARTESIAN_POINT ( 'NONE',  ( -34.97867591359219830, -26.64985754041175525, 6.700000000000000178 ) ) ;
#20717 = CARTESIAN_POINT ( 'NONE',  ( 81.12869333199854793, 61.28902183752150989, -1.194943971655652692 ) ) ;
#20719 = FACE_OUTER_BOUND ( 'NONE', #24479, .T. ) ;
#20720 = CARTESIAN_POINT ( 'NONE',  ( 2.333682990176194849, -26.13904351153081507, 7.781480525794718162 ) ) ;
#20721 = AXIS2_PLACEMENT_3D ( 'NONE', #35587, #16814, #16607 ) ;
#20722 = CARTESIAN_POINT ( 'NONE',  ( -0.1483345642761195737, -26.70808950415996463, 7.139196562012273262 ) ) ;
#20723 = ADVANCED_FACE ( 'NONE', ( #31058 ), #21997, .T. ) ;
#20724 = VERTEX_POINT ( 'NONE', #3082 ) ;
#20725 = EDGE_CURVE ( 'NONE', #513, #35057, #33954, .T. ) ;
#20726 = VERTEX_POINT ( 'NONE', #30436 ) ;
#20727 = CARTESIAN_POINT ( 'NONE',  ( 80.18433095895142060, 63.45046554133029559, -3.702313260098204051 ) ) ;
#20728 = CARTESIAN_POINT ( 'NONE',  ( -1.553388381126008744, -28.28034428687672985, 6.863654226668488789 ) ) ;
#20729 = CARTESIAN_POINT ( 'NONE',  ( 80.65169068708814848, 62.63775009584345099, 3.403428918328332387 ) ) ;
#20730 = CARTESIAN_POINT ( 'NONE',  ( 22.20022480168698920, 0.7782003466350271292, 6.794645230738167285 ) ) ;
#20732 = EDGE_LOOP ( 'NONE', ( #31001, #29325, #24634, #31122, #6359 ) ) ;
#20731 = CARTESIAN_POINT ( 'NONE',  ( -0.8016911122223995267, -27.26782569596947070, 6.871394612369936539 ) ) ;
#20733 = CARTESIAN_POINT ( 'NONE',  ( 74.86608108239484238, 61.39286988729297434, -3.912919437578932236 ) ) ;
#20734 = DIRECTION ( 'NONE',  ( 1.000000000000000000, 0.000000000000000000, 0.000000000000000000 ) ) ;
#20736 = CARTESIAN_POINT ( 'NONE',  ( -16.44874870218064089, -25.49307895267003587, 6.700000000000000178 ) ) ;
#20735 = CARTESIAN_POINT ( 'NONE',  ( 87.04213330793392345, 0.5878691963682337596, -6.000000000000000000 ) ) ;
#20737 = CARTESIAN_POINT ( 'NONE',  ( -36.97867591359219119, -26.64985754041175525, 6.700000000000000178 ) ) ;
#20738 = DIRECTION ( 'NONE',  ( -1.000000000000000000, 0.000000000000000000, 0.000000000000000000 ) ) ;
#20739 = CARTESIAN_POINT ( 'NONE',  ( 24.19406260597309100, 3.095814450226969772, -3.579834043910485430 ) ) ;
#20740 = VERTEX_POINT ( 'NONE', #9006 ) ;
#20741 = CARTESIAN_POINT ( 'NONE',  ( 2.474049714983521664, -26.15650803111381606, 7.013842709614101167 ) ) ;
#20742 = AXIS2_PLACEMENT_3D ( 'NONE', #11472, #8598, #39688 ) ;
#20743 = CARTESIAN_POINT ( 'NONE',  ( 22.40307219844260800, 2.196575021783337522, 8.487454310335619923 ) ) ;
#20744 = AXIS2_PLACEMENT_3D ( 'NONE', #38302, #22282, #19176 ) ;
#20745 = CARTESIAN_POINT ( 'NONE',  ( -70.92837670882107659, -42.37473357531882812, 0.000000000000000000 ) ) ;
#20746 = VERTEX_POINT ( 'NONE', #27339 ) ;
#20747 = DIRECTION ( 'NONE',  ( 0.000000000000000000, -1.147978770867004622E-16, 1.000000000000000000 ) ) ;
#20748 = CARTESIAN_POINT ( 'NONE',  ( 78.68330935989222041, 66.05356751642948154, 1.089225060639253950 ) ) ;
#20749 = CARTESIAN_POINT ( 'NONE',  ( 88.36457133188896762, -1.562442635866588381, -3.606418352999261945 ) ) ;
#20750 = CARTESIAN_POINT ( 'NONE',  ( 5.123750824668761972, -30.29724448404768111, 7.754798119455333705 ) ) ;
#20751 = ORIENTED_EDGE ( 'NONE', *, *, #2148, .T. ) ;
#20752 = CARTESIAN_POINT ( 'NONE',  ( -0.1576164094376339420, -32.53604074034053895, 7.750000000000000888 ) ) ;
#20753 = TOROIDAL_SURFACE ( 'NONE', #16812, 82.54614097552274643, 3.000000000000000000 ) ;
#20754 = CARTESIAN_POINT ( 'NONE',  ( 24.57140847954032736, 3.461729712179683727, -1.987756385015271743 ) ) ;
#20755 = CARTESIAN_POINT ( 'NONE',  ( 14.65343585136595550, -5.052488753627910611, -2.492953801041927431 ) ) ;
#20756 = CARTESIAN_POINT ( 'NONE',  ( 33.46279134528099064, -3.082547165344575735, -5.429075908734783518 ) ) ;
#20757 = DIRECTION ( 'NONE',  ( -0.6662082868431848937, 0.000000000000000000, 0.7457657263118685487 ) ) ;
#20758 = CARTESIAN_POINT ( 'NONE',  ( 26.54498440466941389, 1.102037382031719526, -4.373732055846625499 ) ) ;
#20759 = CARTESIAN_POINT ( 'NONE',  ( 29.67375726883929588, -3.794827553840666834, -4.437594031920679249 ) ) ;
#20760 = ORIENTED_EDGE ( 'NONE', *, *, #23859, .T. ) ;
#20761 = CARTESIAN_POINT ( 'NONE',  ( 36.44579707039719096, -2.356748688111148127, 5.894646096405367963 ) ) ;
#20762 = CARTESIAN_POINT ( 'NONE',  ( -1.142394782723454405, -27.70483658010354588, 6.903372536218457256 ) ) ;
#20763 = ORIENTED_EDGE ( 'NONE', *, *, #1468, .T. ) ;
#20764 = VERTEX_POINT ( 'NONE', #40297 ) ;
#20765 = CARTESIAN_POINT ( 'NONE',  ( 36.68630651783246321, -1.913378901653658204, 5.802382176530635149 ) ) ;
#20766 = CARTESIAN_POINT ( 'NONE',  ( -1.638124420012986970, -30.62083709180146940, 6.880828092187095457 ) ) ;
#20767 = CARTESIAN_POINT ( 'NONE',  ( -42.24874870218063450, -26.64985754041175525, 6.700000000000000178 ) ) ;
#20768 = CARTESIAN_POINT ( 'NONE',  ( -12.97867591359219297, -26.64985754041175525, 6.700000000000000178 ) ) ;
#20769 = EDGE_CURVE ( 'NONE', #19421, #11999, #18061, .T. ) ;
#20770 = ORIENTED_EDGE ( 'NONE', *, *, #38625, .T. ) ;
#20771 = CARTESIAN_POINT ( 'NONE',  ( 0.7553917981025534134, -32.94700704774471944, 7.501983001166816933 ) ) ;
#20772 = EDGE_CURVE ( 'NONE', #7067, #4105, #10278, .T. ) ;
#20773 = VERTEX_POINT ( 'NONE', #11673 ) ;
#20774 = VECTOR ( 'NONE', #24482, 1000.000000000000000 ) ;
#20775 = EDGE_CURVE ( 'NONE', #40623, #6564, #17379, .T. ) ;
#20776 = EDGE_LOOP ( 'NONE', ( #27384, #31890 ) ) ;
#20777 = FACE_OUTER_BOUND ( 'NONE', #16981, .T. ) ;
#20778 = CARTESIAN_POINT ( 'NONE',  ( 81.06670574969137988, 62.21556664890213284, -2.940771700540079969 ) ) ;
#20779 =( BOUNDED_CURVE ( )  B_SPLINE_CURVE ( 3, ( #30393, #11220, #27290, #17395 ),
 .UNSPECIFIED., .F., .T. ) 
 B_SPLINE_CURVE_WITH_KNOTS ( ( 4, 4 ),
 ( 4.748221474220559735, 4.941946782021394036 ),
 .UNSPECIFIED. ) 
 CURVE ( )  GEOMETRIC_REPRESENTATION_ITEM ( )  RATIONAL_B_SPLINE_CURVE ( ( 1.000000000000000000, 0.9968749865767494445, 0.9968749865767494445, 1.000000000000000000 ) ) 
 REPRESENTATION_ITEM ( '' )  );
#20780 = ORIENTED_EDGE ( 'NONE', *, *, #30305, .F. ) ;
#20781 = CARTESIAN_POINT ( 'NONE',  ( 14.72813520417063948, -4.877442212653578579, 2.502183594662707122 ) ) ;
#20782 = ORIENTED_EDGE ( 'NONE', *, *, #11043, .F. ) ;
#20783 = CARTESIAN_POINT ( 'NONE',  ( 4.822514058981756335, -27.98804819767207874, 6.971170733404099096 ) ) ;
#20784 = VERTEX_POINT ( 'NONE', #14985 ) ;
#20785 = CARTESIAN_POINT ( 'NONE',  ( 23.89669137058255899, 3.224793199604093275, 3.569543781043807762 ) ) ;
#20786 = CARTESIAN_POINT ( 'NONE',  ( 81.78811924969963343, 65.04137315806627839, -2.360008641315554545 ) ) ;
#20787 = CARTESIAN_POINT ( 'NONE',  ( 0.07492370758569941169, -33.99638339305766266, 7.635761828346577573 ) ) ;
#20788 = EDGE_LOOP ( 'NONE', ( #35452, #11100, #3148, #38395 ) ) ;
#20790 = CARTESIAN_POINT ( 'NONE',  ( 18.11716068014149883, -2.855953840192153592, -3.034019107959646799 ) ) ;
#20789 = CARTESIAN_POINT ( 'NONE',  ( 0.002871653215719630579, -26.62401247480054067, 7.769368695748484654 ) ) ;
#20791 = CARTESIAN_POINT ( 'NONE',  ( -1.795161916675976466, -29.39339987696827805, 6.903112506833889661 ) ) ;
#20792 = CARTESIAN_POINT ( 'NONE',  ( 75.58356882164667923, 59.79721036961943526, 3.404024988867351720 ) ) ;
#20793 = CARTESIAN_POINT ( 'NONE',  ( 22.69246715650346147, 2.749719814763217141, -4.568240441793316897 ) ) ;
#20794 = VERTEX_POINT ( 'NONE', #40098 ) ;
#20795 = CARTESIAN_POINT ( 'NONE',  ( 16.14043045949875577, 15.25506048169804352, 0.6630684997064625330 ) ) ;
#20796 = FACE_OUTER_BOUND ( 'NONE', #30247, .T. ) ;
#20797 = CARTESIAN_POINT ( 'NONE',  ( -24.44874870218064089, -26.64985754041175525, 6.700000000000000178 ) ) ;
#20798 = CARTESIAN_POINT ( 'NONE',  ( -66.90228649915854930, 37.07846761000362790, 9.592188357273904842 ) ) ;
#20800 = CARTESIAN_POINT ( 'NONE',  ( 81.31254497084479738, 65.18305021144017530, 2.731810022747817701 ) ) ;
#20799 =( REPRESENTATION_RELATIONSHIP ('NONE','NONE', #24012, #23772 ) REPRESENTATION_RELATIONSHIP_WITH_TRANSFORMATION ( #11395 )SHAPE_REPRESENTATION_RELATIONSHIP( ) );
#20801 = CARTESIAN_POINT ( 'NONE',  ( 85.13880989351328310, 2.725772392624387308, 0.2960746283792183853 ) ) ;
#20802 = CARTESIAN_POINT ( 'NONE',  ( 31.27801355750085222, -2.827678977088778911, 5.603419278764796729 ) ) ;
#20803 = CARTESIAN_POINT ( 'NONE',  ( -77.50871672188519312, -4.892925716637096301, -9.117663693479695297 ) ) ;
#20804 = CARTESIAN_POINT ( 'NONE',  ( 15.14474440143671607, -4.106796728886147108, 2.560655039386400489 ) ) ;
#20805 = CARTESIAN_POINT ( 'NONE',  ( 2.921324086407800280, -26.64985754041175525, 6.700000000000000178 ) ) ;
#20806 = CARTESIAN_POINT ( 'NONE',  ( 30.58590753052908440, 0.06668957243665377121, -4.980068611744779439 ) ) ;
#20807 = DIRECTION ( 'NONE',  ( 0.000000000000000000, -1.000000000000000000, 0.000000000000000000 ) ) ;
#20808 = CARTESIAN_POINT ( 'NONE',  ( 4.631036947150836802, -31.48338494934807485, 6.941203072598471024 ) ) ;
#20809 = AXIS2_PLACEMENT_3D ( 'NONE', #853, #17065, #25961 ) ;
#20810 = CARTESIAN_POINT ( 'NONE',  ( -8.348748702180635917, -25.49307895267003587, 6.800000000000000711 ) ) ;
#20811 = VECTOR ( 'NONE', #39531, 1000.000000000000000 ) ;
#20812 = CIRCLE ( 'NONE', #12952, 6.172764123155108251 ) ;
#20813 = DIRECTION ( 'NONE',  ( -0.000000000000000000, -0.000000000000000000, -1.000000000000000000 ) ) ;
#20814 = CARTESIAN_POINT ( 'NONE',  ( -16.24874870218063450, -25.49307895267003587, 6.800000000000000711 ) ) ;
#20815 = ORIENTED_EDGE ( 'NONE', *, *, #5919, .F. ) ;
#20816 = CARTESIAN_POINT ( 'NONE',  ( 21.70417851619663097, 4.205083555597296296, 2.944929548107457329 ) ) ;
#20817 = CARTESIAN_POINT ( 'NONE',  ( -34.24874870218063450, -25.49307895267003587, 6.800000000000000711 ) ) ;
#20818 = CARTESIAN_POINT ( 'NONE',  ( 66.73227421799262515, 57.84320248636868200, -3.999246569070631363 ) ) ;
#20819 = CARTESIAN_POINT ( 'NONE',  ( -70.92837670881976919, 0.2170085631237942680, 10.00000000000113154 ) ) ;
#20820 = CARTESIAN_POINT ( 'NONE',  ( 5.651251297819362307, -26.64985754041175525, 6.700000000000000178 ) ) ;
#20821 = ORIENTED_EDGE ( 'NONE', *, *, #4310, .F. ) ;
#20822 = CARTESIAN_POINT ( 'NONE',  ( -0.4809337148280844465, -32.17797450963541195, 7.763628509615282169 ) ) ;
#20824 = EDGE_CURVE ( 'NONE', #18734, #11497, #11879, .T. ) ;
#20823 = CYLINDRICAL_SURFACE ( 'NONE', #23928, 0.1000000000000028644 ) ;
#20825 = CARTESIAN_POINT ( 'NONE',  ( 85.60524239217707532, 0.9672249164365797069, -5.812461325880615703 ) ) ;
#20826 = CARTESIAN_POINT ( 'NONE',  ( -76.56376567441922987, 10.68475264541021552, 8.270291949397417852 ) ) ;
#20827 = DIRECTION ( 'NONE',  ( 0.000000000000000000, -0.000000000000000000, 1.000000000000000000 ) ) ;
#20828 = EDGE_CURVE ( 'NONE', #12896, #15980, #37414, .T. ) ;
#20829 = DIRECTION ( 'NONE',  ( -0.000000000000000000, -0.000000000000000000, 1.000000000000000000 ) ) ;
#20830 = VERTEX_POINT ( 'NONE', #9210 ) ;
#20831 = CARTESIAN_POINT ( 'NONE',  ( 24.04940727412492762, 3.336460009922597614, 3.254743572800636642 ) ) ;
#20832 = CARTESIAN_POINT ( 'NONE',  ( 82.51683713915174678, 64.24667231656792410, -1.319711737400975915 ) ) ;
#20833 = CARTESIAN_POINT ( 'NONE',  ( 79.55838722571232324, 65.27247487857080444, 3.155412080370055605 ) ) ;
#20834 = CIRCLE ( 'NONE', #3139, 0.1000000000000028644 ) ;
#20835 = CARTESIAN_POINT ( 'NONE',  ( -0.1589752317941719728, -32.41646502212034875, 7.013842709614101167 ) ) ;
#20836 = VERTEX_POINT ( 'NONE', #6138 ) ;
#20837 = CARTESIAN_POINT ( 'NONE',  ( 78.95923394621955538, 61.57577394195563159, -3.401348408886269770 ) ) ;
#20839 = CARTESIAN_POINT ( 'NONE',  ( 14.73588997190238459, -5.111296489852609426, -2.499999999999999556 ) ) ;
#20838 = CARTESIAN_POINT ( 'NONE',  ( 21.96606689427578374, 0.2111432007872987293, 7.751452917624079397 ) ) ;
#20840 = VECTOR ( 'NONE', #20269, 1000.000000000000000 ) ;
#20841 = CARTESIAN_POINT ( 'NONE',  ( 81.35401977073111368, 62.93507997573861701, -3.162824939344917041 ) ) ;
#20842 = CARTESIAN_POINT ( 'NONE',  ( 78.65659160455585663, 63.63274296288032161, 3.750642650174855319 ) ) ;
#20843 = AXIS2_PLACEMENT_3D ( 'NONE', #38782, #38576, #10381 ) ;
#20844 = ORIENTED_EDGE ( 'NONE', *, *, #911, .T. ) ;
#20845 = AXIS2_PLACEMENT_3D ( 'NONE', #15592, #2656, #37203 ) ;
#20846 = CARTESIAN_POINT ( 'NONE',  ( -0.8516922296151283600, -27.32338581145017997, 7.782034975670478971 ) ) ;
#20847 = ORIENTED_EDGE ( 'NONE', *, *, #25489, .F. ) ;
#20848 = CARTESIAN_POINT ( 'NONE',  ( 79.30570723442079384, 66.28915683679507254, 1.250621450094003384 ) ) ;
#20851 = EDGE_LOOP ( 'NONE', ( #27862, #36687, #31900, #8407 ) ) ;
#20850 = CARTESIAN_POINT ( 'NONE',  ( -64.08758708074093136, 38.13199975834322686, 3.043809435734686097 ) ) ;
#20849 = PLANE ( 'NONE',  #5332 ) ;
#20852 = CARTESIAN_POINT ( 'NONE',  ( 29.52151182519568096, -2.704869923190903691, 5.373754524306347591 ) ) ;
#20853 = EDGE_CURVE ( 'NONE', #212, #29188, #18680, .T. ) ;
#20854 = CARTESIAN_POINT ( 'NONE',  ( -38.24874870218063450, -26.64985754041175525, 6.800000000000000711 ) ) ;
#20855 = DIRECTION ( 'NONE',  ( 0.000000000000000000, 0.000000000000000000, 1.000000000000000000 ) ) ;
#20856 = ORIENTED_EDGE ( 'NONE', *, *, #27570, .T. ) ;
#20857 = CARTESIAN_POINT ( 'NONE',  ( -81.48430623221383939, -5.632154720818524751, 2.883670397763604676 ) ) ;
#20858 = CARTESIAN_POINT ( 'NONE',  ( 23.59114525325624001, 0.4240393697126918493, -5.524181805179797955 ) ) ;
#20859 = DIRECTION ( 'NONE',  ( 1.000000000000000000, 0.000000000000000000, 0.000000000000000000 ) ) ;
#20860 = EDGE_LOOP ( 'NONE', ( #6081, #31996, #1059, #21247, #9962 ) ) ;
#20861 = CARTESIAN_POINT ( 'NONE',  ( -33.07867591359219972, -26.64985754041175525, 6.700000000000000178 ) ) ;
#20862 = CARTESIAN_POINT ( 'NONE',  ( 5.157792374610187913, -29.02545772698320903, 6.870737987065013819 ) ) ;
#20863 = DIRECTION ( 'NONE',  ( 1.000000000000000000, 0.000000000000000000, 0.000000000000000000 ) ) ;
#20864 = CARTESIAN_POINT ( 'NONE',  ( 34.14194983325678834, -3.845064528984907692, -5.237895465648701787 ) ) ;
#20865 = CARTESIAN_POINT ( 'NONE',  ( 3.378163903244623345, -26.61272046326372376, 7.652160403243390974 ) ) ;
#20866 = CARTESIAN_POINT ( 'NONE',  ( -75.45330471031414277, 33.71485196875532608, -8.800414904976364028 ) ) ;
#20867 = LINE ( 'NONE', #36926, #30533 ) ;
#20868 = CARTESIAN_POINT ( 'NONE',  ( -71.68115880895459213, -48.41814739710035553, 5.953156766150077495 ) ) ;
#20869 = CARTESIAN_POINT ( 'NONE',  ( 2.679370002084180857, -32.82594665571590298, 7.006423389747790331 ) ) ;
#20870 = CARTESIAN_POINT ( 'NONE',  ( 5.099605094774092073, -29.64363437814743207, 6.874555630061440326 ) ) ;
#20871 = EDGE_CURVE ( 'NONE', #33155, #22837, #6949, .T. ) ;
#20872 = VECTOR ( 'NONE', #27132, 1000.000000000000000 ) ;
#20873 = CARTESIAN_POINT ( 'NONE',  ( 20.40287464734031531, 10.75613383782063970, 2.500000000000000000 ) ) ;
#20874 = CARTESIAN_POINT ( 'NONE',  ( 24.52499130180415676, 2.224616344218060870, -4.186325811553068377 ) ) ;
#20875 = EDGE_LOOP ( 'NONE', ( #3756, #34186, #19868, #40451 ) ) ;
#20876 = ORIENTED_EDGE ( 'NONE', *, *, #24600, .F. ) ;
#20877 = CARTESIAN_POINT ( 'NONE',  ( 66.27376694608996388, 57.73522568913447373, 4.000000000000000000 ) ) ;
#20878 = AXIS2_PLACEMENT_3D ( 'NONE', #6039, #18574, #2977 ) ;
#20879 = CARTESIAN_POINT ( 'NONE',  ( 71.13429564674895289, 59.00621471515203353, -3.925556587156297628 ) ) ;
#20880 = AXIS2_PLACEMENT_3D ( 'NONE', #28353, #8995, #37604 ) ;
#20881 = ORIENTED_EDGE ( 'NONE', *, *, #40286, .F. ) ;
#20882 = CARTESIAN_POINT ( 'NONE',  ( 85.50394501772831291, 1.137698216002840157, 5.721642786829533200 ) ) ;
#20884 = EDGE_CURVE ( 'NONE', #5201, #16788, #5596, .T. ) ;
#20883 = DIRECTION ( 'NONE',  ( 0.000000000000000000, 0.7541618601367583441, 0.6566885781822799917 ) ) ;
#20885 = CARTESIAN_POINT ( 'NONE',  ( 3.057737949672496125, -26.45262135935053749, 6.939395833800443114 ) ) ;
#20886 = CARTESIAN_POINT ( 'NONE',  ( -1.417849890998097440, -28.21472003549629903, 6.979335674598003969 ) ) ;
#20887 = LINE ( 'NONE', #14693, #37273 ) ;
#20888 = CARTESIAN_POINT ( 'NONE',  ( -70.92837670882107659, 13.87661300689599386, -6.000000000000002665 ) ) ;
#20889 = ORIENTED_EDGE ( 'NONE', *, *, #18262, .F. ) ;
#20890 = DIRECTION ( 'NONE',  ( 0.000000000000000000, 0.000000000000000000, 1.000000000000000000 ) ) ;
#20891 = DIRECTION ( 'NONE',  ( 1.000000000000000000, -0.000000000000000000, 0.000000000000000000 ) ) ;
#20892 = ORIENTED_EDGE ( 'NONE', *, *, #19443, .F. ) ;
#20893 = CARTESIAN_POINT ( 'NONE',  ( 80.27814043029276547, 62.51814696698978935, -3.475409704257724997 ) ) ;
#20894 = CARTESIAN_POINT ( 'NONE',  ( 21.82633866793786837, 5.573670839087305318, -3.484773916741194189 ) ) ;
#20895 = CARTESIAN_POINT ( 'NONE',  ( 80.45692750329149590, 65.79057296784165487, -2.573500632437589086 ) ) ;
#20896 = CARTESIAN_POINT ( 'NONE',  ( 79.84106601136197412, 63.63461245521319398, 3.725738571856552550 ) ) ;
#20897 = EDGE_CURVE ( 'NONE', #25596, #19681, #35322, .T. ) ;
#20898 = CIRCLE ( 'NONE', #35390, 7.538952224936807056 ) ;
#20899 = DIRECTION ( 'NONE',  ( 0.3420201433256578882, 0.9396926207859123137, 0.000000000000000000 ) ) ;
#20900 =( BOUNDED_CURVE ( )  B_SPLINE_CURVE ( 3, ( #36861, #34216, #8646, #3682 ),
 .UNSPECIFIED., .F., .F. ) 
 B_SPLINE_CURVE_WITH_KNOTS ( ( 4, 4 ),
 ( 2.498091544796508412, 2.888912398447714747 ),
 .UNSPECIFIED. ) 
 CURVE ( )  GEOMETRIC_REPRESENTATION_ITEM ( )  RATIONAL_B_SPLINE_CURVE ( ( 1.000000000000000000, 0.9873120399594201846, 0.9873120399594201846, 1.000000000000000000 ) ) 
 REPRESENTATION_ITEM ( '' )  );
#20901 = FACE_OUTER_BOUND ( 'NONE', #32313, .T. ) ;
#20902 = CARTESIAN_POINT ( 'NONE',  ( 18.84457505903907659, 12.88015104982928172, 2.500000000000000000 ) ) ;
#20903 = CARTESIAN_POINT ( 'NONE',  ( 21.85643539959778892, 9.726370091839324772, -5.619754257929120200 ) ) ;
#20904 = CIRCLE ( 'NONE', #24171, 3.499999999999999556 ) ;
#20905 = EDGE_LOOP ( 'NONE', ( #37463, #18185, #9534, #6349 ) ) ;
#20906 = CARTESIAN_POINT ( 'NONE',  ( -81.10340860069513269, 10.50981427116896683, 4.150601545968553907 ) ) ;
#20907 = CARTESIAN_POINT ( 'NONE',  ( 14.62026587516738552, -4.585255206722739452, 2.500000000000073275 ) ) ;
#20908 = CARTESIAN_POINT ( 'NONE',  ( -75.34513397755924302, 8.292114957421363286, -9.011728519595546771 ) ) ;
#20909 = CARTESIAN_POINT ( 'NONE',  ( -24.87867591359218977, -26.64985754041175525, 6.800000000000000711 ) ) ;
#20910 = CARTESIAN_POINT ( 'NONE',  ( 2.475127768148066565, -26.25936912986495386, 6.895222827070022653 ) ) ;
#20911 = CARTESIAN_POINT ( 'NONE',  ( -1.740571384909186170, -30.12451254141716106, 7.785344483711591934 ) ) ;
#20912 = CARTESIAN_POINT ( 'NONE',  ( 14.85267465595546277, 12.69378753320559561, 2.508660318056822991 ) ) ;
#20913 = LINE ( 'NONE', #33500, #29950 ) ;
#20914 = CARTESIAN_POINT ( 'NONE',  ( 0.6674044370517944191, -26.22583931010534641, 7.009310105710485850 ) ) ;
#20915 = EDGE_CURVE ( 'NONE', #25549, #25150, #19386, .T. ) ;
#20916 = EDGE_CURVE ( 'NONE', #14526, #27830, #18584, .T. ) ;
#20917 = EDGE_CURVE ( 'NONE', #8080, #28300, #38634, .T. ) ;
#20918 = CARTESIAN_POINT ( 'NONE',  ( 4.490574598675256546, -27.45690618315335030, 7.006908160621416748 ) ) ;
#20919 = LINE ( 'NONE', #36973, #7474 ) ;
#20920 = DIRECTION ( 'NONE',  ( -0.000000000000000000, -1.000000000000000000, -0.000000000000000000 ) ) ;
#20921 = ORIENTED_EDGE ( 'NONE', *, *, #8070, .T. ) ;
#20922 = CIRCLE ( 'NONE', #26207, 0.9999999999999994449 ) ;
#20923 = CARTESIAN_POINT ( 'NONE',  ( 67.66003928550829016, 58.48093499090138891, 3.988165415173012374 ) ) ;
#20924 = CARTESIAN_POINT ( 'NONE',  ( 30.51710498034237773, -0.1346816457499544206, 4.969330309792167277 ) ) ;
#20925 = ORIENTED_EDGE ( 'NONE', *, *, #2821, .F. ) ;
#20926 = DIRECTION ( 'NONE',  ( -0.9396926207858983249, -0.3420201433256965240, 0.000000000000000000 ) ) ;
#20928 = CARTESIAN_POINT ( 'NONE',  ( 4.832094736013836211, -30.89372247464815757, 6.882085323592682435 ) ) ;
#20927 = CARTESIAN_POINT ( 'NONE',  ( -0.1040043641139408170, -32.45162424111279620, 7.754798119455333705 ) ) ;
#20929 = DIRECTION ( 'NONE',  ( 0.7660444431189840087, -0.6427876096865322575, 0.000000000000000000 ) ) ;
#20930 = LINE ( 'NONE', #40680, #32708 ) ;
#20931 = CARTESIAN_POINT ( 'NONE',  ( 86.24939746029500043, 1.399093175074125783, 5.441570408720817653 ) ) ;
#20932 = CARTESIAN_POINT ( 'NONE',  ( -0.6913368354159359352, -32.12524937216382170, 6.931070083220554956 ) ) ;
#20933 = VECTOR ( 'NONE', #1788, 1000.000000000000114 ) ;
#20934 = ORIENTED_EDGE ( 'NONE', *, *, #31116, .F. ) ;
#20935 = CARTESIAN_POINT ( 'NONE',  ( -16.97867591359219475, -26.64985754041175525, 6.700000000000000178 ) ) ;
#20936 = ORIENTED_EDGE ( 'NONE', *, *, #20661, .T. ) ;
#20937 = CARTESIAN_POINT ( 'NONE',  ( 80.72421460287552009, 62.36539998118918504, -3.243225924683091232 ) ) ;
#20938 = CARTESIAN_POINT ( 'NONE',  ( -1.518426245678387021, -28.19544030114832012, 6.935328752148349984 ) ) ;
#20939 = CARTESIAN_POINT ( 'NONE',  ( 78.57229106431512378, 65.97474043420317003, 1.364493914842173306 ) ) ;
#20940 = CARTESIAN_POINT ( 'NONE',  ( 26.38284721815838907, 1.220606850701035917, 4.361609309555559477 ) ) ;
#20942 = ORIENTED_EDGE ( 'NONE', *, *, #2031, .F. ) ;
#20941 = CARTESIAN_POINT ( 'NONE',  ( -70.92837670882107659, 15.04836564048558500, 0.000000000000000000 ) ) ;
#20943 = DIRECTION ( 'NONE',  ( -0.000000000000000000, -0.000000000000000000, 1.000000000000000000 ) ) ;
#20944 = EDGE_CURVE ( 'NONE', #18695, #34099, #25887, .T. ) ;
#20945 = CARTESIAN_POINT ( 'NONE',  ( 74.27115401224453706, 62.67359094190467772, -3.404024988867591084 ) ) ;
#20946 = CYLINDRICAL_SURFACE ( 'NONE', #29773, 0.1000000000000028644 ) ;
#20947 = CIRCLE ( 'NONE', #16995, 6.329987104167475565 ) ;
#20949 = DIRECTION ( 'NONE',  ( 0.000000000000000000, 0.000000000000000000, 1.000000000000000000 ) ) ;
#20948 = CARTESIAN_POINT ( 'NONE',  ( 63.05383694556373797, -7.271989087314214117, -6.000000000000000000 ) ) ;
#20950 = CARTESIAN_POINT ( 'NONE',  ( -36.44874870218064444, -26.64985754041175525, 6.700000000000000178 ) ) ;
#20951 = FACE_OUTER_BOUND ( 'NONE', #24709, .T. ) ;
#20952 =( BOUNDED_CURVE ( )  B_SPLINE_CURVE ( 3, ( #29756, #15896, #37701, #12603 ),
 .UNSPECIFIED., .F., .T. ) 
 B_SPLINE_CURVE_WITH_KNOTS ( ( 4, 4 ),
 ( 4.708531083176469068, 4.895802057644189631 ),
 .UNSPECIFIED. ) 
 CURVE ( )  GEOMETRIC_REPRESENTATION_ITEM ( )  RATIONAL_B_SPLINE_CURVE ( ( 1.000000000000000000, 0.9970795998553221295, 0.9970795998553221295, 1.000000000000000000 ) ) 
 REPRESENTATION_ITEM ( '' )  );
#20953 = CARTESIAN_POINT ( 'NONE',  ( 24.70548837460795610, 3.001373608382478242, -3.440348275608817730 ) ) ;
#20954 = EDGE_LOOP ( 'NONE', ( #19218, #33591, #10785, #24689, #7197, #38168, #155, #34779, #17279, #16396, #35473, #38386, #18301, #35021, #39179, #39000, #35564, #22432, #30055, #20463, #29229, #38810, #22020, #35402, #35553, #24467, #17180, #22692, #33340, #4877, #7295, #1055, #2964, #18201, #32400, #34084, #894, #36996, #1419, #40135, #33192, #36783, #23669, #38759, #2935, #3083, #22459, #31645, #32451, #28902, #31520, #28394, #40712, #27084, #21587, #25813, #12243, #35400, #17321, #4300, #9342, #17533, #31315, #3001, #11762, #35151, #25022, #18333, #25952, #12003, #10813, #27607, #6328, #33510, #34959, #11011, #22676, #37842, #12985, #32198, #2650, #28085, #22240, #16381, #569, #4200, #13012, #6467, #31673, #21321, #27524, #25199, #9184, #24048, #33820, #23854, #37335, #38368, #21007, #23656, #35052, #32203, #3459, #15546, #30311, #21234, #21761, #13091, #27991, #21447, #31449 ) ) ;
#20955 = LINE ( 'NONE', #5928, #33417 ) ;
#20956 = ADVANCED_FACE ( 'NONE', ( #31875 ), #10227, .T. ) ;
#20957 = CARTESIAN_POINT ( 'NONE',  ( 22.58802438714224081, -2.565763546402358486, 8.787087332313648247 ) ) ;
#20958 = EDGE_CURVE ( 'NONE', #35983, #38495, #39080, .T. ) ;
#20959 = CARTESIAN_POINT ( 'NONE',  ( 21.04004186717268965, 8.045167201113928357, 2.500000000002262190 ) ) ;
#20960 = ORIENTED_EDGE ( 'NONE', *, *, #18740, .F. ) ;
#20961 = CARTESIAN_POINT ( 'NONE',  ( 1.060084769145667405, -32.99765172409238545, 7.783750581861601070 ) ) ;
#20962 = CARTESIAN_POINT ( 'NONE',  ( 81.16306007146954471, 61.30159356321340169, 1.077711394955742863 ) ) ;
#20963 = CARTESIAN_POINT ( 'NONE',  ( 84.55403409623259847, 2.802886334004389024, 2.719422554281196280 ) ) ;
#20964 = B_SPLINE_CURVE_WITH_KNOTS ( 'NONE', 3,
 ( #6982, #32124, #16630, #25520, #7376, #38457, #38263, #32512 ),
 .UNSPECIFIED., .F., .F.,
 ( 4, 2, 2, 4 ),
 ( 3.990099683909797064E-17, 0.0004307664291302241554, 0.0006461496436953162838, 0.0008615328582604084122 ),
 .UNSPECIFIED. ) ;
#20965 = CARTESIAN_POINT ( 'NONE',  ( 2.780913079066563487, -32.89888420713570838, 7.753200566781599079 ) ) ;
#20966 = ORIENTED_EDGE ( 'NONE', *, *, #29248, .T. ) ;
#20967 = EDGE_CURVE ( 'NONE', #8713, #28414, #1636, .T. ) ;
#20968 = FACE_OUTER_BOUND ( 'NONE', #27349, .T. ) ;
#20969 = CARTESIAN_POINT ( 'NONE',  ( 14.74324248891501554, -5.593081337125382468, -2.503816905324318665 ) ) ;
#20970 = EDGE_CURVE ( 'NONE', #38778, #34298, #38437, .T. ) ;
#20971 = CARTESIAN_POINT ( 'NONE',  ( 35.86767921836906226, -2.089981252190320937, -5.804416823763172140 ) ) ;
#20972 = CARTESIAN_POINT ( 'NONE',  ( 38.29999999999999716, 3.061616997868383141E-16, -2.500000000000000000 ) ) ;
#20973 = CARTESIAN_POINT ( 'NONE',  ( 22.69170078865038320, 0.3323897375237238605, -6.389351011922190793 ) ) ;
#20974 = CARTESIAN_POINT ( 'NONE',  ( 3.960473582032317363, -32.24238647371081612, 7.635761828346576685 ) ) ;
#20975 = EDGE_LOOP ( 'NONE', ( #34860, #3476, #10456, #39304 ) ) ;
#20976 = CARTESIAN_POINT ( 'NONE',  ( 2.787276362915718231, -32.89601384403606943, 7.761113333116785640 ) ) ;
#20977 = FACE_OUTER_BOUND ( 'NONE', #28859, .T. ) ;
#20978 = VECTOR ( 'NONE', #8167, 1000.000000000000000 ) ;
#20979 = ORIENTED_EDGE ( 'NONE', *, *, #31861, .T. ) ;
#20980 = ORIENTED_EDGE ( 'NONE', *, *, #31579, .T. ) ;
#20982 = CARTESIAN_POINT ( 'NONE',  ( 30.88492579994572296, 0.7017300443915822639, 4.487230210454935531 ) ) ;
#20981 = CARTESIAN_POINT ( 'NONE',  ( 81.13213036240664167, 62.83067685251092627, -3.261148789966863859 ) ) ;
#20983 = CARTESIAN_POINT ( 'NONE',  ( 18.12789740749335010, -2.854475511803001631, 3.035694833931636971 ) ) ;
#20984 = CARTESIAN_POINT ( 'NONE',  ( 17.77531322304072603, -3.190942049385152135, -2.940571408766233130 ) ) ;
#20985 = CARTESIAN_POINT ( 'NONE',  ( 14.77315594796472631, 13.19392823276517568, -2.499999999999998668 ) ) ;
#20986 = ORIENTED_EDGE ( 'NONE', *, *, #32052, .T. ) ;
#20987 = PLANE ( 'NONE',  #12164 ) ;
#20988 = ORIENTED_EDGE ( 'NONE', *, *, #13776, .T. ) ;
#20989 = ORIENTED_EDGE ( 'NONE', *, *, #20263, .F. ) ;
#20990 = CARTESIAN_POINT ( 'NONE',  ( 4.662690227536057996, -31.23869556963216354, 7.695279973900954751 ) ) ;
#20991 = DIRECTION ( 'NONE',  ( -0.000000000000000000, -0.000000000000000000, 1.000000000000000000 ) ) ;
#20992 = CARTESIAN_POINT ( 'NONE',  ( 80.89892670780336914, 62.72941125082673608, -3.340002271463665906 ) ) ;
#20993 = ORIENTED_EDGE ( 'NONE', *, *, #20958, .F. ) ;
#20995 = CARTESIAN_POINT ( 'NONE',  ( 21.88711032999522743, 3.208699644441221022, 3.395463446396979279 ) ) ;
#20994 = SURFACE_STYLE_USAGE ( .BOTH. , #29853 ) ;
#20996 = ORIENTED_EDGE ( 'NONE', *, *, #5109, .F. ) ;
#20997 = CARTESIAN_POINT ( 'NONE',  ( 23.42598874491005034, 3.327995987485997897, 3.701944623341963503 ) ) ;
#20998 = CARTESIAN_POINT ( 'NONE',  ( 81.77194423968612114, 61.86568514665825802, -1.662695954554818778 ) ) ;
#20999 = VECTOR ( 'NONE', #1534, 1000.000000000000000 ) ;
#21000 = ADVANCED_FACE ( 'NONE', ( #13526 ), #15254, .F. ) ;
#21001 = CARTESIAN_POINT ( 'NONE',  ( 4.742907322181076246, -28.05233206275141811, 6.979335674598003969 ) ) ;
#21002 = ORIENTED_EDGE ( 'NONE', *, *, #12175, .T. ) ;
#21004 = CARTESIAN_POINT ( 'NONE',  ( 17.03255388622768507, -3.044842113014305962, -2.864739986454959642 ) ) ;
#21003 = CARTESIAN_POINT ( 'NONE',  ( -0.02095206919630761971, -26.63786329112441820, 7.740055089680397238 ) ) ;
#21005 = CARTESIAN_POINT ( 'NONE',  ( -70.92837670882107659, 13.87661300689593880, -6.000000000000005329 ) ) ;
#21006 = CARTESIAN_POINT ( 'NONE',  ( 74.72645207833699033, 61.69672356374137223, 3.865308561588414182 ) ) ;
#21007 = ORIENTED_EDGE ( 'NONE', *, *, #13033, .T. ) ;
#21008 = CARTESIAN_POINT ( 'NONE',  ( 22.04800161786629431, 2.700078594769402152, -5.146687023986929788 ) ) ;
#21009 = VERTEX_POINT ( 'NONE', #11219 ) ;
#21010 = CARTESIAN_POINT ( 'NONE',  ( 0.5134882369223120469, -26.38382311207955411, 7.652160403243385645 ) ) ;
#21011 = DIRECTION ( 'NONE',  ( -0.000000000000000000, -0.000000000000000000, -1.000000000000000000 ) ) ;
#21012 = AXIS2_PLACEMENT_3D ( 'NONE', #39105, #17075, #5146 ) ;
#21013 = DIRECTION ( 'NONE',  ( -0.000000000000000000, -0.000000000000000000, 1.000000000000000000 ) ) ;
#21014 = ORIENTED_EDGE ( 'NONE', *, *, #35802, .T. ) ;
#21015 = CARTESIAN_POINT ( 'NONE',  ( -65.62105494222964808, 35.19887319331469655, 7.481751891072599747 ) ) ;
#21016 = ADVANCED_BREP_SHAPE_REPRESENTATION ( '', ( #26623, #30744 ), #31385 ) ;
#21017 = CARTESIAN_POINT ( 'NONE',  ( 81.96106518217335690, 62.90574382782723717, 2.573500632437473623 ) ) ;
#21018 = CARTESIAN_POINT ( 'NONE',  ( 85.11099552155531001, 2.757014815357352155, -1.204572545719858834 ) ) ;
#21019 = PLANE ( 'NONE',  #9628 ) ;
#21020 = CARTESIAN_POINT ( 'NONE',  ( -70.92837670882107659, 13.87661300689593880, 0.000000000000000000 ) ) ;
#21021 = EDGE_CURVE ( 'NONE', #40083, #153, #8131, .T. ) ;
#21022 = ADVANCED_FACE ( 'NONE', ( #20294 ), #7545, .F. ) ;
#21023 = DIRECTION ( 'NONE',  ( -0.1736481776669206722, -0.9848077530122096857, -0.000000000000000000 ) ) ;
#21024 = ORIENTED_EDGE ( 'NONE', *, *, #7675, .T. ) ;
#21025 = CARTESIAN_POINT ( 'NONE',  ( 15.15534889434650090, -4.116562409201322659, 2.560140338179660358 ) ) ;
#21026 = CARTESIAN_POINT ( 'NONE',  ( 0.01496732657086547076, -26.50244713504975635, 6.867280401193706751 ) ) ;
#21027 = ADVANCED_FACE ( 'NONE', ( #17000 ), #33285, .T. ) ;
#21028 = CARTESIAN_POINT ( 'NONE',  ( 37.07067537406068425, -2.906362785499426060, -5.992173468430849859 ) ) ;
#21029 = CARTESIAN_POINT ( 'NONE',  ( 6.112940767310136359, -27.90626689514689218, 7.695279973900954751 ) ) ;
#21030 = CARTESIAN_POINT ( 'NONE',  ( 4.651387254527720394, -31.45187073487890217, 6.880828092187094569 ) ) ;
#21031 = DIRECTION ( 'NONE',  ( -0.000000000000000000, -0.000000000000000000, 1.000000000000000000 ) ) ;
#21033 = VECTOR ( 'NONE', #22392, 1000.000000000000000 ) ;
#21032 = CARTESIAN_POINT ( 'NONE',  ( -70.92837670882107659, -23.80776546975053165, 0.000000000000000000 ) ) ;
#21034 = DIRECTION ( 'NONE',  ( 0.8660254037844380415, 0.5000000000000009992, -0.000000000000000000 ) ) ;
#21035 = EDGE_LOOP ( 'NONE', ( #9490, #6149, #37791, #18293, #40572 ) ) ;
#21036 = CARTESIAN_POINT ( 'NONE',  ( 30.84889139629300558, 0.6455805249289596759, 4.592240215719487040 ) ) ;
#21037 =( BOUNDED_CURVE ( )  B_SPLINE_CURVE ( 3, ( #6711, #38583, #29539, #542 ),
 .UNSPECIFIED., .F., .T. ) 
 B_SPLINE_CURVE_WITH_KNOTS ( ( 4, 4 ),
 ( 1.347909859412854239, 1.534781240595298968 ),
 .UNSPECIFIED. ) 
 CURVE ( )  GEOMETRIC_REPRESENTATION_ITEM ( )  RATIONAL_B_SPLINE_CURVE ( ( 1.000000000000000000, 0.9970920404276226723, 0.9970920404276226723, 1.000000000000000000 ) ) 
 REPRESENTATION_ITEM ( '' )  );
#21038 = CARTESIAN_POINT ( 'NONE',  ( -71.25654746924473670, 0.1680418597759353594, 3.991851897078962708 ) ) ;
#21039 = CARTESIAN_POINT ( 'NONE',  ( 66.72344311391505300, 57.86780257000127392, -3.999628797551961767 ) ) ;
#21040 = CARTESIAN_POINT ( 'NONE',  ( -0.6434037460695107846, -32.16928249125778194, 7.751599049952175413 ) ) ;
#21041 = EDGE_LOOP ( 'NONE', ( #28693, #37071, #12680, #10000, #5999 ) ) ;
#21042 = CARTESIAN_POINT ( 'NONE',  ( -0.5155868758681084740, -32.14860049917209750, 7.784838882742138644 ) ) ;
#21043 = AXIS2_PLACEMENT_3D ( 'NONE', #12395, #21872, #37694 ) ;
#21044 = CARTESIAN_POINT ( 'NONE',  ( 3.847093746412449722, -32.20655010317304345, 7.785868773668303433 ) ) ;
#21045 = CARTESIAN_POINT ( 'NONE',  ( 18.54789246542846470, 7.518219598317671171, 3.101245220341271036 ) ) ;
#21046 = CARTESIAN_POINT ( 'NONE',  ( -73.59524413808043164, 8.148159543145636619, 9.640765774018305478 ) ) ;
#21047 = PLANE ( 'NONE',  #18188 ) ;
#21048 = VERTEX_POINT ( 'NONE', #39429 ) ;
#21049 = CARTESIAN_POINT ( 'NONE',  ( 2.817328913877361618, -32.78123018042540338, 6.894806418505346812 ) ) ;
#21050 = CARTESIAN_POINT ( 'NONE',  ( -8.448748702180639114, -26.64985754041175525, 6.700000000000000178 ) ) ;
#21051 = EDGE_LOOP ( 'NONE', ( #365, #29724, #1824, #28012 ) ) ;
#21052 = CARTESIAN_POINT ( 'NONE',  ( 21.99994241389349980, 5.558807285328593473, 3.121874822124243387 ) ) ;
#21053 = CARTESIAN_POINT ( 'NONE',  ( 82.09527124944445120, 65.20214329949099863, -1.328060019258380242 ) ) ;
#21054 = CARTESIAN_POINT ( 'NONE',  ( 81.18881611591316982, 61.34569122823197773, 1.520709669156496968 ) ) ;
#21055 = CARTESIAN_POINT ( 'NONE',  ( -0.04165398999324298329, -32.48973880933039737, 6.894806418505347700 ) ) ;
#21056 = EDGE_LOOP ( 'NONE', ( #32132, #40060, #38502, #33437 ) ) ;
#21057 = CARTESIAN_POINT ( 'NONE',  ( 77.93772202372294089, 64.31926776197542495, -3.361664161258271388 ) ) ;
#21059 = CARTESIAN_POINT ( 'NONE',  ( 14.69507384520581361, -4.883229594507451310, -2.499999999999376055 ) ) ;
#21058 = CARTESIAN_POINT ( 'NONE',  ( 21.73405496294427053, 0.2198986141765594815, 9.095395277813500101 ) ) ;
#21060 = CARTESIAN_POINT ( 'NONE',  ( 80.86168855680497813, 64.16696250863120099, -3.456914256419914011 ) ) ;
#21061 = CARTESIAN_POINT ( 'NONE',  ( 79.66831987096976775, 61.58041732747442865, 3.164065397988992778 ) ) ;
#21062 = ORIENTED_EDGE ( 'NONE', *, *, #12983, .F. ) ;
#21064 = CARTESIAN_POINT ( 'NONE',  ( 0.7201709579117279159, -51.60714625320436255, 2.500000000000000000 ) ) ;
#21063 = ADVANCED_BREP_SHAPE_REPRESENTATION ( '', ( #12876, #30744 ), #18883 ) ;
#21065 = CARTESIAN_POINT ( 'NONE',  ( 80.99740051111626826, 66.07939114927827973, 1.509105202934762024 ) ) ;
#21067 = CARTESIAN_POINT ( 'NONE',  ( -13.07867591359219617, -26.64985754041175525, 6.800000000000000711 ) ) ;
#21066 = CARTESIAN_POINT ( 'NONE',  ( 3.410047845041411563, -26.63102917700635430, 7.775108481317166031 ) ) ;
#21068 = CARTESIAN_POINT ( 'NONE',  ( 31.28551011801044268, -2.837290201336624129, -5.599793116354693012 ) ) ;
#21069 = CARTESIAN_POINT ( 'NONE',  ( -1.769892952498073768, -30.02514449314797673, 6.880828092187097234 ) ) ;
#21070 = LINE ( 'NONE', #17543, #14740 ) ;
#21071 = CARTESIAN_POINT ( 'NONE',  ( -80.68515367620979362, -6.621186074883498307, 2.228965439759364564 ) ) ;
#21072 = CARTESIAN_POINT ( 'NONE',  ( 24.12565218530084366, 0.5136036009149196335, -5.092665358616495830 ) ) ;
#21073 = ADVANCED_FACE ( 'NONE', ( #39637 ), #29769, .F. ) ;
#21074 = LINE ( 'NONE', #21691, #1165 ) ;
#21075 = DIRECTION ( 'NONE',  ( -1.000000000000000000, -1.241493069327139093E-16, 0.000000000000000000 ) ) ;
#21076 = CARTESIAN_POINT ( 'NONE',  ( -1.060034464505671403, -31.72168673584834053, 7.750000000000000888 ) ) ;
#21077 = AXIS2_PLACEMENT_3D ( 'NONE', #35726, #1156, #10982 ) ;
#21078 = EDGE_CURVE ( 'NONE', #17881, #5880, #39229, .T. ) ;
#21079 = FACE_BOUND ( 'NONE', #15062, .T. ) ;
#21080 = CARTESIAN_POINT ( 'NONE',  ( 36.13131606425951503, -1.533108014538433039, -5.645148619362555742 ) ) ;
#21081 = CARTESIAN_POINT ( 'NONE',  ( 3.391251241177835940, -32.61740345834337518, 7.785593909369613819 ) ) ;
#21082 = CARTESIAN_POINT ( 'NONE',  ( 0.9689046511080217083, -32.99263803653528271, 7.750000000000000888 ) ) ;
#21083 = CYLINDRICAL_SURFACE ( 'NONE', #36457, 83.68529983683480111 ) ;
#21084 = DIRECTION ( 'NONE',  ( 1.000000000000000000, 0.000000000000000000, -0.000000000000000000 ) ) ;
#21085 = CARTESIAN_POINT ( 'NONE',  ( 2.670334759559959803, -32.82864271202553397, 6.988553391373221402 ) ) ;
#21086 = CARTESIAN_POINT ( 'NONE',  ( 4.626750114682200987, -27.83891399941946077, 7.692469944509199742 ) ) ;
#21087 = CARTESIAN_POINT ( 'NONE',  ( 4.888877264403690859, -28.38944318249906118, 7.748216051605119503 ) ) ;
#21088 = LINE ( 'NONE', #33659, #5986 ) ;
#21089 = CARTESIAN_POINT ( 'NONE',  ( 22.81770739701413930, 1.428927919918285605, -5.507341944819657442 ) ) ;
#21090 = ORIENTED_EDGE ( 'NONE', *, *, #12422, .T. ) ;
#21091 = CARTESIAN_POINT ( 'NONE',  ( 66.43286826475038254, 57.76021747899728354, 4.000000000000004441 ) ) ;
#21092 = CARTESIAN_POINT ( 'NONE',  ( 69.17602579976487220, 58.86946863987066791, -3.990151341881416514 ) ) ;
#21093 = AXIS2_PLACEMENT_3D ( 'NONE', #12668, #25242, #22771 ) ;
#21094 = LINE ( 'NONE', #33664, #25362 ) ;
#21095 = ORIENTED_EDGE ( 'NONE', *, *, #37936, .F. ) ;
#21096 = DIRECTION ( 'NONE',  ( 0.000000000000000000, 1.000000000000000000, 0.000000000000000000 ) ) ;
#21097 = CARTESIAN_POINT ( 'NONE',  ( 0.1859022642979256124, -26.52586597056204099, 6.949473656533218247 ) ) ;
#21098 = CARTESIAN_POINT ( 'NONE',  ( -70.53519588576141075, -48.57790317178756823, 9.993926770235830759 ) ) ;
#21099 = CARTESIAN_POINT ( 'NONE',  ( 1.700390093233090871, -29.56993018339339940, 6.000000000000000000 ) ) ;
#21101 = CARTESIAN_POINT ( 'NONE',  ( 1.318368334477774573, -26.19146016107992025, 6.949473656533216470 ) ) ;
#21100 = CARTESIAN_POINT ( 'NONE',  ( -75.45330471031414277, 33.71485196875532608, -12.49999999999999645 ) ) ;
#21102 = EDGE_CURVE ( 'NONE', #26823, #19049, #17599, .T. ) ;
#21103 = APPLICATION_PROTOCOL_DEFINITION ( 'draft international standard', 'automotive_design', 1998, #13950 ) ;
#21104 = PLANE ( 'NONE',  #27792 ) ;
#21105 = EDGE_LOOP ( 'NONE', ( #18890, #28566, #35852, #24371 ) ) ;
#21106 = CARTESIAN_POINT ( 'NONE',  ( 7.121324086407810228, -26.64985754041175525, 6.700000000000000178 ) ) ;
#21107 = DIRECTION ( 'NONE',  ( -1.000000000000000000, -0.000000000000000000, -0.000000000000000000 ) ) ;
#21108 = CIRCLE ( 'NONE', #3393, 10.99999999999998224 ) ;
#21109 = ORIENTED_EDGE ( 'NONE', *, *, #37990, .F. ) ;
#21110 = CARTESIAN_POINT ( 'NONE',  ( 79.08605325858584933, 64.90301710537214319, -3.311815948186460190 ) ) ;
#21111 = CARTESIAN_POINT ( 'NONE',  ( 17.73639088777611761, 11.88077751880594768, -2.499999999999990230 ) ) ;
#21112 = CARTESIAN_POINT ( 'NONE',  ( 81.16598293928451824, 61.30266375757629049, -1.057717897339658153 ) ) ;
#21113 = CARTESIAN_POINT ( 'NONE',  ( 80.70428644432419674, 61.65645308977151728, 2.679976076788563866 ) ) ;
#21114 = CARTESIAN_POINT ( 'NONE',  ( 23.94692112590556832, 2.808164783556298616, 3.943894218810308328 ) ) ;
#21116 = ORIENTED_EDGE ( 'NONE', *, *, #26172, .T. ) ;
#21115 = CARTESIAN_POINT ( 'NONE',  ( 17.35960385848256493, 14.27653579843486220, 2.500000000000000444 ) ) ;
#21117 = CARTESIAN_POINT ( 'NONE',  ( 21.85643539959774273, 9.214175136349357587, -0.8338435668127727185 ) ) ;
#21118 = EDGE_LOOP ( 'NONE', ( #17467, #27764, #12115, #38490 ) ) ;
#21119 = DIRECTION ( 'NONE',  ( 0.000000000000000000, 0.000000000000000000, -1.000000000000000000 ) ) ;
#21120 = AXIS2_PLACEMENT_3D ( 'NONE', #4339, #39090, #36029 ) ;
#21121 = CARTESIAN_POINT ( 'NONE',  ( 14.75290036705818508, -5.144397853053700231, 2.500000000000000444 ) ) ;
#21122 = CARTESIAN_POINT ( 'NONE',  ( -74.02478150447711869, 6.647606516902553331, -9.563567244161919945 ) ) ;
#21123 = ADVANCED_FACE ( 'NONE', ( #20100 ), #32476, .F. ) ;
#21124 = CARTESIAN_POINT ( 'NONE',  ( -0.1779045157466759008, -32.41245094751727862, 7.386948897581450346 ) ) ;
#21125 = CARTESIAN_POINT ( 'NONE',  ( 2.403116422957143783, -26.24334398948340663, 6.864276522220859711 ) ) ;
#21126 = CARTESIAN_POINT ( 'NONE',  ( -1.746590121550728236, -30.10122404981289534, 7.782861076432730840 ) ) ;
#21127 = CARTESIAN_POINT ( 'NONE',  ( 14.89578813002483670, 12.34317254588458468, 2.524919271954451094 ) ) ;
#21128 = CARTESIAN_POINT ( 'NONE',  ( -1.391746016950013320, -31.20965402480746320, 7.750000000000000888 ) ) ;
#21129 = CARTESIAN_POINT ( 'NONE',  ( 0.6641905360584041684, -26.22683424134941177, 6.895394898881668233 ) ) ;
#21130 = CARTESIAN_POINT ( 'NONE',  ( -0.4067295501017070269, -32.37312860990524399, 7.139344958878410807 ) ) ;
#21131 = CARTESIAN_POINT ( 'NONE',  ( 16.38665980882106155, 15.06251823374549303, -2.500000000000000000 ) ) ;
#21132 = VECTOR ( 'NONE', #22425, 1000.000000000000000 ) ;
#21133 = CARTESIAN_POINT ( 'NONE',  ( 87.08948198750766778, 0.5346849121671046756, 4.856188771401600768 ) ) ;
#21134 = CARTESIAN_POINT ( 'NONE',  ( 26.49611857872572784, 1.696983071862875336, -4.309887170283649205 ) ) ;
#21135 = ORIENTED_EDGE ( 'NONE', *, *, #2009, .T. ) ;
#21136 = ORIENTED_EDGE ( 'NONE', *, *, #23953, .T. ) ;
#21137 = CARTESIAN_POINT ( 'NONE',  ( 68.06744372826909739, 58.27867795456629807, 3.994255761866622123 ) ) ;
#21138 = CARTESIAN_POINT ( 'NONE',  ( 35.33522366009476912, -3.174037382202389512, 5.721314256408138732 ) ) ;
#21139 = DIRECTION ( 'NONE',  ( 0.000000000000000000, 0.000000000000000000, 1.000000000000000000 ) ) ;
#21140 = CARTESIAN_POINT ( 'NONE',  ( 85.55911739799610416, 1.969564878966352905, 4.951173091362058187 ) ) ;
#21142 = FACE_OUTER_BOUND ( 'NONE', #9904, .T. ) ;
#21141 = DIRECTION ( 'NONE',  ( -0.000000000000000000, -0.000000000000000000, 1.000000000000000000 ) ) ;
#21143 = FACE_OUTER_BOUND ( 'NONE', #38203, .T. ) ;
#21144 = CARTESIAN_POINT ( 'NONE',  ( 3.651251297819360531, -25.49307895267003587, 6.700000000000000178 ) ) ;
#21145 = CARTESIAN_POINT ( 'NONE',  ( -0.6518040451976112593, -32.16169936346016556, 6.870724624169667116 ) ) ;
#21146 = ORIENTED_EDGE ( 'NONE', *, *, #20044, .F. ) ;
#21147 = CARTESIAN_POINT ( 'NONE',  ( -70.08069538478937943, -21.32521480519122647, 3.940028962036594251 ) ) ;
#21148 = ORIENTED_EDGE ( 'NONE', *, *, #39453, .T. ) ;
#21149 = VERTEX_POINT ( 'NONE', #1789 ) ;
#21150 = CARTESIAN_POINT ( 'NONE',  ( 80.21880177947251411, 63.46656020078422955, -3.697630003121159081 ) ) ;
#21151 = EDGE_CURVE ( 'NONE', #23320, #28333, #37795, .T. ) ;
#21152 = CARTESIAN_POINT ( 'NONE',  ( 4.932354078450567059, -25.52873147056503811, 7.754798119455333705 ) ) ;
#21153 = CARTESIAN_POINT ( 'NONE',  ( 79.30978077413506355, 65.08723789429433282, 3.243225924683099226 ) ) ;
#21154 = CARTESIAN_POINT ( 'NONE',  ( 25.33366054371228770, 0.7754436759679742552, 4.607944210112060013 ) ) ;
#21155 = VERTEX_POINT ( 'NONE', #7942 ) ;
#21156 = EDGE_CURVE ( 'NONE', #8770, #25652, #20056, .T. ) ;
#21157 = CARTESIAN_POINT ( 'NONE',  ( 73.33958664722344167, 61.75625940721955942, -3.692213121420756305 ) ) ;
#21158 = VECTOR ( 'NONE', #11867, 1000.000000000000000 ) ;
#21159 = LINE ( 'NONE', #33938, #35792 ) ;
#21161 = CARTESIAN_POINT ( 'NONE',  ( 1.700390093233090871, -29.56993018339339940, 7.800000000000000711 ) ) ;
#21160 = CARTESIAN_POINT ( 'NONE',  ( 4.970031525767722336, -30.81870754651817990, 6.875671892026065102 ) ) ;
#21162 = PLANE ( 'NONE',  #15242 ) ;
#21163 = DIRECTION ( 'NONE',  ( -1.000000000000000000, 0.000000000000000000, -0.000000000000000000 ) ) ;
#21164 = CARTESIAN_POINT ( 'NONE',  ( -1.584315626793068921, -30.77853884495590719, 7.756742906098588186 ) ) ;
#21165 = CARTESIAN_POINT ( 'NONE',  ( 24.00944515006052171, 3.309123255076573678, -3.353452565180164324 ) ) ;
#21166 = VERTEX_POINT ( 'NONE', #33076 ) ;
#21167 = CARTESIAN_POINT ( 'NONE',  ( -1.797390937478270612, -29.44531139368447725, 7.751599049952198506 ) ) ;
#21168 = CARTESIAN_POINT ( 'NONE',  ( 24.43802896994273510, -0.4903351684736660387, 6.966919456710074954 ) ) ;
#21169 = DIRECTION ( 'NONE',  ( 1.165409145176969993E-16, -1.000000000000000000, 0.000000000000000000 ) ) ;
#21170 = EDGE_CURVE ( 'NONE', #27620, #36238, #22036, .T. ) ;
#21171 = DIRECTION ( 'NONE',  ( 0.000000000000000000, 0.000000000000000000, 1.000000000000000000 ) ) ;
#21172 = CARTESIAN_POINT ( 'NONE',  ( 81.42004705248814389, 62.63944267392375309, 2.989933650883211502 ) ) ;
#21173 = CARTESIAN_POINT ( 'NONE',  ( 86.42495861400665547, -0.1300389677119091758, -5.942483626122943896 ) ) ;
#21174 = FACE_OUTER_BOUND ( 'NONE', #6258, .T. ) ;
#21175 = VERTEX_POINT ( 'NONE', #24613 ) ;
#21176 = CARTESIAN_POINT ( 'NONE',  ( -32.87867591359218977, -26.64985754041175525, 6.700000000000000178 ) ) ;
#21177 = CARTESIAN_POINT ( 'NONE',  ( 4.079964913973585183, -27.00329292675143478, 7.009310105710486738 ) ) ;
#21178 = CARTESIAN_POINT ( 'NONE',  ( 14.85208526505567050, -4.487224198574636169, -2.516407688438223822 ) ) ;
#21179 = CARTESIAN_POINT ( 'NONE',  ( -67.57960606288774841, 36.15173574121457989, -8.626892781891035256 ) ) ;
#21180 = DIRECTION ( 'NONE',  ( -0.000000000000000000, 0.000000000000000000, -1.000000000000000000 ) ) ;
#21181 = CARTESIAN_POINT ( 'NONE',  ( -0.4618072112497045301, -26.94602034948383107, 7.782167645815904145 ) ) ;
#21182 = ORIENTED_EDGE ( 'NONE', *, *, #14061, .T. ) ;
#21183 = CARTESIAN_POINT ( 'NONE',  ( 2.844063789200206749, -32.86231350904720472, 7.785344483711591934 ) ) ;
#21184 = EDGE_CURVE ( 'NONE', #2141, #37191, #21739, .T. ) ;
#21185 = CARTESIAN_POINT ( 'NONE',  ( 85.52484820210342775, 2.292155841932438154, 3.149942891487422791 ) ) ;
#21186 = VERTEX_POINT ( 'NONE', #18425 ) ;
#21187 = EDGE_LOOP ( 'NONE', ( #5322, #29399, #19540, #12502, #15015, #4111 ) ) ;
#21189 = CARTESIAN_POINT ( 'NONE',  ( 36.49369427451753722, -3.560799718971868089, 5.796041169543606486 ) ) ;
#21188 = CARTESIAN_POINT ( 'NONE',  ( 80.45774067191287315, 64.33927723362793927, -3.562450064734666189 ) ) ;
#21190 = CARTESIAN_POINT ( 'NONE',  ( 19.68761177061032086, -2.696979717695116463, 3.279125982130457473 ) ) ;
#21191 = CARTESIAN_POINT ( 'NONE',  ( 20.50705206718803808, -3.049029319690857776, -3.332098049053498823 ) ) ;
#21192 = AXIS2_PLACEMENT_3D ( 'NONE', #25960, #34841, #852 ) ;
#21193 = CYLINDRICAL_SURFACE ( 'NONE', #29041, 0.1000000000000028644 ) ;
#21194 = VERTEX_POINT ( 'NONE', #24201 ) ;
#21195 = DIRECTION ( 'NONE',  ( 1.000000000000000000, 0.000000000000000000, -0.000000000000000000 ) ) ;
#21196 = VERTEX_POINT ( 'NONE', #5889 ) ;
#21197 = ORIENTED_EDGE ( 'NONE', *, *, #6153, .F. ) ;
#21198 = CARTESIAN_POINT ( 'NONE',  ( 0.03112795225476835265, -32.53195046136271174, 7.680992449362118890 ) ) ;
#21199 = CARTESIAN_POINT ( 'NONE',  ( 79.04990754624076033, 65.77731930041099417, -2.468641556982019480 ) ) ;
#21200 = CARTESIAN_POINT ( 'NONE',  ( 14.77222811005485603, -4.461988841550141416, 2.511961482897715481 ) ) ;
#21201 = ORIENTED_EDGE ( 'NONE', *, *, #6383, .T. ) ;
#21203 = CARTESIAN_POINT ( 'NONE',  ( 21.33678673121765712, 8.399421056148055342, -2.668923178601029456 ) ) ;
#21202 = CARTESIAN_POINT ( 'NONE',  ( 24.71742244748645945, 2.639037666618674116, 3.924515567304096120 ) ) ;
#21204 = ORIENTED_EDGE ( 'NONE', *, *, #22298, .T. ) ;
#21205 = ADVANCED_FACE ( 'NONE', ( #34320 ), #15059, .T. ) ;
#21206 = CARTESIAN_POINT ( 'NONE',  ( 81.57551674523598706, 65.32158946912282715, -2.325514254129002367 ) ) ;
#21207 = DIRECTION ( 'NONE',  ( -0.000000000000000000, -1.000000000000000000, -0.000000000000000000 ) ) ;
#21208 = EDGE_LOOP ( 'NONE', ( #32543, #28760, #25166, #39087 ) ) ;
#21210 = CARTESIAN_POINT ( 'NONE',  ( 21.57378257072032213, -2.652646515802797200, -3.573508552700807250 ) ) ;
#21209 = DIRECTION ( 'NONE',  ( 0.000000000000000000, 0.000000000000000000, 1.000000000000000000 ) ) ;
#21211 = FACE_OUTER_BOUND ( 'NONE', #518, .T. ) ;
#21212 = CARTESIAN_POINT ( 'NONE',  ( 74.43259725886051115, 60.83706718145764114, 3.924711207976804950 ) ) ;
#21213 = CARTESIAN_POINT ( 'NONE',  ( 22.03527598358551387, 3.722255905023069911, -4.359252203237127254 ) ) ;
#21214 = EDGE_LOOP ( 'NONE', ( #21706, #12801, #28365, #33490 ) ) ;
#21215 = CARTESIAN_POINT ( 'NONE',  ( 21.85643539959774273, 11.92045248574714300, 0.01447246376323708950 ) ) ;
#21216 = LINE ( 'NONE', #39944, #18391 ) ;
#21217 = VERTEX_POINT ( 'NONE', #9363 ) ;
#21218 = CARTESIAN_POINT ( 'NONE',  ( -68.33309634913140940, 36.51831931741379833, 8.800414904976364028 ) ) ;
#21219 = CARTESIAN_POINT ( 'NONE',  ( 82.03499260127753701, 62.66326407617584238, 2.270757614041261530 ) ) ;
#21220 = CARTESIAN_POINT ( 'NONE',  ( 85.09863483756090830, 2.770898922293168809, 1.806811963633389695 ) ) ;
#21221 = CARTESIAN_POINT ( 'NONE',  ( -35.07867591359219972, -24.55319635012989110, 6.800000000000000711 ) ) ;
#21222 = LINE ( 'NONE', #14613, #21451 ) ;
#21223 = VECTOR ( 'NONE', #6421, 1000.000000000000000 ) ;
#21224 = CARTESIAN_POINT ( 'NONE',  ( -51.21549048184568420, -30.38627270959228710, 6.000000000000000000 ) ) ;
#21225 = ORIENTED_EDGE ( 'NONE', *, *, #32206, .T. ) ;
#21226 = CARTESIAN_POINT ( 'NONE',  ( 31.37373683152652148, -3.593601361316209886, 4.916934954046649153 ) ) ;
#21227 = LINE ( 'NONE', #34011, #26301 ) ;
#21228 = CARTESIAN_POINT ( 'NONE',  ( 36.63366809872980667, -3.081676326702182056, -5.923967914054548700 ) ) ;
#21229 =( LENGTH_UNIT ( ) NAMED_UNIT ( * ) SI_UNIT ( .MILLI., .METRE. ) );
#21230 = CARTESIAN_POINT ( 'NONE',  ( 5.197197318687171830, -29.57030403941794461, 7.767581361668585593 ) ) ;
#21231 = CARTESIAN_POINT ( 'NONE',  ( -70.92837670882107659, -56.35932253828835314, 0.000000000000000000 ) ) ;
#21232 = DIRECTION ( 'NONE',  ( 1.000000000000000000, 0.000000000000000000, 0.000000000000000000 ) ) ;
#21233 = DIRECTION ( 'NONE',  ( 0.000000000000000000, 0.000000000000000000, 1.000000000000000000 ) ) ;
#21234 = ORIENTED_EDGE ( 'NONE', *, *, #22574, .T. ) ;
#21235 = CARTESIAN_POINT ( 'NONE',  ( 30.81594338096673980, 0.5927415480317952401, 4.684896961509361191 ) ) ;
#21236 = CARTESIAN_POINT ( 'NONE',  ( -71.92133747557326728, -0.6645477131579885510, 5.929309462487116100 ) ) ;
#21237 = CARTESIAN_POINT ( 'NONE',  ( 66.99808371854801692, 58.02529356684345885, -3.999241514195644331 ) ) ;
#21238 = EDGE_CURVE ( 'NONE', #10219, #25277, #10170, .T. ) ;
#21239 = FACE_OUTER_BOUND ( 'NONE', #3923, .T. ) ;
#21240 = CARTESIAN_POINT ( 'NONE',  ( -59.01947560891952804, 27.90920910948504385, -6.147301388271595890 ) ) ;
#21241 = ORIENTED_EDGE ( 'NONE', *, *, #37504, .F. ) ;
#21242 = LINE ( 'NONE', #40171, #291 ) ;
#21243 = EDGE_CURVE ( 'NONE', #12529, #32500, #20685, .T. ) ;
#21244 = CARTESIAN_POINT ( 'NONE',  ( -73.55410448504031251, 8.091590788868597173, -9.651951412758178250 ) ) ;
#21245 = CARTESIAN_POINT ( 'NONE',  ( -71.43156905789128075, -21.65680325503002734, 5.980078429000514006 ) ) ;
#21246 = DIRECTION ( 'NONE',  ( -1.000000000000000000, 0.000000000000000000, 0.000000000000000000 ) ) ;
#21247 = ORIENTED_EDGE ( 'NONE', *, *, #30090, .T. ) ;
#21248 = LINE ( 'NONE', #18345, #36542 ) ;
#21249 = AXIS2_PLACEMENT_3D ( 'NONE', #6012, #3365, #2742 ) ;
#21250 = PLANE ( 'NONE',  #9393 ) ;
#21251 = ORIENTED_EDGE ( 'NONE', *, *, #18544, .T. ) ;
#21252 = CARTESIAN_POINT ( 'NONE',  ( 24.03985768575755344, 3.329662727276597511, 3.280238031040798141 ) ) ;
#21253 = EDGE_CURVE ( 'NONE', #33252, #40099, #15959, .T. ) ;
#21254 = CARTESIAN_POINT ( 'NONE',  ( 82.54681503119213914, 63.20390409618730132, -1.263752851813363609 ) ) ;
#21255 = CARTESIAN_POINT ( 'NONE',  ( 79.49612969957790654, 65.22981380272329943, 3.178394274514609208 ) ) ;
#21256 = EDGE_CURVE ( 'NONE', #6532, #27165, #13713, .T. ) ;
#21257 = CARTESIAN_POINT ( 'NONE',  ( 24.05471417302198489, 3.308817292245012975, -3.187513558550173265 ) ) ;
#21258 = ORIENTED_EDGE ( 'NONE', *, *, #32114, .T. ) ;
#21259 = CARTESIAN_POINT ( 'NONE',  ( 78.76819457884754172, 61.97782169454064416, -3.640295653904960904 ) ) ;
#21261 = CARTESIAN_POINT ( 'NONE',  ( 2.270926882672761771, -26.21813482148259311, 7.643333865083956624 ) ) ;
#21260 = CARTESIAN_POINT ( 'NONE',  ( 23.04769222910721993, 0.3307062739915670457, 5.968048623999395730 ) ) ;
#21262 = CARTESIAN_POINT ( 'NONE',  ( 81.49799543786826916, 62.67690593247225905, -2.943961322783049450 ) ) ;
#21263 = CARTESIAN_POINT ( 'NONE',  ( 78.50009633871025017, 63.24008633025189852, 3.804514705604313374 ) ) ;
#21264 = ORIENTED_EDGE ( 'NONE', *, *, #9302, .F. ) ;
#21265 = CIRCLE ( 'NONE', #31798, 3.499999999999999556 ) ;
#21266 = CARTESIAN_POINT ( 'NONE',  ( 35.34196908527864878, -3.786851321365131806, -5.507838251830221132 ) ) ;
#21267 = VECTOR ( 'NONE', #38764, 1000.000000000000000 ) ;
#21268 = CARTESIAN_POINT ( 'NONE',  ( 81.56437483599492566, 65.67932636690383674, 1.586031901069098193 ) ) ;
#21271 = ORIENTED_EDGE ( 'NONE', *, *, #23474, .T. ) ;
#21270 = DIRECTION ( 'NONE',  ( 0.000000000000000000, 0.000000000000000000, 1.000000000000000000 ) ) ;
#21269 = FACE_OUTER_BOUND ( 'NONE', #14925, .T. ) ;
#21272 = CARTESIAN_POINT ( 'NONE',  ( 29.46612689758034875, 1.430465584783186639, -3.840811867917949929 ) ) ;
#21273 = CARTESIAN_POINT ( 'NONE',  ( -1.774560659206035451, -29.98792227883944150, 6.941203072598477242 ) ) ;
#21274 = DIRECTION ( 'NONE',  ( 0.000000000000000000, 0.000000000000000000, 1.000000000000000000 ) ) ;
#21275 = CARTESIAN_POINT ( 'NONE',  ( 1.555264031125473068, -33.06692009274359378, 6.875780273367531947 ) ) ;
#21276 = CARTESIAN_POINT ( 'NONE',  ( 25.36727076954679916, 0.7411443615474921920, -4.603813888107473495 ) ) ;
#21277 = FACE_OUTER_BOUND ( 'NONE', #18434, .T. ) ;
#21278 = CARTESIAN_POINT ( 'NONE',  ( 4.998126050557230471, -30.74251124864294837, 7.737115613922533441 ) ) ;
#21279 = CARTESIAN_POINT ( 'NONE',  ( 5.198144250753316875, -29.69314003934108470, 7.753200566781576875 ) ) ;
#21280 = FACE_OUTER_BOUND ( 'NONE', #33964, .T. ) ;
#21281 = CARTESIAN_POINT ( 'NONE',  ( 35.16097584309888902, -1.161037321149452239, -5.517930166532758918 ) ) ;
#21282 = DIRECTION ( 'NONE',  ( -0.5000000000000039968, 0.8660254037844363761, -0.000000000000000000 ) ) ;
#21283 = CARTESIAN_POINT ( 'NONE',  ( 5.200344093257736056, -29.59065050415977538, 6.906385212079477753 ) ) ;
#21284 = DIRECTION ( 'NONE',  ( -0.000000000000000000, -0.000000000000000000, 1.000000000000000000 ) ) ;
#21285 =( BOUNDED_CURVE ( )  B_SPLINE_CURVE ( 3, ( #40548, #15038, #12360, #39956 ),
 .UNSPECIFIED., .F., .T. ) 
 B_SPLINE_CURVE_WITH_KNOTS ( ( 4, 4 ),
 ( 1.396263401595456699, 1.574767692156075594 ),
 .UNSPECIFIED. ) 
 CURVE ( )  GEOMETRIC_REPRESENTATION_ITEM ( )  RATIONAL_B_SPLINE_CURVE ( ( 1.000000000000000000, 0.9973464470609390009, 0.9973464470609390009, 1.000000000000000000 ) ) 
 REPRESENTATION_ITEM ( '' )  );
#21286 = DIRECTION ( 'NONE',  ( 0.3420201433256790380, -0.9396926207859046531, -0.000000000000000000 ) ) ;
#21287 = CARTESIAN_POINT ( 'NONE',  ( -33.07867591359219972, -24.55319635012989110, 6.800000000000000711 ) ) ;
#21288 = CARTESIAN_POINT ( 'NONE',  ( -14.87867591359218977, -26.64985754041175525, 6.700000000000000178 ) ) ;
#21289 = PLANE ( 'NONE',  #24803 ) ;
#21290 = CARTESIAN_POINT ( 'NONE',  ( 14.76475291679427393, -5.159125289594414632, -2.500001731999736077 ) ) ;
#21291 = LINE ( 'NONE', #33864, #34347 ) ;
#21292 = ORIENTED_EDGE ( 'NONE', *, *, #35018, .F. ) ;
#21293 = DIRECTION ( 'NONE',  ( -0.000000000000000000, -0.000000000000000000, 1.000000000000000000 ) ) ;
#21294 = CARTESIAN_POINT ( 'NONE',  ( 69.39861229970156842, 58.29198505329483027, -3.933428174212718176 ) ) ;
#21295 = VECTOR ( 'NONE', #9948, 1000.000000000000000 ) ;
#21296 = ORIENTED_EDGE ( 'NONE', *, *, #27472, .F. ) ;
#21297 = CARTESIAN_POINT ( 'NONE',  ( 87.88829317789571860, -2.466143857431153830, 1.215092630805642671 ) ) ;
#21298 = PLANE ( 'NONE',  #22641 ) ;
#21299 = CARTESIAN_POINT ( 'NONE',  ( 69.99634961962405555, 58.48381665884328839, 3.916752429509930078 ) ) ;
#21300 = CARTESIAN_POINT ( 'NONE',  ( -2.878675913592191993, -26.64985754041175525, 6.800000000000000711 ) ) ;
#21301 = CARTESIAN_POINT ( 'NONE',  ( -1.419396944644200298, -28.21829086823094102, 6.988553391373221402 ) ) ;
#21303 = CARTESIAN_POINT ( 'NONE',  ( 1.317243270070298511, -26.19158756650236342, 6.969307238440505259 ) ) ;
#21302 = CARTESIAN_POINT ( 'NONE',  ( -34.87867591359218977, -24.55319635012989110, 6.700000000000000178 ) ) ;
#21304 = CARTESIAN_POINT ( 'NONE',  ( 2.170460981197068762, -32.93727830324805694, 7.754798119455333705 ) ) ;
#21305 = ORIENTED_EDGE ( 'NONE', *, *, #4609, .F. ) ;
#21306 = CARTESIAN_POINT ( 'NONE',  ( 24.76343259005120601, 3.021619590193751925, 3.339778374755230317 ) ) ;
#21307 = EDGE_CURVE ( 'NONE', #32308, #16760, #11715, .T. ) ;
#21308 = DIRECTION ( 'NONE',  ( -1.000000000000000000, 0.000000000000000000, 0.000000000000000000 ) ) ;
#21309 = CIRCLE ( 'NONE', #29209, 5.000000000000000888 ) ;
#21310 = EDGE_CURVE ( 'NONE', #12509, #14835, #14629, .T. ) ;
#21311 = VECTOR ( 'NONE', #1764, 1000.000000000000227 ) ;
#21312 = VERTEX_POINT ( 'NONE', #20453 ) ;
#21313 = CARTESIAN_POINT ( 'NONE',  ( 79.74939209361063774, 63.58699539661090228, -3.734652355492745102 ) ) ;
#21314 = CARTESIAN_POINT ( 'NONE',  ( -12.44874870218064267, -26.64985754041175525, 6.700000000000000178 ) ) ;
#21315 = CARTESIAN_POINT ( 'NONE',  ( 81.46256558106179568, 64.48035972931448612, -3.017922835037758933 ) ) ;
#21316 = CARTESIAN_POINT ( 'NONE',  ( 80.79830692519234958, 61.67796721187822584, 2.640205493567646222 ) ) ;
#21317 = CARTESIAN_POINT ( 'NONE',  ( 22.36801796201435977, 4.217314093436514533, 3.697468194167767841 ) ) ;
#21319 = VERTEX_POINT ( 'NONE', #33031 ) ;
#21318 = CARTESIAN_POINT ( 'NONE',  ( -1.389564992689783951, -31.21326896663422090, 7.754798119455333705 ) ) ;
#21320 = CARTESIAN_POINT ( 'NONE',  ( 21.85643539959772497, -11.05315871940826078, 3.104450560420165317 ) ) ;
#21321 = ORIENTED_EDGE ( 'NONE', *, *, #5799, .T. ) ;
#21322 = CARTESIAN_POINT ( 'NONE',  ( -79.46431696083011786, 10.38012969939556740, 7.168986771804887859 ) ) ;
#21323 = CARTESIAN_POINT ( 'NONE',  ( 36.19706241022630877, -3.644680151509849253, 5.718849134531836853 ) ) ;
#21324 = CARTESIAN_POINT ( 'NONE',  ( 5.039926880157825195, -30.20828278875847062, 6.894806418505346812 ) ) ;
#21325 = AXIS2_PLACEMENT_3D ( 'NONE', #32121, #4115, #29210 ) ;
#21326 = CARTESIAN_POINT ( 'NONE',  ( -73.53200420073510202, 5.707097961328267743, -10.87087679806554341 ) ) ;
#21327 = DIRECTION ( 'NONE',  ( 0.000000000000000000, -0.000000000000000000, -1.000000000000000000 ) ) ;
#21328 = CARTESIAN_POINT ( 'NONE',  ( 36.88849515942500545, -3.352853972477296995, -5.910143701334799715 ) ) ;
#21329 = B_SPLINE_CURVE_WITH_KNOTS ( 'NONE', 3,
 ( #9182, #11849, #17614, #27104, #30827, #12050, #5904, #36777, #8560, #31030 ),
 .UNSPECIFIED., .F., .F.,
 ( 4, 2, 2, 2, 4 ),
 ( 0.001566336636202482176, 0.001957536639217857637, 0.002348736642233233314, 0.002739936645248608992, 0.003131136648263984669 ),
 .UNSPECIFIED. ) ;
#21330 = CARTESIAN_POINT ( 'NONE',  ( -10.24874870218063450, -26.64985754041175525, 6.700000000000000178 ) ) ;
#21331 = CARTESIAN_POINT ( 'NONE',  ( 15.16924916808596357, 11.40858824471275312, 2.573926220994043224 ) ) ;
#21332 = LINE ( 'NONE', #25239, #33108 ) ;
#21333 = CARTESIAN_POINT ( 'NONE',  ( 29.36363007681232418, -3.858821234667521249, 4.337399626228677363 ) ) ;
#21334 = DIRECTION ( 'NONE',  ( -0.7660444431189761261, -0.6427876096865416944, 0.000000000000000000 ) ) ;
#21335 = CIRCLE ( 'NONE', #3611, 2.500000000000002220 ) ;
#21336 = CARTESIAN_POINT ( 'NONE',  ( 17.32389278323182680, 14.30653710295208647, -2.500000000000000000 ) ) ;
#21337 = CARTESIAN_POINT ( 'NONE',  ( 1.128064129311358244, -33.02281926226938680, 7.695279973900954751 ) ) ;
#21338 = CARTESIAN_POINT ( 'NONE',  ( 24.53892863518501599, 2.743979168526681445, -3.872037506538268392 ) ) ;
#21339 = ORIENTED_EDGE ( 'NONE', *, *, #2109, .F. ) ;
#21340 = CARTESIAN_POINT ( 'NONE',  ( 67.19584252064707641, 57.93747020029492489, 3.996350724342223604 ) ) ;
#21341 = CARTESIAN_POINT ( 'NONE',  ( 33.68675182762641640, -1.062721320211014175, 5.464030358509579521 ) ) ;
#21342 = CARTESIAN_POINT ( 'NONE',  ( 0.6783104270758654186, -48.60743831809499227, 6.000000000000000000 ) ) ;
#21343 = LINE ( 'NONE', #33917, #18764 ) ;
#21344 = CARTESIAN_POINT ( 'NONE',  ( 88.25293897076788596, -0.9571425830051931705, -4.167473131139645126 ) ) ;
#21345 = CARTESIAN_POINT ( 'NONE',  ( 31.28447350889217304, -0.4025536940246822737, -5.089096727550352917 ) ) ;
#21346 = B_SPLINE_CURVE_WITH_KNOTS ( 'NONE', 3,
 ( #30562, #37333, #21290, #27659, #15306, #14681, #17975, #34284, #15099, #2372, #21500, #24368, #34077, #11587, #33463, #2993, #40620, #14890 ),
 .UNSPECIFIED., .F., .F.,
 ( 4, 2, 2, 2, 2, 2, 2, 2, 4 ),
 ( 0.000000000000000000, 2.302533481709740794E-05, 4.605066963419481588E-05, 9.210133926839220674E-05, 0.0001842026785367869614, 0.0003684053570735786390, 0.0005526080356103703437, 0.0006447093748787674971, 0.0007368107141471646505 ),
 .UNSPECIFIED. ) ;
#21347 = ORIENTED_EDGE ( 'NONE', *, *, #35482, .F. ) ;
#21348 = CARTESIAN_POINT ( 'NONE',  ( -16.34874870218063592, -26.64985754041175525, 6.700000000000000178 ) ) ;
#21349 = CARTESIAN_POINT ( 'NONE',  ( -69.95454086882011779, -21.04534624052442382, 5.920661432671354696 ) ) ;
#21350 = ORIENTED_EDGE ( 'NONE', *, *, #4092, .F. ) ;
#21351 = CARTESIAN_POINT ( 'NONE',  ( -69.92837670882107659, -20.78299143688747819, 3.916079783099620126 ) ) ;
#21352 = VECTOR ( 'NONE', #33855, 1000.000000000000000 ) ;
#21353 = UNCERTAINTY_MEASURE_WITH_UNIT (LENGTH_MEASURE( 1.000000000000000082E-05 ), #19275, 'distance_accuracy_value', 'NONE');
#21354 = AXIS2_PLACEMENT_3D ( 'NONE', #18898, #3288, #32284 ) ;
#21355 = EDGE_CURVE ( 'NONE', #10601, #9954, #34526, .T. ) ;
#21356 = ORIENTED_EDGE ( 'NONE', *, *, #6102, .F. ) ;
#21357 = CARTESIAN_POINT ( 'NONE',  ( 79.17340063025110908, 65.28954359503943294, -3.030715982579950563 ) ) ;
#21358 = CARTESIAN_POINT ( 'NONE',  ( -1.528267587133116612, -28.21871976935260662, 6.890920332093122269 ) ) ;
#21359 = ADVANCED_FACE ( 'NONE', ( #34070 ), #21083, .T. ) ;
#21360 = CARTESIAN_POINT ( 'NONE',  ( 79.92041472187213458, 64.04075560556067614, 3.697630003121161302 ) ) ;
#21362 = ORIENTED_EDGE ( 'NONE', *, *, #33535, .F. ) ;
#21361 = CARTESIAN_POINT ( 'NONE',  ( 14.77315594796471743, 13.19392823276620419, 2.499999999999996891 ) ) ;
#21363 = CARTESIAN_POINT ( 'NONE',  ( 74.21382537490346465, 62.79450482958245772, -3.300071129360916622 ) ) ;
#21364 = CARTESIAN_POINT ( 'NONE',  ( -1.799609906766908685, -29.56993018339339940, 7.202408869016148074 ) ) ;
#21366 = FACE_OUTER_BOUND ( 'NONE', #10489, .T. ) ;
#21365 = DIRECTION ( 'NONE',  ( -0.000000000000000000, -1.000000000000000000, -0.000000000000000000 ) ) ;
#21367 = CARTESIAN_POINT ( 'NONE',  ( -63.58520484588294153, 35.72026407271188475, -6.999999999999999112 ) ) ;
#21368 = CARTESIAN_POINT ( 'NONE',  ( 24.33330849205117374, 3.134806574687862391, -3.409030949822150713 ) ) ;
#21369 = EDGE_LOOP ( 'NONE', ( #14140, #31381, #1254, #7408 ) ) ;
#21370 = CARTESIAN_POINT ( 'NONE',  ( 24.76528640762570888, -1.939968142380837701, -6.533370004292007316 ) ) ;
#21371 = CARTESIAN_POINT ( 'NONE',  ( 2.896981936218417264, -32.75240845689362601, 7.695279973900954751 ) ) ;
#21372 = CARTESIAN_POINT ( 'NONE',  ( 1.700390093233090871, -29.56993018339339940, -2.499999999999998668 ) ) ;
#21373 = CARTESIAN_POINT ( 'NONE',  ( 81.51347805233932320, 61.90211215308875836, 2.263370276488428257 ) ) ;
#21374 = CARTESIAN_POINT ( 'NONE',  ( 84.24490603200722205, 3.007448030680667017, 1.128815683486722454 ) ) ;
#21375 = CYLINDRICAL_SURFACE ( 'NONE', #12824, 0.1000000000000028644 ) ;
#21376 = ORIENTED_EDGE ( 'NONE', *, *, #32592, .F. ) ;
#21377 = DIRECTION ( 'NONE',  ( 0.000000000000000000, 0.000000000000000000, 1.000000000000000000 ) ) ;
#21378 = CARTESIAN_POINT ( 'NONE',  ( 3.533038598990357215, -26.70610496455467953, 6.871394612369934762 ) ) ;
#21379 = ADVANCED_FACE ( 'NONE', ( #5430 ), #27853, .T. ) ;
#21380 = VERTEX_POINT ( 'NONE', #30350 ) ;
#21381 = AXIS2_PLACEMENT_3D ( 'NONE', #27551, #40108, #30868 ) ;
#21382 = VECTOR ( 'NONE', #24855, 1000.000000000000000 ) ;
#21383 = DIRECTION ( 'NONE',  ( -0.000000000000000000, -1.000000000000000000, -0.000000000000000000 ) ) ;
#21384 = CARTESIAN_POINT ( 'NONE',  ( 33.11740971841622638, -3.526206640162208750, -5.310590497510783159 ) ) ;
#21385 = CARTESIAN_POINT ( 'NONE',  ( -68.71186372058383540, 37.81212149306785619, -9.800414904976365804 ) ) ;
#21386 = LINE ( 'NONE', #33962, #26003 ) ;
#21387 = CIRCLE ( 'NONE', #3663, 0.1000000000000028644 ) ;
#21388 = CARTESIAN_POINT ( 'NONE',  ( 1.845837775478998077, -26.17304264157967708, 6.868387053540520704 ) ) ;
#21389 = ORIENTED_EDGE ( 'NONE', *, *, #6381, .F. ) ;
#21390 = CARTESIAN_POINT ( 'NONE',  ( 2.877452244276258231, -32.85680554558438615, 7.778495531946297170 ) ) ;
#21391 = EDGE_CURVE ( 'NONE', #28028, #20325, #35821, .T. ) ;
#21392 = CARTESIAN_POINT ( 'NONE',  ( 86.50262394474026451, 1.193871719766480100, -4.934721793127618383 ) ) ;
#21393 = ORIENTED_EDGE ( 'NONE', *, *, #31254, .T. ) ;
#21394 = VERTEX_POINT ( 'NONE', #12209 ) ;
#21396 = CARTESIAN_POINT ( 'NONE',  ( 36.44620324436766623, -1.730678941397710169, 5.729688724127439237 ) ) ;
#21395 = CARTESIAN_POINT ( 'NONE',  ( 79.79486853628222320, 65.42109455898982162, -3.057227112800017910 ) ) ;
#21397 =( BOUNDED_CURVE ( )  B_SPLINE_CURVE ( 3, ( #15408, #12938, #24896, #34993 ),
 .UNSPECIFIED., .F., .F. ) 
 B_SPLINE_CURVE_WITH_KNOTS ( ( 4, 4 ),
 ( 1.381924640371167357, 1.574767692156076038 ),
 .UNSPECIFIED. ) 
 CURVE ( )  GEOMETRIC_REPRESENTATION_ITEM ( )  RATIONAL_B_SPLINE_CURVE ( ( 1.000000000000000000, 0.9969033633783032089, 0.9969033633783032089, 1.000000000000000000 ) ) 
 REPRESENTATION_ITEM ( '' )  );
#21398 = CARTESIAN_POINT ( 'NONE',  ( 26.12357031956679876, -2.759746946588834682, 4.283612967940825911 ) ) ;
#21399 = CARTESIAN_POINT ( 'NONE',  ( 3.463872813216964275, -32.59319547873680989, 7.638132480492515697 ) ) ;
#21400 = CARTESIAN_POINT ( 'NONE',  ( -75.45330471031414277, 33.71485196875532608, -46.17089178453873188 ) ) ;
#21401 = EDGE_LOOP ( 'NONE', ( #29936, #22358, #34753, #11756 ) ) ;
#21402 = DIRECTION ( 'NONE',  ( 0.000000000000000000, 0.000000000000000000, 1.000000000000000000 ) ) ;
#21403 = ORIENTED_EDGE ( 'NONE', *, *, #34802, .F. ) ;
#21404 = VERTEX_POINT ( 'NONE', #8704 ) ;
#21405 = LINE ( 'NONE', #19074, #9538 ) ;
#21406 = EDGE_CURVE ( 'NONE', #13175, #17512, #33860, .T. ) ;
#21407 = EDGE_CURVE ( 'NONE', #28306, #11301, #36717, .T. ) ;
#21408 = CARTESIAN_POINT ( 'NONE',  ( 81.11951992695615843, 61.28566998660698317, -1.215327096190472966 ) ) ;
#21409 = CARTESIAN_POINT ( 'NONE',  ( -59.00289461565213855, 28.67396232720155780, -6.820567581290490899 ) ) ;
#21411 = CARTESIAN_POINT ( 'NONE',  ( 31.22136964576698404, 0.5681969411430533023, 4.564728438945290456 ) ) ;
#21410 = CARTESIAN_POINT ( 'NONE',  ( 23.67960553047068473, 2.561144650517011456, 4.199896394371767094 ) ) ;
#21412 = VERTEX_POINT ( 'NONE', #17763 ) ;
#21413 = CARTESIAN_POINT ( 'NONE',  ( 82.26467961622988412, 63.75423115438291433, -2.259066313178065499 ) ) ;
#21414 = VECTOR ( 'NONE', #6476, 1000.000000000000000 ) ;
#21415 = CARTESIAN_POINT ( 'NONE',  ( -58.99872204295123623, 28.48507918597134037, -12.49999999999999645 ) ) ;
#21416 = ORIENTED_EDGE ( 'NONE', *, *, #16119, .T. ) ;
#21418 = CARTESIAN_POINT ( 'NONE',  ( 85.15434555589628474, 2.708321999268741731, -0.5844145583951695366 ) ) ;
#21417 = DIRECTION ( 'NONE',  ( 0.000000000000000000, 0.000000000000000000, 1.000000000000000000 ) ) ;
#21419 = CARTESIAN_POINT ( 'NONE',  ( -1.796981532764649003, -29.43400205062587816, 6.870724624169667116 ) ) ;
#21420 = CARTESIAN_POINT ( 'NONE',  ( 72.85835069609119330, 61.31913755009141909, 3.785151435630688788 ) ) ;
#21421 = CARTESIAN_POINT ( 'NONE',  ( 23.74549009334706540, 2.920879532582420168, -3.920752113660479932 ) ) ;
#21422 = EDGE_LOOP ( 'NONE', ( #33871, #33991, #2600, #34480 ) ) ;
#21423 = AXIS2_PLACEMENT_3D ( 'NONE', #7457, #16123, #28688 ) ;
#21424 = EDGE_CURVE ( 'NONE', #37652, #33400, #20867, .T. ) ;
#21425 = CARTESIAN_POINT ( 'NONE',  ( 21.85643539959774273, -11.65679437655345474, 11.20963770477306554 ) ) ;
#21426 = B_SPLINE_CURVE_WITH_KNOTS ( 'NONE', 3,
 ( #9102, #18364, #2755, #25984, #10517, #19194, #3573, #32177, #10712, #674, #29272, #38516, #13213, #16299, #25779, #16494, #7432, #38119, #22896 ),
 .UNSPECIFIED., .F., .F.,
 ( 4, 3, 3, 3, 3, 3, 4 ),
 ( 0.000000000000000000, 2.546128104244783745E-05, 5.711050680484153604E-05, 8.113074941675923069E-05, 0.0001053129305727060346, 0.0001360598016347114444, 0.0001612931755702003752 ),
 .UNSPECIFIED. ) ;
#21427 = CARTESIAN_POINT ( 'NONE',  ( 0.9213240864078056092, -24.55319635012989110, 6.800000000000000711 ) ) ;
#21428 = EDGE_LOOP ( 'NONE', ( #17465, #2021, #34795, #22311 ) ) ;
#21429 = CARTESIAN_POINT ( 'NONE',  ( 3.896194328649233984, -32.16578144256224903, 7.635761828346577573 ) ) ;
#21430 = CARTESIAN_POINT ( 'NONE',  ( 81.46256558106202306, 64.48035972931458559, 3.017922835037552876 ) ) ;
#21431 = CARTESIAN_POINT ( 'NONE',  ( 88.21591849536395102, -0.7305820373589052563, 3.481732356799086769 ) ) ;
#21432 = DIRECTION ( 'NONE',  ( -1.000000000000000000, 0.000000000000000000, 0.000000000000000000 ) ) ;
#21433 = DIRECTION ( 'NONE',  ( -1.000000000000000000, 0.000000000000000000, 0.000000000000000000 ) ) ;
#21434 = CARTESIAN_POINT ( 'NONE',  ( 31.37751630285753990, -3.642699559265466291, 4.877213502604051953 ) ) ;
#21435 = CARTESIAN_POINT ( 'NONE',  ( -28.34874870218063947, -26.64985754041175525, 6.700000000000000178 ) ) ;
#21436 = CARTESIAN_POINT ( 'NONE',  ( 32.78155291855927089, -0.9262908896100177092, -5.322752176431207793 ) ) ;
#21437 = CARTESIAN_POINT ( 'NONE',  ( -1.078675913592196167, -26.64985754041175525, 6.700000000000000178 ) ) ;
#21438 = CARTESIAN_POINT ( 'NONE',  ( 5.166053052204034657, -29.08252373668924307, 7.754798119455333705 ) ) ;
#21439 = ADVANCED_FACE ( 'NONE', ( #18383 ), #1958, .F. ) ;
#21440 = EDGE_CURVE ( 'NONE', #3377, #40670, #33459, .T. ) ;
#21441 = CARTESIAN_POINT ( 'NONE',  ( -63.08758708074093136, -21.25669541281728669, -3.000000000000000000 ) ) ;
#21442 = EDGE_CURVE ( 'NONE', #12108, #25231, #2156, .T. ) ;
#21443 = LINE ( 'NONE', #15248, #19016 ) ;
#21444 = CIRCLE ( 'NONE', #37207, 3.499999999999999556 ) ;
#21445 = CARTESIAN_POINT ( 'NONE',  ( 1.952673410241816176, -32.96768074256310399, 7.505001789837626447 ) ) ;
#21446 = CIRCLE ( 'NONE', #15528, 1.000000000000000666 ) ;
#21447 = ORIENTED_EDGE ( 'NONE', *, *, #14880, .T. ) ;
#21448 = CARTESIAN_POINT ( 'NONE',  ( 34.60561289930970474, -0.8402221667057534482, 5.339566637150812589 ) ) ;
#21449 = DIRECTION ( 'NONE',  ( 0.000000000000000000, 0.000000000000000000, 1.000000000000000000 ) ) ;
#21450 = CARTESIAN_POINT ( 'NONE',  ( 66.87313677512783272, 57.91234881663538658, -3.999382933222194847 ) ) ;
#21451 = VECTOR ( 'NONE', #17909, 1000.000000000000114 ) ;
#21452 = CARTESIAN_POINT ( 'NONE',  ( 1.700390093233090871, -29.56993018339339940, 7.750000000000000888 ) ) ;
#21453 = EDGE_LOOP ( 'NONE', ( #31927, #21923, #30170, #4103, #40526, #8142, #8509, #19370 ) ) ;
#21454 = CARTESIAN_POINT ( 'NONE',  ( -71.92837670882107659, -65.19654454972992141, 5.916079783099617906 ) ) ;
#21455 = CARTESIAN_POINT ( 'NONE',  ( 5.866854291671645960, -27.23014986009699712, 7.013842709614101167 ) ) ;
#21456 = DIRECTION ( 'NONE',  ( 1.000000000000000000, 0.000000000000000000, -0.000000000000000000 ) ) ;
#21457 = ORIENTED_EDGE ( 'NONE', *, *, #33288, .T. ) ;
#21458 = CARTESIAN_POINT ( 'NONE',  ( -34.34874870218063592, -26.64985754041175525, 6.800000000000000711 ) ) ;
#21459 = LINE ( 'NONE', #34438, #12667 ) ;
#21460 = ORIENTED_EDGE ( 'NONE', *, *, #25355, .F. ) ;
#21461 = CARTESIAN_POINT ( 'NONE',  ( 22.39063959453807939, 4.900407498310523025, 3.082520428777218324 ) ) ;
#21462 = CARTESIAN_POINT ( 'NONE',  ( 79.34209122208885390, 66.30884595491197331, -1.000000000000000000 ) ) ;
#21463 = CARTESIAN_POINT ( 'NONE',  ( 80.81256737103976207, 62.69530837521176636, 3.364061116559607267 ) ) ;
#21464 = CARTESIAN_POINT ( 'NONE',  ( -0.1322584125241582920, -32.43375540223212994, 6.871394612369934762 ) ) ;
#21465 = ORIENTED_EDGE ( 'NONE', *, *, #32386, .T. ) ;
#21466 = CARTESIAN_POINT ( 'NONE',  ( 77.10371989074776877, 62.50202019409577048, -3.856837490694493997 ) ) ;
#21468 = LINE ( 'NONE', #2960, #39443 ) ;
#21467 = CARTESIAN_POINT ( 'NONE',  ( 3.859316710813556206, -32.32368945768034507, 7.761113333116784752 ) ) ;
#21469 = CARTESIAN_POINT ( 'NONE',  ( 0.5037982502477859059, -26.38745190989316214, 7.703977250142848732 ) ) ;
#21470 = CARTESIAN_POINT ( 'NONE',  ( 78.68244131272051334, 66.05295088176872298, -1.094381639753450930 ) ) ;
#21471 = CARTESIAN_POINT ( 'NONE',  ( 76.39468346684418520, 63.92226846272791363, 3.160174624570346147 ) ) ;
#21472 = ORIENTED_EDGE ( 'NONE', *, *, #17606, .F. ) ;
#21473 = ADVANCED_FACE ( 'NONE', ( #30969 ), #2775, .F. ) ;
#21474 = CARTESIAN_POINT ( 'NONE',  ( 4.747584925568015812, -31.29173262670428102, 7.670465701733750308 ) ) ;
#21475 = CARTESIAN_POINT ( 'NONE',  ( 82.26850461147290616, 62.50126132183006433, 1.564050819713521223 ) ) ;
#21478 = ORIENTED_EDGE ( 'NONE', *, *, #21548, .T. ) ;
#21477 = DIRECTION ( 'NONE',  ( 0.4999999999999999445, -0.8660254037844387076, 0.000000000000000000 ) ) ;
#21476 = CARTESIAN_POINT ( 'NONE',  ( 4.258250226677295913, -31.95893657470690741, 6.921725064902953584 ) ) ;
#21479 = CARTESIAN_POINT ( 'NONE',  ( 31.96174557538834193, -4.583587016071825282, 3.235063174744643000 ) ) ;
#21480 = FACE_OUTER_BOUND ( 'NONE', #22277, .T. ) ;
#21481 = DIRECTION ( 'NONE',  ( 1.000000000000000000, 0.000000000000000000, 0.000000000000000000 ) ) ;
#21482 = CARTESIAN_POINT ( 'NONE',  ( -64.59661209699966378, 34.69995260619790400, 6.002488439271551179 ) ) ;
#21483 = CARTESIAN_POINT ( 'NONE',  ( 23.60498067204314410, 0.4413003733997728495, -5.510345162601594460 ) ) ;
#21484 = EDGE_CURVE ( 'NONE', #21149, #2729, #33857, .T. ) ;
#21485 = AXIS2_PLACEMENT_3D ( 'NONE', #22701, #29070, #19991 ) ;
#21486 = CARTESIAN_POINT ( 'NONE',  ( -1.593127767899503722, -28.38555688987459291, 7.635761828346575797 ) ) ;
#21487 = DIRECTION ( 'NONE',  ( -0.6662082868431850047, 0.000000000000000000, -0.7457657263118683266 ) ) ;
#21488 = CARTESIAN_POINT ( 'NONE',  ( 0.5179793559627476895, -32.86415379421544714, 7.638132480492514809 ) ) ;
#21489 = ADVANCED_FACE ( 'NONE', ( #21699 ), #22672, .T. ) ;
#21490 = DIRECTION ( 'NONE',  ( 1.000000000000000000, 0.000000000000000000, 0.000000000000000000 ) ) ;
#21491 = CARTESIAN_POINT ( 'NONE',  ( 36.41841363650763697, -1.780316330609500675, -5.760878658093356641 ) ) ;
#21492 = CARTESIAN_POINT ( 'NONE',  ( 30.87873567178753831, -3.511903919675081642, -4.882802410549687444 ) ) ;
#21493 = CARTESIAN_POINT ( 'NONE',  ( 1.123288416806107026, -32.92059484209399045, 7.635761828346577573 ) ) ;
#21494 = CARTESIAN_POINT ( 'NONE',  ( -0.07210163165322443224, -26.55193716086669653, 7.737115613922529889 ) ) ;
#21495 = DIRECTION ( 'NONE',  ( -0.000000000000000000, -0.000000000000000000, -1.000000000000000000 ) ) ;
#21496 = CARTESIAN_POINT ( 'NONE',  ( -22.87867591359218977, -26.64985754041175525, 6.700000000000000178 ) ) ;
#21497 = CARTESIAN_POINT ( 'NONE',  ( 5.099125247292754182, -29.66318013251687447, 6.866852738645440546 ) ) ;
#21498 = EDGE_CURVE ( 'NONE', #142, #25139, #5228, .T. ) ;
#21499 = DIRECTION ( 'NONE',  ( 1.000000000000000000, 0.000000000000000000, 0.000000000000000000 ) ) ;
#21500 = CARTESIAN_POINT ( 'NONE',  ( 14.72811636034318639, -4.878256426182215222, -2.502161937363848843 ) ) ;
#21501 = CARTESIAN_POINT ( 'NONE',  ( 23.52668297624172666, 2.287558078930879368, -4.447727279419068758 ) ) ;
#21502 = ORIENTED_EDGE ( 'NONE', *, *, #4212, .F. ) ;
#21503 = CARTESIAN_POINT ( 'NONE',  ( 4.738207753463742122, -31.30822356001046458, 7.635761828346574021 ) ) ;
#21504 = CARTESIAN_POINT ( 'NONE',  ( 69.67664977695649497, 59.29623187989270150, -3.972683913566358083 ) ) ;
#21505 = VECTOR ( 'NONE', #8743, 1000.000000000000000 ) ;
#21506 = ORIENTED_EDGE ( 'NONE', *, *, #20472, .F. ) ;
#21507 = CARTESIAN_POINT ( 'NONE',  ( 84.50243033367722489, 2.523019330700893903, 3.504063919878146027 ) ) ;
#21508 = DIRECTION ( 'NONE',  ( 0.5000000000000101030, -0.8660254037844328234, -0.000000000000000000 ) ) ;
#21509 = CARTESIAN_POINT ( 'NONE',  ( 4.954463893073100422, -28.58453498085037836, 7.013842709614101167 ) ) ;
#21510 = CARTESIAN_POINT ( 'NONE',  ( -1.419098044220405974, -28.21759841648404432, 6.920489980334477487 ) ) ;
#21511 = AXIS2_PLACEMENT_3D ( 'NONE', #19920, #29397, #10444 ) ;
#21512 = CARTESIAN_POINT ( 'NONE',  ( 1.301684415825685726, -26.19338184037020767, 7.006423389747789443 ) ) ;
#21513 = VECTOR ( 'NONE', #1894, 1000.000000000000000 ) ;
#21514 = ITEM_DEFINED_TRANSFORMATION ( 'NONE', 'NONE', #40587,  #30744 ) ;
#21515 = VECTOR ( 'NONE', #38225, 1000.000000000000000 ) ;
#21516 = LINE ( 'NONE', #8930, #26485 ) ;
#21517 = ORIENTED_EDGE ( 'NONE', *, *, #12561, .T. ) ;
#21518 = CARTESIAN_POINT ( 'NONE',  ( 21.98762963305790308, 5.627346946651078596, 3.080487669913397841 ) ) ;
#21519 = ORIENTED_EDGE ( 'NONE', *, *, #12062, .F. ) ;
#21520 = VERTEX_POINT ( 'NONE', #28264 ) ;
#21521 = CARTESIAN_POINT ( 'NONE',  ( 79.09261123048416664, 64.22416776617160394, -3.612066323963887715 ) ) ;
#21522 = CARTESIAN_POINT ( 'NONE',  ( 15.71701945473647655, 8.042377430118643034, -3.484701709439959494 ) ) ;
#21523 = CARTESIAN_POINT ( 'NONE',  ( 80.65441534633333731, 65.56043466500595684, -2.771525467262166753 ) ) ;
#21524 = B_SPLINE_CURVE_WITH_KNOTS ( 'NONE', 3,
 ( #15659, #24937, #225, #19364 ),
 .UNSPECIFIED., .F., .F.,
 ( 4, 4 ),
 ( 0.000000000000000000, 6.391136169993434029E-06 ),
 .UNSPECIFIED. ) ;
#21525 = CARTESIAN_POINT ( 'NONE',  ( 79.01107290893718016, 64.84207397985339583, 3.331801170923393673 ) ) ;
#21526 = ORIENTED_EDGE ( 'NONE', *, *, #6333, .T. ) ;
#21527 = CARTESIAN_POINT ( 'NONE',  ( 4.389962996808223217, -27.48995486600581728, 6.865312560952602006 ) ) ;
#21528 = CARTESIAN_POINT ( 'NONE',  ( 2.895778614782184679, -32.75286161408205743, 7.712764235869103757 ) ) ;
#21529 = CARTESIAN_POINT ( 'NONE',  ( 21.85643539959774273, -6.858222381794880640, 10.60035608423801357 ) ) ;
#21530 = ORIENTED_EDGE ( 'NONE', *, *, #168, .F. ) ;
#21531 = CARTESIAN_POINT ( 'NONE',  ( -74.90361456537704044, 9.559336010372646797, 9.177345781745600561 ) ) ;
#21532 = LINE ( 'NONE', #37161, #37798 ) ;
#21533 = CARTESIAN_POINT ( 'NONE',  ( -1.312560436656866392, -31.35097737660188244, 7.695279973900954751 ) ) ;
#21534 = AXIS2_PLACEMENT_3D ( 'NONE', #6135, #12505, #37610 ) ;
#21535 = FACE_OUTER_BOUND ( 'NONE', #10093, .T. ) ;
#21536 = CARTESIAN_POINT ( 'NONE',  ( 3.465471057152984091, -32.59226193070500699, 7.750000000000000000 ) ) ;
#21537 = CARTESIAN_POINT ( 'NONE',  ( 35.36814664345466497, -3.792965548836813028, -5.510366441342056554 ) ) ;
#21538 = CARTESIAN_POINT ( 'NONE',  ( -1.758218327909825129, -30.07531940574666507, 7.771081512783698741 ) ) ;
#21539 = DIRECTION ( 'NONE',  ( 0.000000000000000000, 0.000000000000000000, -1.000000000000000000 ) ) ;
#21540 = FACE_OUTER_BOUND ( 'NONE', #18748, .T. ) ;
#21541 = CARTESIAN_POINT ( 'NONE',  ( -21.07867591359219617, -24.55319635012989110, 6.800000000000000711 ) ) ;
#21542 = AXIS2_PLACEMENT_3D ( 'NONE', #33647, #9311, #24562 ) ;
#21543 = CIRCLE ( 'NONE', #17565, 10.00000000000000888 ) ;
#21544 = EDGE_CURVE ( 'NONE', #30375, #320, #28885, .T. ) ;
#21545 = ADVANCED_FACE ( 'NONE', ( #37930 ), #3790, .F. ) ;
#21546 = DIRECTION ( 'NONE',  ( 1.000000000000000000, 0.000000000000000000, 0.000000000000000000 ) ) ;
#21547 = CARTESIAN_POINT ( 'NONE',  ( 30.98497569240768001, -3.765466457291608116, -4.599884699063723659 ) ) ;
#21548 = EDGE_CURVE ( 'NONE', #19820, #24741, #32321, .T. ) ;
#21549 = CARTESIAN_POINT ( 'NONE',  ( 25.67913400440570015, 2.136453941815092961, -4.141921070930310478 ) ) ;
#21550 = ORIENTED_EDGE ( 'NONE', *, *, #21613, .F. ) ;
#21551 = CARTESIAN_POINT ( 'NONE',  ( 67.17808119270118539, 57.98628055940345405, 3.998197261021421589 ) ) ;
#21552 = CARTESIAN_POINT ( 'NONE',  ( 36.82698429609488500, -3.168745687177260351, 5.951708789409448919 ) ) ;
#21553 = CARTESIAN_POINT ( 'NONE',  ( 4.948327458862285866, -30.86155448860804285, 7.771081512783703182 ) ) ;
#21554 = FACE_OUTER_BOUND ( 'NONE', #10674, .T. ) ;
#21555 = CARTESIAN_POINT ( 'NONE',  ( 87.30391260081773908, -0.2898811470106905652, 5.673122884556256906 ) ) ;
#21557 = CARTESIAN_POINT ( 'NONE',  ( 33.93672751689359757, -1.338894892125421565, -5.503045110504557691 ) ) ;
#21556 = CARTESIAN_POINT ( 'NONE',  ( 29.97939791730999914, 0.4010955892747467555, 5.210136963171234648 ) ) ;
#21558 = DIRECTION ( 'NONE',  ( -0.000000000000000000, -0.000000000000000000, 1.000000000000000000 ) ) ;
#21559 = CARTESIAN_POINT ( 'NONE',  ( -1.551921384529348691, -30.56115925902171071, 6.887945620086122211 ) ) ;
#21560 = B_SPLINE_CURVE_WITH_KNOTS ( 'NONE', 5,
 ( #36781, #8564, #39869, #20931, #30627, #5288, #17825, #2433 ),
 .UNSPECIFIED., .F., .F.,
 ( 6, 2, 6 ),
 ( 0.000000000000000000, 0.5000000000000000000, 1.000000000000000000 ),
 .UNSPECIFIED. ) ;
#21561 = VERTEX_POINT ( 'NONE', #24989 ) ;
#21562 = CARTESIAN_POINT ( 'NONE',  ( 24.67496769583028993, 2.993954329345769771, 3.481334102667019259 ) ) ;
#21563 = DIRECTION ( 'NONE',  ( -0.000000000000000000, -0.000000000000000000, 1.000000000000000000 ) ) ;
#21564 = ORIENTED_EDGE ( 'NONE', *, *, #18724, .T. ) ;
#21565 = CARTESIAN_POINT ( 'NONE',  ( -70.22814611767556414, -21.49690818219047017, 5.971043812772915516 ) ) ;
#21566 = ORIENTED_EDGE ( 'NONE', *, *, #7909, .T. ) ;
#21567 = CARTESIAN_POINT ( 'NONE',  ( 80.97211960314545820, 61.55694294823970836, -2.294512580621450137 ) ) ;
#21568 = CARTESIAN_POINT ( 'NONE',  ( 24.75839165839662925, 3.019244830385916956, -3.350409272483306111 ) ) ;
#21569 = AXIS2_PLACEMENT_3D ( 'NONE', #33135, #1853, #38889 ) ;
#21570 = CARTESIAN_POINT ( 'NONE',  ( 80.93309715666640614, 61.70751139687529729, 2.576318598473983368 ) ) ;
#21572 = ORIENTED_EDGE ( 'NONE', *, *, #33298, .F. ) ;
#21571 = CARTESIAN_POINT ( 'NONE',  ( -1.343423704725136059, -31.08492112836934496, 6.959317978105162616 ) ) ;
#21573 = CARTESIAN_POINT ( 'NONE',  ( 74.14280505202560789, 59.94172787350157705, -3.795548882712136418 ) ) ;
#21574 = CARTESIAN_POINT ( 'NONE',  ( -59.00071946683020485, 28.09513742959886784, 6.356270780544043930 ) ) ;
#21575 = LINE ( 'NONE', #30640, #26531 ) ;
#21576 = DIRECTION ( 'NONE',  ( 0.7394003126383932312, 0.1303762246624257659, 0.6605219282605379050 ) ) ;
#21577 = CARTESIAN_POINT ( 'NONE',  ( -54.85202521353782856, 31.46638146376523792, 1.118005318203281417 ) ) ;
#21578 = CARTESIAN_POINT ( 'NONE',  ( 23.42649477596276952, 3.757704045721736996, -3.184095338007110421 ) ) ;
#21579 = ORIENTED_EDGE ( 'NONE', *, *, #27918, .T. ) ;
#21580 = CARTESIAN_POINT ( 'NONE',  ( -34.87867591359218977, -26.64985754041175525, 6.800000000000000711 ) ) ;
#21581 = CARTESIAN_POINT ( 'NONE',  ( 24.43246502961036626, -0.4583524411608039251, -6.968550363799582925 ) ) ;
#21582 = CARTESIAN_POINT ( 'NONE',  ( -79.49313711070512056, -5.542708507839796184, -7.172005795361188873 ) ) ;
#21583 = CARTESIAN_POINT ( 'NONE',  ( 5.005772579430486147, -30.36645195696452149, 6.949473656533219135 ) ) ;
#21584 = CARTESIAN_POINT ( 'NONE',  ( 81.40003982928760706, 62.35377290961283592, 2.797238656122803757 ) ) ;
#21585 = CARTESIAN_POINT ( 'NONE',  ( 87.67494654488285732, -1.518266458920173312, 4.408571129606221994 ) ) ;
#21586 = DIRECTION ( 'NONE',  ( 0.000000000000000000, 1.000000000000000000, 0.000000000000000000 ) ) ;
#21587 = ORIENTED_EDGE ( 'NONE', *, *, #10120, .T. ) ;
#21588 = CARTESIAN_POINT ( 'NONE',  ( 2.884763386751913572, -26.27641232226080703, 7.635761828346579350 ) ) ;
#21589 = CARTESIAN_POINT ( 'NONE',  ( 4.609042127190076776, -31.33056771902256088, 7.784476445165074310 ) ) ;
#21590 = DIRECTION ( 'NONE',  ( 0.000000000000000000, 1.000000000000000000, 0.000000000000000000 ) ) ;
#21591 = CARTESIAN_POINT ( 'NONE',  ( 18.25124071569355877, -3.122163946110289245, -3.009088641841451306 ) ) ;
#21592 = ADVANCED_FACE ( 'NONE', ( #21896 ), #34474, .F. ) ;
#21593 = CARTESIAN_POINT ( 'NONE',  ( 20.42172546146963796, 3.659902873894464115, -3.393702178195764585 ) ) ;
#21594 = LINE ( 'NONE', #5942, #18066 ) ;
#21595 = CYLINDRICAL_SURFACE ( 'NONE', #11652, 0.1000000000000028644 ) ;
#21596 = ORIENTED_EDGE ( 'NONE', *, *, #22115, .T. ) ;
#21597 = CARTESIAN_POINT ( 'NONE',  ( 34.92873844507915493, -1.712022664174882358, 5.657872407722902786 ) ) ;
#21598 = VECTOR ( 'NONE', #14517, 1000.000000000000000 ) ;
#21599 = CARTESIAN_POINT ( 'NONE',  ( 85.18642856628412119, 2.672284839249654542, -1.189885989438959069 ) ) ;
#21600 = ORIENTED_EDGE ( 'NONE', *, *, #5683, .F. ) ;
#21602 = DIRECTION ( 'NONE',  ( 1.000000000000000000, 0.000000000000000000, 0.000000000000000000 ) ) ;
#21601 = CARTESIAN_POINT ( 'NONE',  ( 79.24523542244192242, 65.91691524828223692, -2.349509806045104732 ) ) ;
#21603 = APPLICATION_CONTEXT ( 'automotive_design' ) ;
#21604 = CARTESIAN_POINT ( 'NONE',  ( 16.51093427324735430, -3.201950870117511450, 2.783328630431367579 ) ) ;
#21605 = CARTESIAN_POINT ( 'NONE',  ( 3.462070670749302970, -32.59424523688933562, 7.635761828346575797 ) ) ;
#21606 = ORIENTED_EDGE ( 'NONE', *, *, #31317, .F. ) ;
#21607 = CARTESIAN_POINT ( 'NONE',  ( 28.66920249112477848, -4.024975064351027143, -4.110187144531254333 ) ) ;
#21608 = VERTEX_POINT ( 'NONE', #492 ) ;
#21609 = ORIENTED_EDGE ( 'NONE', *, *, #37330, .F. ) ;
#21610 = CARTESIAN_POINT ( 'NONE',  ( 81.18585152890854317, 61.61024096112966220, -2.156541836018578628 ) ) ;
#21611 = CARTESIAN_POINT ( 'NONE',  ( -58.56173084424084863, 30.28994157939056819, -5.156891857687778469 ) ) ;
#21612 = ORIENTED_EDGE ( 'NONE', *, *, #40218, .T. ) ;
#21613 = EDGE_CURVE ( 'NONE', #19192, #27494, #28411, .T. ) ;
#21615 = CARTESIAN_POINT ( 'NONE',  ( 35.16676341537907291, -1.025548178550078626, 5.403050771363623994 ) ) ;
#21614 = CARTESIAN_POINT ( 'NONE',  ( 23.93610855655161274, 2.571716072343740667, 4.117792848012141960 ) ) ;
#21616 = VERTEX_POINT ( 'NONE', #19412 ) ;
#21617 = CARTESIAN_POINT ( 'NONE',  ( 81.00802433895691479, 65.38516391083560109, -2.726953404243311230 ) ) ;
#21618 = LINE ( 'NONE', #2084, #23916 ) ;
#21619 = ORIENTED_EDGE ( 'NONE', *, *, #36300, .T. ) ;
#21621 = DIRECTION ( 'NONE',  ( -1.000000000000000000, -1.273455763949465810E-16, 0.000000000000000000 ) ) ;
#21620 = FACE_OUTER_BOUND ( 'NONE', #30160, .T. ) ;
#21622 = CARTESIAN_POINT ( 'NONE',  ( 8.290806648384990041, -25.50263309590217276, -6.000000000000001776 ) ) ;
#21623 = CARTESIAN_POINT ( 'NONE',  ( 0.5644051061537491698, -26.27513991809672333, 7.785593909369612931 ) ) ;
#21624 = CARTESIAN_POINT ( 'NONE',  ( 74.74317362787380148, 60.13816936446348649, 3.762445401688810698 ) ) ;
#21625 = CARTESIAN_POINT ( 'NONE',  ( 24.42172553482546959, 2.823060965057244243, -3.827932450290554733 ) ) ;
#21626 = ORIENTED_EDGE ( 'NONE', *, *, #8014, .F. ) ;
#21627 = EDGE_CURVE ( 'NONE', #9954, #1114, #13423, .T. ) ;
#21628 = CARTESIAN_POINT ( 'NONE',  ( 21.85643539959777470, -5.354795180264900978, -13.61019886989645933 ) ) ;
#21629 = CARTESIAN_POINT ( 'NONE',  ( -57.31082258017699615, 33.19667476323267152, -3.999999999999999112 ) ) ;
#21630 = EDGE_LOOP ( 'NONE', ( #24898, #34345, #24673, #20980 ) ) ;
#21631 = CARTESIAN_POINT ( 'NONE',  ( -54.83720514956231540, 31.47881213581769089, -1.097840624867143733 ) ) ;
#21632 = CARTESIAN_POINT ( 'NONE',  ( 78.87111998578922112, 66.14166623576274162, 1.344573736155044053 ) ) ;
#21633 = CARTESIAN_POINT ( 'NONE',  ( 86.85660104221420852, 0.7962678431171816840, 5.176869783008884340 ) ) ;
#21634 = B_SPLINE_CURVE_WITH_KNOTS ( 'NONE', 3,
 ( #34170, #31060, #9625, #5936, #18475, #15394, #37820, #27950, #40493, #12304, #24878, #37416, #34370, #6140 ),
 .UNSPECIFIED., .F., .F.,
 ( 4, 2, 2, 2, 2, 2, 4 ),
 ( 4.336808689942017255E-19, 0.0008516721041744092658, 0.001703344208348818098, 0.002129180260436026959, 0.002555016312523236688, 0.002980852364610445983, 0.003406688416697655278 ),
 .UNSPECIFIED. ) ;
#21635 = EDGE_LOOP ( 'NONE', ( #29269, #6517 ) ) ;
#21636 = CARTESIAN_POINT ( 'NONE',  ( 29.20850709934801159, 2.242166301403143880, -0.5075834600922535245 ) ) ;
#21637 = FACE_OUTER_BOUND ( 'NONE', #21187, .T. ) ;
#21638 = CARTESIAN_POINT ( 'NONE',  ( 17.13439990770066856, -3.171075681061939822, 2.872495620988768206 ) ) ;
#21639 = LINE ( 'NONE', #11936, #1950 ) ;
#21640 = EDGE_CURVE ( 'NONE', #34783, #29061, #12769, .T. ) ;
#21641 = CARTESIAN_POINT ( 'NONE',  ( 33.46229367853198511, -3.089018271621291500, -5.428998235802485972 ) ) ;
#21642 = CARTESIAN_POINT ( 'NONE',  ( 5.100388886341633565, -29.57279494524226138, 7.769368695748485543 ) ) ;
#21643 = CARTESIAN_POINT ( 'NONE',  ( -0.000000000000000000, 13.37661300689600097, -6.000000000000000000 ) ) ;
#21644 =( BOUNDED_CURVE ( )  B_SPLINE_CURVE ( 3, ( #14314, #11014, #11823, #26690 ),
 .UNSPECIFIED., .F., .F. ) 
 B_SPLINE_CURVE_WITH_KNOTS ( ( 4, 4 ),
 ( 4.748221474220558846, 4.941946782021393147 ),
 .UNSPECIFIED. ) 
 CURVE ( )  GEOMETRIC_REPRESENTATION_ITEM ( )  RATIONAL_B_SPLINE_CURVE ( ( 1.000000000000000000, 0.9968749865767494445, 0.9968749865767494445, 1.000000000000000000 ) ) 
 REPRESENTATION_ITEM ( '' )  );
#21645 = DIRECTION ( 'NONE',  ( 0.000000000000000000, 0.000000000000000000, 1.000000000000000000 ) ) ;
#21646 = DIRECTION ( 'NONE',  ( 0.000000000000000000, -0.000000000000000000, -1.000000000000000000 ) ) ;
#21647 = CARTESIAN_POINT ( 'NONE',  ( -70.92837670882107659, -45.61702805680359063, 6.000000000000002665 ) ) ;
#21648 = ORIENTED_EDGE ( 'NONE', *, *, #32563, .T. ) ;
#21649 = ORIENTED_EDGE ( 'NONE', *, *, #24250, .T. ) ;
#21650 = CARTESIAN_POINT ( 'NONE',  ( 36.48451820331894169, -3.515659605614979810, 5.817203863836646782 ) ) ;
#21651 = CARTESIAN_POINT ( 'NONE',  ( -71.77605803285275954, -0.2407680685837292611, 5.952073100432620834 ) ) ;
#21652 = ORIENTED_EDGE ( 'NONE', *, *, #7219, .F. ) ;
#21653 = CARTESIAN_POINT ( 'NONE',  ( 66.86527468745164526, 57.93417386730686758, -3.999594749379963066 ) ) ;
#21654 = CARTESIAN_POINT ( 'NONE',  ( -71.90229890510927646, -0.5209448599347925590, 9.952588678376171671 ) ) ;
#21655 = CIRCLE ( 'NONE', #3932, 0.1000000000000028644 ) ;
#21656 = EDGE_CURVE ( 'NONE', #23269, #25596, #25279, .T. ) ;
#21657 = VERTEX_POINT ( 'NONE', #32790 ) ;
#21658 = CARTESIAN_POINT ( 'NONE',  ( 88.37073220026057641, -0.9044761386004964709, -0.07382722449155432187 ) ) ;
#21659 = LINE ( 'NONE', #34237, #18671 ) ;
#21660 = CARTESIAN_POINT ( 'NONE',  ( -71.19089206238980694, -21.75657400278875286, 5.995467141624637009 ) ) ;
#21661 = CARTESIAN_POINT ( 'NONE',  ( 3.121324086407806231, -26.64985754041175525, 6.700000000000000178 ) ) ;
#21662 = CARTESIAN_POINT ( 'NONE',  ( 5.030284764849001000, -28.49206123220129783, 7.750000000000000888 ) ) ;
#21663 = VERTEX_POINT ( 'NONE', #29490 ) ;
#21664 = CARTESIAN_POINT ( 'NONE',  ( 22.39423033477626745, 4.887851171428074792, 3.091777426714782617 ) ) ;
#21665 = CARTESIAN_POINT ( 'NONE',  ( 81.16944410057618597, 61.30393124705405938, -1.011532654301245060 ) ) ;
#21666 = CARTESIAN_POINT ( 'NONE',  ( 79.34351131543186852, 65.42632830064323457, 2.956864960647761720 ) ) ;
#21667 = AXIS2_PLACEMENT_3D ( 'NONE', #473, #18564, #21681 ) ;
#21668 = CARTESIAN_POINT ( 'NONE',  ( -0.06304711255985051555, -32.47688463027607497, 6.874555630061442990 ) ) ;
#21669 = EDGE_LOOP ( 'NONE', ( #31487, #9889, #29859, #25399 ) ) ;
#21670 = CARTESIAN_POINT ( 'NONE',  ( 77.48353911088550205, 60.20448024992294478, -2.970791854447082603 ) ) ;
#21672 = DIRECTION ( 'NONE',  ( 1.000000000000000000, 0.000000000000000000, -0.000000000000000000 ) ) ;
#21671 = CARTESIAN_POINT ( 'NONE',  ( -72.23801069314184531, -46.35958874329211454, 5.855843091881858697 ) ) ;
#21673 = CARTESIAN_POINT ( 'NONE',  ( 0.5143470587258708315, -26.38350004588937381, 7.740055089680401679 ) ) ;
#21674 = ADVANCED_FACE ( 'NONE', ( #1299 ), #13836, .F. ) ;
#21675 = EDGE_CURVE ( 'NONE', #28854, #37831, #4183, .T. ) ;
#21676 = CARTESIAN_POINT ( 'NONE',  ( 81.53538963105238224, 62.13961868399401567, -2.518708746843058677 ) ) ;
#21677 = CARTESIAN_POINT ( 'NONE',  ( 76.63893934653985696, 63.44172143924968310, 3.539370024148535965 ) ) ;
#21678 = ORIENTED_EDGE ( 'NONE', *, *, #17819, .T. ) ;
#21679 = EDGE_CURVE ( 'NONE', #2075, #17900, #8732, .T. ) ;
#21680 = LINE ( 'NONE', #261, #33270 ) ;
#21681 = DIRECTION ( 'NONE',  ( 0.000000000000000000, 0.000000000000000000, -1.000000000000000000 ) ) ;
#21682 = CARTESIAN_POINT ( 'NONE',  ( 80.87103490326518340, 66.01227193428226769, 1.936735430445677197 ) ) ;
#21684 = PLANE ( 'NONE',  #22273 ) ;
#21683 = CARTESIAN_POINT ( 'NONE',  ( -4.448748702180642667, -26.64985754041175525, 6.700000000000000178 ) ) ;
#21685 = CARTESIAN_POINT ( 'NONE',  ( 30.98800548345937855, -0.8519925708576415735, -5.886550247782252221 ) ) ;
#21686 = PLANE ( 'NONE',  #4983 ) ;
#21687 = CARTESIAN_POINT ( 'NONE',  ( -62.99366871073556950, 35.53755692985882320, -6.184786337850739280 ) ) ;
#21688 = CARTESIAN_POINT ( 'NONE',  ( -62.74303057475812295, 35.98358351542167100, 5.167368988332134982 ) ) ;
#21689 = CARTESIAN_POINT ( 'NONE',  ( 27.36544478893236487, 1.086804081426588242, -4.476750403029456926 ) ) ;
#21690 = CIRCLE ( 'NONE', #18406, 2.999999999999998668 ) ;
#21691 = CARTESIAN_POINT ( 'NONE',  ( -0.000000000000000000, 13.37661300689600097, -2.500000000000000000 ) ) ;
#21692 = DIRECTION ( 'NONE',  ( 0.000000000000000000, -0.000000000000000000, -1.000000000000000000 ) ) ;
#21693 = CARTESIAN_POINT ( 'NONE',  ( 79.11873141236488038, 60.58998131946810162, 2.372212216456983214 ) ) ;
#21694 = CARTESIAN_POINT ( 'NONE',  ( -12.99139449055068596, 10.37661300689600097, 6.000000000000000000 ) ) ;
#21695 = ADVANCED_FACE ( 'NONE', ( #14229 ), #29882, .F. ) ;
#21696 = CARTESIAN_POINT ( 'NONE',  ( 36.99638130734812336, -3.220727926517238160, -5.952632950965317526 ) ) ;
#21697 = CARTESIAN_POINT ( 'NONE',  ( 71.52974698506822904, 58.56680916168235740, -3.757746881545229289 ) ) ;
#21698 = CARTESIAN_POINT ( 'NONE',  ( 79.89212576172681679, 63.66154800590240370, -1.000000000000000000 ) ) ;
#21699 = FACE_OUTER_BOUND ( 'NONE', #5457, .T. ) ;
#21700 = DIRECTION ( 'NONE',  ( 0.8660254037844252739, 0.5000000000000230926, 0.000000000000000000 ) ) ;
#21701 = CARTESIAN_POINT ( 'NONE',  ( -0.7974450458313169232, -25.21654760013375451, 7.635761828346577573 ) ) ;
#21702 = CARTESIAN_POINT ( 'NONE',  ( -18.24874870218063450, -25.49307895267003587, 6.700000000000000178 ) ) ;
#21703 = CARTESIAN_POINT ( 'NONE',  ( -10.34874870218063769, -25.49307895267003587, 6.700000000000000178 ) ) ;
#21704 = CARTESIAN_POINT ( 'NONE',  ( 2.829436171004394041, -26.36286689144161954, 7.692469944509199742 ) ) ;
#21705 = VECTOR ( 'NONE', #27505, 1000.000000000000114 ) ;
#21706 = ORIENTED_EDGE ( 'NONE', *, *, #3699, .T. ) ;
#21707 = CARTESIAN_POINT ( 'NONE',  ( 70.02038816076994010, 58.42250406220534131, -3.901551322707177416 ) ) ;
#21708 = EDGE_LOOP ( 'NONE', ( #30471, #34380, #4148, #21869 ) ) ;
#21709 = DIRECTION ( 'NONE',  ( 0.9396926207859126468, -0.3420201433256568890, -0.000000000000000000 ) ) ;
#21710 = LINE ( 'NONE', #8719, #28505 ) ;
#21711 = CARTESIAN_POINT ( 'NONE',  ( 1.280975525403379889, -26.19589825996822086, 6.882085323592684212 ) ) ;
#21712 = EDGE_CURVE ( 'NONE', #25728, #33766, #19478, .T. ) ;
#21713 = CARTESIAN_POINT ( 'NONE',  ( 5.028355742328307620, -30.26613402516411355, 7.768425012602594215 ) ) ;
#21714 = ORIENTED_EDGE ( 'NONE', *, *, #27060, .F. ) ;
#21715 = CARTESIAN_POINT ( 'NONE',  ( 22.38233119875572186, 4.942362494773947290, 3.043640801607715218 ) ) ;
#21716 = CIRCLE ( 'NONE', #3982, 9.804803391925412726 ) ;
#21717 = FILL_AREA_STYLE_COLOUR ( '', #11657 ) ;
#21718 = EDGE_CURVE ( 'NONE', #18768, #20340, #25998, .T. ) ;
#21719 = ORIENTED_EDGE ( 'NONE', *, *, #13709, .F. ) ;
#21720 = CARTESIAN_POINT ( 'NONE',  ( 80.18735707129573598, 62.48858554017570555, -3.489618106120242036 ) ) ;
#21721 = CARTESIAN_POINT ( 'NONE',  ( -1.483070179901938568, -30.76391300394762141, 7.670860738520329569 ) ) ;
#21722 = CARTESIAN_POINT ( 'NONE',  ( 81.94287803445135410, 63.22849810396151327, -2.713791510777194382 ) ) ;
#21723 = CARTESIAN_POINT ( 'NONE',  ( 79.04765299714190974, 64.87162515256790130, 3.322373183921397466 ) ) ;
#21724 = EDGE_CURVE ( 'NONE', #4303, #37042, #26566, .T. ) ;
#21725 = CARTESIAN_POINT ( 'NONE',  ( 4.345932563343239075, -27.43424125969082894, 6.880147297696982633 ) ) ;
#21726 = AXIS2_PLACEMENT_3D ( 'NONE', #28238, #15275, #40585 ) ;
#21728 = EDGE_LOOP ( 'NONE', ( #37620, #18078 ) ) ;
#21727 = CARTESIAN_POINT ( 'NONE',  ( -1.064602432027077050, -27.57915845623975670, 7.505001789837630000 ) ) ;
#21729 = CARTESIAN_POINT ( 'NONE',  ( 21.85643539959777115, -1.513967970512005268, 12.69801924519992120 ) ) ;
#21730 = ORIENTED_EDGE ( 'NONE', *, *, #10815, .T. ) ;
#21731 = CARTESIAN_POINT ( 'NONE',  ( -76.72287709695605429, 9.359952303362009118, 8.166909960842559713 ) ) ;
#21732 = CARTESIAN_POINT ( 'NONE',  ( -1.799429409603024332, -29.60556360950435817, 7.707924859530665529 ) ) ;
#21733 = FACE_OUTER_BOUND ( 'NONE', #32261, .T. ) ;
#21734 = VERTEX_POINT ( 'NONE', #13634 ) ;
#21735 = CARTESIAN_POINT ( 'NONE',  ( 1.592658322483926137, -32.96823108478886866, 7.768425012602593327 ) ) ;
#21736 = CARTESIAN_POINT ( 'NONE',  ( 1.649183331817654086, -32.96954544161381762, 6.892063359921931642 ) ) ;
#21737 = CARTESIAN_POINT ( 'NONE',  ( 36.13343955306980604, -1.529194832581077135, -5.642286574374616670 ) ) ;
#21738 = CARTESIAN_POINT ( 'NONE',  ( 4.907431569743298638, -30.69903822425716911, 7.691066658568948888 ) ) ;
#21739 = LINE ( 'NONE', #14715, #27922 ) ;
#21740 = CARTESIAN_POINT ( 'NONE',  ( -12.44874870218064267, -26.64985754041175525, 6.700000000000000178 ) ) ;
#21741 = CARTESIAN_POINT ( 'NONE',  ( 29.98495624012389982, -3.733826441308198962, 4.538579857738193724 ) ) ;
#21742 = CARTESIAN_POINT ( 'NONE',  ( 1.700390093233090871, -29.56993018339339940, 6.850000000000000533 ) ) ;
#21743 = CARTESIAN_POINT ( 'NONE',  ( 17.33572800788162738, 14.29660996616593849, -2.500000000000000444 ) ) ;
#21744 = CARTESIAN_POINT ( 'NONE',  ( 23.13463400706473649, 0.4140889092209439903, -5.868895817274544235 ) ) ;
#21745 = CARTESIAN_POINT ( 'NONE',  ( 36.53420504795911938, -1.804924688322298909, -5.759860367675933013 ) ) ;
#21746 = CARTESIAN_POINT ( 'NONE',  ( 26.91012592398995551, 1.445922882693422729, -4.391925638988915637 ) ) ;
#21747 = VERTEX_POINT ( 'NONE', #38532 ) ;
#21748 = CARTESIAN_POINT ( 'NONE',  ( 67.20767295658653495, 57.90495500903578829, 3.994504660676310159 ) ) ;
#21749 = CARTESIAN_POINT ( 'NONE',  ( 36.44546669202388500, -3.301925173002164815, 5.889632857546714284 ) ) ;
#21750 = CARTESIAN_POINT ( 'NONE',  ( -1.657912054741428554, -30.10078485551160554, 7.785172627573962778 ) ) ;
#21751 = EDGE_CURVE ( 'NONE', #8622, #1010, #7509, .T. ) ;
#21752 = DIRECTION ( 'NONE',  ( 1.000000000000000000, -0.000000000000000000, 0.000000000000000000 ) ) ;
#21753 = CARTESIAN_POINT ( 'NONE',  ( 85.43170627155664931, 2.122511629702291902, -4.702826977918449280 ) ) ;
#21754 = AXIS2_PLACEMENT_3D ( 'NONE', #2931, #21645, #16265 ) ;
#21756 = CARTESIAN_POINT ( 'NONE',  ( 22.22893185000578953, 4.118675178843608897, 2.394718637401875405 ) ) ;
#21755 = CARTESIAN_POINT ( 'NONE',  ( 33.90241230359465874, -5.503808810968542353, 0.4955917775451662566 ) ) ;
#21757 = VERTEX_POINT ( 'NONE', #32986 ) ;
#21758 = CARTESIAN_POINT ( 'NONE',  ( 25.10207142344970421, 2.436503095005564390, 4.015748850599299757 ) ) ;
#21759 = ADVANCED_FACE ( 'NONE', ( #7250 ), #22910, .F. ) ;
#21760 = DIRECTION ( 'NONE',  ( -0.8888117386314225987, -0.4582725098355650006, 0.000000000000000000 ) ) ;
#21761 = ORIENTED_EDGE ( 'NONE', *, *, #21640, .T. ) ;
#21762 = CARTESIAN_POINT ( 'NONE',  ( -70.50053432363721129, -21.68684479525939324, 3.984726467720987042 ) ) ;
#21763 = UNCERTAINTY_MEASURE_WITH_UNIT (LENGTH_MEASURE( 1.000000000000000082E-05 ), #10403, 'distance_accuracy_value', 'NONE');
#21764 = EDGE_CURVE ( 'NONE', #24059, #30463, #39650, .T. ) ;
#21765 = ORIENTED_EDGE ( 'NONE', *, *, #2249, .F. ) ;
#21766 = CARTESIAN_POINT ( 'NONE',  ( 80.62613562354505348, 62.33752749645043423, -3.268578535636858629 ) ) ;
#21767 = CARTESIAN_POINT ( 'NONE',  ( -42.24874870218063450, -26.64985754041175525, 6.700000000000000178 ) ) ;
#21768 = CARTESIAN_POINT ( 'NONE',  ( 80.81138441778081472, 62.13752223189714385, 3.030715982579940793 ) ) ;
#21770 = ORIENTED_EDGE ( 'NONE', *, *, #19521, .T. ) ;
#21769 = CARTESIAN_POINT ( 'NONE',  ( -0.8709512122991237559, -27.34547296267558281, 6.892063359921930754 ) ) ;
#21771 = CIRCLE ( 'NONE', #31654, 3.000000000000003997 ) ;
#21772 = EDGE_CURVE ( 'NONE', #17549, #347, #30381, .T. ) ;
#21774 = EDGE_CURVE ( 'NONE', #38484, #13794, #36268, .T. ) ;
#21773 = CARTESIAN_POINT ( 'NONE',  ( -19.07867591359219972, -26.64985754041175525, 6.700000000000000178 ) ) ;
#21775 = B_SPLINE_SURFACE_WITH_KNOTS ( 'NONE', 5, 3, ( 
 ( #38018, #16199, #13512, #13114, #16394, #16786, #9819, #3878, #19890, #38215, #25672, #1185, #13720, #770, #32272, #35162, #26286, #6935, #22398, #38820, #38617, #10012, #19290, #13302, #10214, #29167, #28765, #22795, #35366, #7137, #19697, #4071, #16586, #975, #26082, #32867, #17384, #23775, #11411, #29965, #33275, #20282, #7932, #27278, #23387, #17588, #2188 ),
 ( #36352, #2402, #33066, #20903, #30169, #4850, #20482, #1777, #8119, #39846, #29758, #14508, #36550, #24192, #30384, #14306, #5465, #20691, #18005, #27083, #8328, #5258, #33489, #4655, #26682, #1572, #26876, #39628, #11613, #39217, #26481, #5056, #10811, #11210, #17798, #36752, #33686, #17190, #23978, #11006, #23590, #39009, #35954, #1990, #14104, #14706, #8537 ),
 ( #21117, #30594, #7735, #39420, #36154, #8737, #2609, #15541, #120, #28095, #19045, #40649, #36957, #11817, #24399, #3021, #28301, #15128, #9352, #9153, #37158, #37754, #21933, #34310, #31404, #24816, #21320, #40240, #12651, #25020, #27684, #21529, #25226, #2809, #9564, #21729, #24603, #12451, #3229, #6079, #8944, #12024, #12242, #30803, #31608, #18614, #14924 ),
 ( #34507, #22144, #5879, #18416, #34716, #6495, #37358, #31201, #31004, #27493, #18832, #40042, #15331, #37557, #33895, #6283, #5671, #18211, #34105, #27886, #40433, #6697, #13063, #31812, #26036, #22754, #35713, #16739, #16152, #38776, #9770, #25624, #318, #38570, #37965, #35516, #38169, #16544, #7489, #19245, #29323, #26244, #7286, #15944, #1140, #28716, #4026 ),
 ( #19850, #3431, #28921, #25424, #928, #3829, #32023, #9972, #25830, #23145, #19654, #22953, #35321, #22353, #34920, #3628, #527, #22552, #16347, #10572, #20049, #13674, #29124, #35115, #722, #12857, #28509, #19449, #13462, #10377, #13263, #38366, #10163, #32225, #7090, #32419, #4218, #32629, #26638, #30129, #32824, #35914, #23933, #17541, #39172, #26835, #17145 ),
 ( #4423, #29525, #14264, #38966, #8278, #14660, #27232, #29717, #36307, #1944, #36505, #10968, #39375, #26440, #20242, #33224, #17750, #5010, #36704, #14462, #13873, #1337, #10766, #20643, #5213, #4615, #27037, #11165, #14060, #39797, #39581, #23736, #20852, #1733, #23342, #1526, #30335, #11366, #23548, #36113, #2142, #20442, #11566, #8079, #7890, #33445, #24142 ),
 ( #33021, #29915, #7693, #8487, #16947, #4810, #17338, #12195, #15490, #21884, #11978, #24556, #6237, #28250, #2761, #27840, #37110, #21068, #24974, #18781, #8896, #37312, #39998, #31155, #3184, #2971, #33642, #21479, #40599, #24348, #15698, #28048, #5417, #34057, #12406, #36912, #30756, #8692, #37511, #40393, #12607, #34461, #33844, #74, #27442, #2558, #17956 ),
 ( #9306, #15080, #34263, #25173, #21272, #31358, #37705, #30540, #2350, #14869, #5622, #21685, #15287, #24765, #6034, #11767, #18162, #27640, #40197, #5830, #18370, #30957, #18568, #9109, #5285, #21755, #40068, #30193, #30622, #40265, #2837, #12269, #11436, #5697, #17822, #2212, #5082, #2013, #27517, #24001, #21556, #27914, #40460, #14731, #8762, #15155, #37182 ) ),
 .UNSPECIFIED., .F., .T., .F.,
 ( 6, 2, 6 ),
 ( 4, 1, 1, 1, 1, 1, 1, 1, 1, 1, 1, 1, 1, 1, 1, 1, 1, 1, 1, 1, 1, 1, 1, 1, 1, 1, 1, 1, 1, 1, 1, 1, 1, 1, 1, 1, 1, 1, 1, 1, 1, 1, 1, 1, 4 ),
 ( 0.000000000000000000, 0.5000000000000000000, 1.000000000000000000 ),
 ( -0.09263217477943377909, -0.08973741931757646395, -0.08732512309936206474, -0.08539528612479052594, -0.08394790839386186143, -0.08250053066293322468, -0.08105315293200456017, -0.07960577520107590954, -0.07815839747014724503, -0.07671101973921859440, -0.07478118276464705561, -0.07285134579007553068, -0.07092150881550399188, -0.06947413108457534126, -0.06802675335364669063, -0.06609691637907515183, -0.06416707940450361303, -0.06223724242993208117, -0.06030740545536053543, -0.05789510923714611540, -0.05548281301893168843, -0.05355297604436015657, -0.05162313906978862471, -0.04921084285157419774, -0.04631608738971689648, -0.04342133192785958135, -0.04052657646600228009, -0.03763182100414497189, -0.03521952478593055186, -0.03328968781135902000, -0.03184231008043036937, -0.03039493234950170833, -0.02846509537493017647, -0.02605279915671574950, -0.02364050293850132947, -0.02171066596392979067, -0.01978082898935825881, -0.01785099201478672001, -0.01592115504021518121, -0.01399131806564364588, -0.01157902184742922412, -0.008684266385571917657, -0.005789510923714612060, -0.002894755461857306030, 0.000000000000000000 ),
 .UNSPECIFIED. ) ;
#21777 = CYLINDRICAL_SURFACE ( 'NONE', #8471, 9.804803391925412726 ) ;
#21776 = DIRECTION ( 'NONE',  ( 1.000000000000000000, 0.000000000000000000, 0.000000000000000000 ) ) ;
#21778 = LINE ( 'NONE', #34357, #18932 ) ;
#21779 = VECTOR ( 'NONE', #31102, 1000.000000000000000 ) ;
#21780 = CARTESIAN_POINT ( 'NONE',  ( 33.89795617549800255, -5.470764165105774346, -0.4365038096981310733 ) ) ;
#21781 = CARTESIAN_POINT ( 'NONE',  ( 21.73635333206707543, 6.105328942885613230, -3.274543301268284523 ) ) ;
#21782 = ORIENTED_EDGE ( 'NONE', *, *, #40033, .T. ) ;
#21783 = CARTESIAN_POINT ( 'NONE',  ( -77.95330471031414277, 33.71485196875532608, -12.49999999999999645 ) ) ;
#21784 = CARTESIAN_POINT ( 'NONE',  ( 24.65869693034278143, -1.551691026114866201, -6.728867248637652843 ) ) ;
#21785 = AXIS2_PLACEMENT_3D ( 'NONE', #5739, #11683, #24464 ) ;
#21786 = CARTESIAN_POINT ( 'NONE',  ( -80.35141725551916636, -6.644025400410976445, -3.371800178188818276 ) ) ;
#21787 = LINE ( 'NONE', #9828, #30737 ) ;
#21788 = CARTESIAN_POINT ( 'NONE',  ( 81.44732304147008506, 62.37541782542987789, 2.773332820898644524 ) ) ;
#21789 = CARTESIAN_POINT ( 'NONE',  ( 88.12503612275229159, -2.065192647045405838, -2.806263388478303256 ) ) ;
#21790 = CARTESIAN_POINT ( 'NONE',  ( -0.8560347025813198618, -25.25037435423009669, 7.695279973900954751 ) ) ;
#21791 = EDGE_LOOP ( 'NONE', ( #34050, #25510 ) ) ;
#21792 = DIRECTION ( 'NONE',  ( -1.000000000000000000, 0.000000000000000000, 0.000000000000000000 ) ) ;
#21793 = CARTESIAN_POINT ( 'NONE',  ( 21.53928041017985251, 7.378620751039662196, -0.9880446992327728273 ) ) ;
#21794 = ORIENTED_EDGE ( 'NONE', *, *, #11986, .T. ) ;
#21795 = CARTESIAN_POINT ( 'NONE',  ( 4.037301893384181994, -26.96438931088447433, 6.865482280155368322 ) ) ;
#21796 = CARTESIAN_POINT ( 'NONE',  ( 14.74464696855122980, -5.058300963987686139, -2.496493677045212856 ) ) ;
#21797 = CARTESIAN_POINT ( 'NONE',  ( -66.22295697852544549, 35.49170696305579753, -7.967283012324265279 ) ) ;
#21798 = DIRECTION ( 'NONE',  ( -1.000000000000000000, -0.000000000000000000, -0.000000000000000000 ) ) ;
#21799 = CARTESIAN_POINT ( 'NONE',  ( -62.99901854238083843, 37.98537211836831062, 4.070195263749428527 ) ) ;
#21800 = CARTESIAN_POINT ( 'NONE',  ( 27.40614744282377657, 0.9610282265797985835, 4.483790147270008575 ) ) ;
#21801 = CARTESIAN_POINT ( 'NONE',  ( -70.92837670882107659, -56.35932253828835314, 6.000000000000002665 ) ) ;
#21802 = VERTEX_POINT ( 'NONE', #37066 ) ;
#21804 = DIRECTION ( 'NONE',  ( 0.000000000000000000, -0.000000000000000000, -1.000000000000000000 ) ) ;
#21803 = CARTESIAN_POINT ( 'NONE',  ( 80.84834833306130975, 63.77578157039148721, -3.533418250979444064 ) ) ;
#21805 = FACE_OUTER_BOUND ( 'NONE', #7637, .T. ) ;
#21806 = CARTESIAN_POINT ( 'NONE',  ( -0.3487487021806359722, -25.49307895267003587, 6.700000000000000178 ) ) ;
#21807 = CARTESIAN_POINT ( 'NONE',  ( 0.8386806441584250260, -25.38437669007690900, 7.754798119455333705 ) ) ;
#21808 = ORIENTED_EDGE ( 'NONE', *, *, #28605, .F. ) ;
#21809 = CARTESIAN_POINT ( 'NONE',  ( -1.644339674572252052, -28.95929335108931468, 7.779495906702011965 ) ) ;
#21810 = VERTEX_POINT ( 'NONE', #21438 ) ;
#21811 = AXIS2_PLACEMENT_3D ( 'NONE', #24897, #25305, #25504 ) ;
#21812 = ORIENTED_EDGE ( 'NONE', *, *, #9150, .F. ) ;
#21813 = CARTESIAN_POINT ( 'NONE',  ( 80.62495340926818699, 62.95361341830508906, -3.497296750721713199 ) ) ;
#21814 = CARTESIAN_POINT ( 'NONE',  ( 33.46455515056310759, -3.089188617792877789, 5.429351193206847448 ) ) ;
#21815 = EDGE_LOOP ( 'NONE', ( #33207, #18993, #22583, #19334 ) ) ;
#21817 = CARTESIAN_POINT ( 'NONE',  ( 36.08990603727164626, -1.513213400165028810, 5.635049790240730161 ) ) ;
#21816 = CARTESIAN_POINT ( 'NONE',  ( 23.15206694985459634, 2.717029284607917372, 4.326704671169357752 ) ) ;
#21818 = ORIENTED_EDGE ( 'NONE', *, *, #25714, .F. ) ;
#21819 = EDGE_CURVE ( 'NONE', #10291, #13813, #4973, .T. ) ;
#21821 = ADVANCED_FACE ( 'NONE', ( #24097 ), #11327, .F. ) ;
#21820 = CARTESIAN_POINT ( 'NONE',  ( 4.739544865517091310, -28.04560401959518501, 6.911401339314954484 ) ) ;
#21823 = FACE_OUTER_BOUND ( 'NONE', #39800, .T. ) ;
#21822 = CARTESIAN_POINT ( 'NONE',  ( -69.92837670882109080, -0.6506954850797312950, 5.916079783099628564 ) ) ;
#21824 = CARTESIAN_POINT ( 'NONE',  ( 3.613857606807241218, -32.50872529095400409, 7.139344958878409919 ) ) ;
#21825 = DIRECTION ( 'NONE',  ( -1.000000000000000000, 0.000000000000000000, 0.000000000000000000 ) ) ;
#21826 = CARTESIAN_POINT ( 'NONE',  ( 73.06729433089581960, 60.84378783247667144, 3.914122288852233567 ) ) ;
#21827 = EDGE_LOOP ( 'NONE', ( #36771, #29625, #34799, #4704 ) ) ;
#21828 = CARTESIAN_POINT ( 'NONE',  ( 23.25171722262629359, 3.194370665195247483, -3.902736047147622234 ) ) ;
#21829 = ORIENTED_EDGE ( 'NONE', *, *, #37038, .T. ) ;
#21830 = PLANE ( 'NONE',  #36225 ) ;
#21831 = CARTESIAN_POINT ( 'NONE',  ( 21.85643539959779957, -14.30241103581959727, -6.272691714111175543 ) ) ;
#21832 = CARTESIAN_POINT ( 'NONE',  ( 17.10505430645456926, 14.50076029598319849, 3.172244300429228225 ) ) ;
#21833 = VERTEX_POINT ( 'NONE', #23892 ) ;
#21834 = AXIS2_PLACEMENT_3D ( 'NONE', #24790, #9326, #19018 ) ;
#21835 = ORIENTED_EDGE ( 'NONE', *, *, #38488, .F. ) ;
#21836 = CARTESIAN_POINT ( 'NONE',  ( 37.19747299874393320, -2.841585884120807481, 5.999818732555961098 ) ) ;
#21837 = CARTESIAN_POINT ( 'NONE',  ( 79.85781052176636763, 66.03394566247145292, 2.299173245602477156 ) ) ;
#21838 = CARTESIAN_POINT ( 'NONE',  ( 86.99908277331161344, 0.6362256001576577225, -5.325422653610870860 ) ) ;
#21839 = ORIENTED_EDGE ( 'NONE', *, *, #13387, .T. ) ;
#21840 = CARTESIAN_POINT ( 'NONE',  ( -0.9271279775035500270, -27.41211907304282036, 7.695279973900954751 ) ) ;
#21841 = ORIENTED_EDGE ( 'NONE', *, *, #27383, .T. ) ;
#21842 = CARTESIAN_POINT ( 'NONE',  ( 14.80252671224570271, -4.520290230480198623, 2.514186659199406204 ) ) ;
#21843 = DIRECTION ( 'NONE',  ( 0.000000000000000000, 0.000000000000000000, 1.000000000000000000 ) ) ;
#21844 = CARTESIAN_POINT ( 'NONE',  ( 36.64694695204426722, -2.460141890980504620, -5.926040400264396268 ) ) ;
#21845 = CARTESIAN_POINT ( 'NONE',  ( 5.100032641329620198, -29.62024639473925092, 7.785868773668302545 ) ) ;
#21846 = DIRECTION ( 'NONE',  ( 1.000000000000000000, 0.000000000000000000, 0.000000000000000000 ) ) ;
#21847 = EDGE_CURVE ( 'NONE', #530, #24953, #21335, .T. ) ;
#21848 = CARTESIAN_POINT ( 'NONE',  ( -26.24874870218063450, -25.49307895267003587, 6.700000000000000178 ) ) ;
#21849 = ORIENTED_EDGE ( 'NONE', *, *, #36261, .T. ) ;
#21850 = ORIENTED_EDGE ( 'NONE', *, *, #10410, .F. ) ;
#21851 = CARTESIAN_POINT ( 'NONE',  ( 36.88753254950347582, -3.349785859984652614, 5.911062257491906280 ) ) ;
#21852 = CARTESIAN_POINT ( 'NONE',  ( -71.87513448197603338, -0.4420453205300980959, 3.925045345733726432 ) ) ;
#21853 = CARTESIAN_POINT ( 'NONE',  ( 66.55222248544532704, 57.88363434508141125, -3.999616584014993759 ) ) ;
#21854 = CARTESIAN_POINT ( 'NONE',  ( 86.43572624768425783, -0.5192074800720990480, -5.777013305174518720 ) ) ;
#21855 = EDGE_CURVE ( 'NONE', #34205, #17894, #17917, .T. ) ;
#21856 = ORIENTED_EDGE ( 'NONE', *, *, #39341, .T. ) ;
#21857 = DIRECTION ( 'NONE',  ( -0.000000000000000000, -0.000000000000000000, -1.000000000000000000 ) ) ;
#21858 = CARTESIAN_POINT ( 'NONE',  ( -74.21080977438080595, 8.885293297773669607, -9.447016131426053676 ) ) ;
#21859 = DIRECTION ( 'NONE',  ( 0.000000000000000000, 0.000000000000000000, 1.000000000000000000 ) ) ;
#21860 = ORIENTED_EDGE ( 'NONE', *, *, #21718, .F. ) ;
#21861 = FACE_BOUND ( 'NONE', #18837, .T. ) ;
#21862 = DIRECTION ( 'NONE',  ( -0.000000000000000000, -1.000000000000000000, -0.000000000000000000 ) ) ;
#21863 = ORIENTED_EDGE ( 'NONE', *, *, #28790, .F. ) ;
#21864 = CARTESIAN_POINT ( 'NONE',  ( 24.36694571186475144, 3.146468230158969703, 3.351613297348657650 ) ) ;
#21865 = CARTESIAN_POINT ( 'NONE',  ( 82.53887461166610251, 63.53329618120191924, -1.555014038483378158 ) ) ;
#21866 = CARTESIAN_POINT ( 'NONE',  ( 81.13529310646420356, 61.59586411174932863, 2.189516896894247999 ) ) ;
#21868 = EDGE_CURVE ( 'NONE', #15748, #37942, #26591, .T. ) ;
#21867 = CARTESIAN_POINT ( 'NONE',  ( 2.882556208928725550, -26.38205034947389649, 7.779495906702015517 ) ) ;
#21869 = ORIENTED_EDGE ( 'NONE', *, *, #35802, .F. ) ;
#21870 = CARTESIAN_POINT ( 'NONE',  ( 77.29397510068352517, 60.62518447217949813, -3.385286751607444966 ) ) ;
#21872 = DIRECTION ( 'NONE',  ( 0.000000000000000000, 0.000000000000000000, 1.000000000000000000 ) ) ;
#21871 = CARTESIAN_POINT ( 'NONE',  ( 2.375388416495339605, -26.13562163180044706, 6.869132338375688818 ) ) ;
#21873 = CARTESIAN_POINT ( 'NONE',  ( 16.45937104885421931, 9.965318428467051959, -2.758229892786640214 ) ) ;
#21874 = CARTESIAN_POINT ( 'NONE',  ( 81.36706168520306903, 62.61468991663324601, -3.015642068896332795 ) ) ;
#21875 = CARTESIAN_POINT ( 'NONE',  ( 79.63092111360344916, 60.86998874196343223, 2.418543376929441546 ) ) ;
#21876 = VECTOR ( 'NONE', #23910, 1000.000000000000000 ) ;
#21877 = ORIENTED_EDGE ( 'NONE', *, *, #33534, .T. ) ;
#21878 = DIRECTION ( 'NONE',  ( -0.9999026450364576490, -0.01395351027862084224, 0.000000000000000000 ) ) ;
#21879 = CARTESIAN_POINT ( 'NONE',  ( 0.5197218266442334977, -32.86477804699348582, 7.750000000000000888 ) ) ;
#21880 = CARTESIAN_POINT ( 'NONE',  ( 82.21693166776744022, 64.09145645796296265, 2.325514254128254521 ) ) ;
#21881 =( BOUNDED_CURVE ( )  B_SPLINE_CURVE ( 3, ( #37005, #15178, #2659, #11258 ),
 .UNSPECIFIED., .F., .F. ) 
 B_SPLINE_CURVE_WITH_KNOTS ( ( 4, 4 ),
 ( 4.708531083176467291, 4.895802057644188743 ),
 .UNSPECIFIED. ) 
 CURVE ( )  GEOMETRIC_REPRESENTATION_ITEM ( )  RATIONAL_B_SPLINE_CURVE ( ( 1.000000000000000000, 0.9970795998553221295, 0.9970795998553221295, 1.000000000000000000 ) ) 
 REPRESENTATION_ITEM ( '' )  );
#21883 = CARTESIAN_POINT ( 'NONE',  ( -1.581856393934390814, -30.78519064826367568, 7.643192810543816051 ) ) ;
#21882 = CARTESIAN_POINT ( 'NONE',  ( 4.260855366779333409, -31.95614730464330933, 6.912143950357351407 ) ) ;
#21884 = CARTESIAN_POINT ( 'NONE',  ( 28.96592479936138176, -0.01829609152130128036, -5.755841479376210934 ) ) ;
#21885 = LINE ( 'NONE', #12608, #31305 ) ;
#21886 = CARTESIAN_POINT ( 'NONE',  ( -2.978675913592195190, -26.64985754041175525, 6.700000000000000178 ) ) ;
#21887 = CARTESIAN_POINT ( 'NONE',  ( -64.50921092724549055, 36.42665533667680933, 5.809226461016177012 ) ) ;
#21888 = CARTESIAN_POINT ( 'NONE',  ( -94.24726447194083789, -65.19654454972992141, -8.800414904976364028 ) ) ;
#21889 = ORIENTED_EDGE ( 'NONE', *, *, #1597, .T. ) ;
#21890 = CARTESIAN_POINT ( 'NONE',  ( -53.21549048184568420, -38.28842912540938670, -4.152976064860135708 ) ) ;
#21891 = CARTESIAN_POINT ( 'NONE',  ( -22.34874870218063947, -25.49307895267003587, 6.700000000000000178 ) ) ;
#21892 = CARTESIAN_POINT ( 'NONE',  ( -73.79226524390077202, -1.360417495813321054, 15.50000000000000000 ) ) ;
#21893 = CARTESIAN_POINT ( 'NONE',  ( 33.04859423313239830, -0.2660396992994370491, -5.100192512784728294 ) ) ;
#21894 = CARTESIAN_POINT ( 'NONE',  ( 77.27624361166392930, 60.01008998901625091, -2.873380611938707752 ) ) ;
#21895 = FACE_OUTER_BOUND ( 'NONE', #35165, .T. ) ;
#21896 = FACE_OUTER_BOUND ( 'NONE', #2996, .T. ) ;
#21897 = CARTESIAN_POINT ( 'NONE',  ( 0.5095177897111177190, -32.85964367047046153, 7.762796336881260473 ) ) ;
#21898 = CARTESIAN_POINT ( 'NONE',  ( 1.531218635892081847, -33.06583936671340496, 7.013842709614101167 ) ) ;
#21899 = CARTESIAN_POINT ( 'NONE',  ( 1.680225990343694908, -26.16998345069513832, 7.643333865083956624 ) ) ;
#21900 = EDGE_CURVE ( 'NONE', #36272, #32421, #31519, .T. ) ;
#21901 = CIRCLE ( 'NONE', #8291, 7.999999999999992895 ) ;
#21902 = CARTESIAN_POINT ( 'NONE',  ( -62.85296432947374967, 36.91960874151965299, -4.452026683640994520 ) ) ;
#21903 = LINE ( 'NONE', #6255, #13858 ) ;
#21904 = VERTEX_POINT ( 'NONE', #25544 ) ;
#21905 = EDGE_CURVE ( 'NONE', #4105, #25100, #37725, .T. ) ;
#21906 = CARTESIAN_POINT ( 'NONE',  ( -59.00110696496997775, 28.68040728033255249, -6.999999999999999112 ) ) ;
#21907 = CARTESIAN_POINT ( 'NONE',  ( 69.19640405677364470, 58.81667877646589204, -3.990151341881418290 ) ) ;
#21908 = CIRCLE ( 'NONE', #17936, 0.1000000000000028644 ) ;
#21909 = ADVANCED_FACE ( 'NONE', ( #9887 ), #37271, .F. ) ;
#21910 = ORIENTED_EDGE ( 'NONE', *, *, #38624, .F. ) ;
#21911 = CARTESIAN_POINT ( 'NONE',  ( -70.92837670224925262, -21.78291075600659354, 3.999987187540717137 ) ) ;
#21912 = CARTESIAN_POINT ( 'NONE',  ( -20.24874870218063805, -26.64985754041175525, 6.700000000000000178 ) ) ;
#21913 = CARTESIAN_POINT ( 'NONE',  ( 5.017169059587130775, -28.45235365878695077, 6.865554069792297653 ) ) ;
#21914 = CARTESIAN_POINT ( 'NONE',  ( -1.425344313683088782, -28.23208962058615512, 6.895222827070020877 ) ) ;
#21915 = CARTESIAN_POINT ( 'NONE',  ( 4.884862803864217895, -30.76120410455747844, 7.782167645815905033 ) ) ;
#21916 = CARTESIAN_POINT ( 'NONE',  ( 5.043346053430708409, -30.19012809388586760, 7.782167645815904145 ) ) ;
#21917 = ORIENTED_EDGE ( 'NONE', *, *, #12983, .T. ) ;
#21918 = CARTESIAN_POINT ( 'NONE',  ( 21.82942332946822361, 5.970316737997020340, 3.131952444615608844 ) ) ;
#21919 = DIRECTION ( 'NONE',  ( 0.6834397476448837994, 0.000000000000000000, -0.7300069255418729641 ) ) ;
#21920 = CARTESIAN_POINT ( 'NONE',  ( 18.42522192648813828, -3.123253340230073061, 3.033926698805842648 ) ) ;
#21921 = AXIS2_PLACEMENT_3D ( 'NONE', #15343, #27899, #29135 ) ;
#21922 = EDGE_CURVE ( 'NONE', #9338, #23233, #38085, .T. ) ;
#21923 = ORIENTED_EDGE ( 'NONE', *, *, #38805, .F. ) ;
#21924 = CARTESIAN_POINT ( 'NONE',  ( 79.60787101065389493, 62.86536646861404165, -3.718817779187658434 ) ) ;
#21926 = CARTESIAN_POINT ( 'NONE',  ( -1.677641490061642759, -29.95580920881881681, 6.929923840112066635 ) ) ;
#21925 = CARTESIAN_POINT ( 'NONE',  ( 22.65837895044245798, 0.3099126875621054378, 6.437328739972214109 ) ) ;
#21927 = CARTESIAN_POINT ( 'NONE',  ( 81.48469013494968749, 61.56585122427132006, -1.622497907168742648 ) ) ;
#21928 = CARTESIAN_POINT ( 'NONE',  ( 80.02751534128088906, 63.03952351013455768, 3.681573067026198576 ) ) ;
#21929 = CARTESIAN_POINT ( 'NONE',  ( 4.402002282394398058, -27.50561746263473495, 6.871394612369932986 ) ) ;
#21930 = LINE ( 'NONE', #525, #219 ) ;
#21932 = VERTEX_POINT ( 'NONE', #31320 ) ;
#21931 = DIRECTION ( 'NONE',  ( -0.000000000000000000, -0.000000000000000000, -1.000000000000000000 ) ) ;
#21933 = CARTESIAN_POINT ( 'NONE',  ( 21.85643539959779957, -10.54057479330554159, -5.012605957032298498 ) ) ;
#21934 = LINE ( 'NONE', #6284, #25299 ) ;
#21935 = EDGE_LOOP ( 'NONE', ( #18055, #23977, #2681, #17023 ) ) ;
#21936 = CARTESIAN_POINT ( 'NONE',  ( -72.92592677944759316, 1.059812494767570668, 9.858470738818239099 ) ) ;
#21937 = CARTESIAN_POINT ( 'NONE',  ( 36.50792169068728299, -3.548421012104517658, 5.802103936190841083 ) ) ;
#21938 = ORIENTED_EDGE ( 'NONE', *, *, #39487, .F. ) ;
#21939 = EDGE_CURVE ( 'NONE', #39722, #11704, #21524, .T. ) ;
#21940 = FACE_OUTER_BOUND ( 'NONE', #2642, .T. ) ;
#21941 = ADVANCED_FACE ( 'NONE', ( #12564 ), #3142, .F. ) ;
#21942 = CARTESIAN_POINT ( 'NONE',  ( 1.729679958306010068, -32.96980524772960308, 7.730758795053805699 ) ) ;
#21943 = CARTESIAN_POINT ( 'NONE',  ( 1.635900804779897300, -32.96932766995732322, 6.880147297696981745 ) ) ;
#21944 = CARTESIAN_POINT ( 'NONE',  ( 21.74105148488215988, 4.237279870184942787, -2.792868468085587530 ) ) ;
#21945 = CARTESIAN_POINT ( 'NONE',  ( -1.555626379089409372, -30.54891009224447629, 7.006423389747794772 ) ) ;
#21946 = CARTESIAN_POINT ( 'NONE',  ( 3.828902690058404445, -32.22125608946033992, 6.874555630061442102 ) ) ;
#21947 = CARTESIAN_POINT ( 'NONE',  ( 20.06265332725812556, 6.856321025424916726, 3.229911059913491478 ) ) ;
#21948 = CARTESIAN_POINT ( 'NONE',  ( -16.87867591359218977, -24.55319635012989110, 6.700000000000000178 ) ) ;
#21949 = FACE_OUTER_BOUND ( 'NONE', #5097, .T. ) ;
#21950 = DIRECTION ( 'NONE',  ( 1.000000000000000000, 0.000000000000000000, 0.000000000000000000 ) ) ;
#21951 = AXIS2_PLACEMENT_3D ( 'NONE', #12771, #6813, #31937 ) ;
#21952 = CARTESIAN_POINT ( 'NONE',  ( 3.913290293412393872, -32.15122301917286762, 7.695279973900954751 ) ) ;
#21953 = CIRCLE ( 'NONE', #9435, 34.02204673211314656 ) ;
#21954 = CARTESIAN_POINT ( 'NONE',  ( 23.14765463162058623, 0.4541928285590982606, -5.841642121512133023 ) ) ;
#21955 = CARTESIAN_POINT ( 'NONE',  ( 29.53970505027308491, -3.873674039035061689, -4.297879082457085609 ) ) ;
#21956 = CARTESIAN_POINT ( 'NONE',  ( 24.80520132849324710, 2.592517504530978290, -3.945774167130594812 ) ) ;
#21957 = EDGE_LOOP ( 'NONE', ( #556, #18025, #30132, #14387, #20780, #39554, #24901 ) ) ;
#21958 = EDGE_CURVE ( 'NONE', #863, #2870, #4891, .T. ) ;
#21960 = EDGE_CURVE ( 'NONE', #14737, #37640, #22135, .T. ) ;
#21959 = CARTESIAN_POINT ( 'NONE',  ( 66.95869957004099149, 58.13407781516350070, 3.995640437668404044 ) ) ;
#21961 = CARTESIAN_POINT ( 'NONE',  ( 20.53310891050050557, 3.934803127027559189, 3.411086259235923457 ) ) ;
#21962 = CARTESIAN_POINT ( 'NONE',  ( -1.666668308769183815, -30.04207646230481998, 7.757178535559534183 ) ) ;
#21963 = EDGE_CURVE ( 'NONE', #1128, #29803, #37876, .T. ) ;
#21964 = DIRECTION ( 'NONE',  ( 0.4690749385695646145, 0.8831583674551010121, 0.000000000000000000 ) ) ;
#21965 = PRODUCT_DEFINITION ( 'UNKNOWN', '', #35365, #31238 ) ;
#21966 = CARTESIAN_POINT ( 'NONE',  ( 86.86785128967072467, -0.4505172232112327757, -5.755800129507335328 ) ) ;
#21967 = CARTESIAN_POINT ( 'NONE',  ( 35.63404480038042976, -3.169100885857628391, -5.767952522366300627 ) ) ;
#21968 = ORIENTED_EDGE ( 'NONE', *, *, #27658, .T. ) ;
#21969 = CARTESIAN_POINT ( 'NONE',  ( 26.04389118395324587, 1.945336293897782287, 4.218032799664143795 ) ) ;
#21970 = EDGE_CURVE ( 'NONE', #32703, #169, #6198, .T. ) ;
#21971 = CARTESIAN_POINT ( 'NONE',  ( 1.551251297819356001, -25.49307895267003587, 6.700000000000000178 ) ) ;
#21972 = VERTEX_POINT ( 'NONE', #31933 ) ;
#21973 = LINE ( 'NONE', #28339, #9719 ) ;
#21974 = ORIENTED_EDGE ( 'NONE', *, *, #26010, .T. ) ;
#21975 = CARTESIAN_POINT ( 'NONE',  ( 80.48490785079538057, 62.58389448792956955, -3.438247877890626469 ) ) ;
#21976 = CARTESIAN_POINT ( 'NONE',  ( 4.487153213455422396, -27.45239593059636363, 7.013842709614101167 ) ) ;
#21977 = CARTESIAN_POINT ( 'NONE',  ( 78.79145472225366120, 65.75511795602321286, 2.294512580621463016 ) ) ;
#21978 = B_SPLINE_CURVE_WITH_KNOTS ( 'NONE', 3,
 ( #36881, #8052, #21040, #20611 ),
 .UNSPECIFIED., .F., .F.,
 ( 4, 4 ),
 ( 0.000000000000000000, 6.391136169897297484E-06 ),
 .UNSPECIFIED. ) ;
#21981 = ORIENTED_EDGE ( 'NONE', *, *, #33410, .T. ) ;
#21980 = ORIENTED_EDGE ( 'NONE', *, *, #36132, .T. ) ;
#21979 = DIRECTION ( 'NONE',  ( 0.7055275666422172742, -0.2567910337120293818, 0.6605219282605377940 ) ) ;
#21982 = CIRCLE ( 'NONE', #4232, 0.1000000000000028644 ) ;
#21983 = VECTOR ( 'NONE', #13812, 1000.000000000000000 ) ;
#21984 = CARTESIAN_POINT ( 'NONE',  ( 0.03641831304798801017, -26.49892041654603503, 7.776484688137387025 ) ) ;
#21985 = CARTESIAN_POINT ( 'NONE',  ( 24.80613193118815474, -5.883788488468095323, 2.846725823111817100 ) ) ;
#21986 = CARTESIAN_POINT ( 'NONE',  ( -71.54191492143920073, -21.58360693942124797, 9.981599438687137393 ) ) ;
#21987 = CARTESIAN_POINT ( 'NONE',  ( -1.425774885472621767, -28.23310838303483550, 7.013842709614101167 ) ) ;
#21988 = CARTESIAN_POINT ( 'NONE',  ( 21.71920171916170261, 6.265005891781191494, -3.215796620455622090 ) ) ;
#21989 = ORIENTED_EDGE ( 'NONE', *, *, #12845, .T. ) ;
#21990 = DIRECTION ( 'NONE',  ( -0.9396926207859007674, 0.3420201433256899737, 0.000000000000000000 ) ) ;
#21991 = VECTOR ( 'NONE', #17826, 1000.000000000000000 ) ;
#21992 = CARTESIAN_POINT ( 'NONE',  ( -80.83685820618015327, -6.606126994342639946, -1.409722980286805427 ) ) ;
#21993 = VECTOR ( 'NONE', #22246, 1000.000000000000000 ) ;
#21994 = CARTESIAN_POINT ( 'NONE',  ( -89.20959394718985891, -29.55642757665872722, 7.635761828346577573 ) ) ;
#21995 = CARTESIAN_POINT ( 'NONE',  ( 81.46310422711934507, 61.87916883045102878, 2.296576099417781958 ) ) ;
#21996 = CARTESIAN_POINT ( 'NONE',  ( 87.44477293306643162, -1.228341977218806447, 4.926563918429203603 ) ) ;
#21997 = CYLINDRICAL_SURFACE ( 'NONE', #35190, 1.000000000000003997 ) ;
#21998 = ORIENTED_EDGE ( 'NONE', *, *, #22799, .T. ) ;
#21999 = CARTESIAN_POINT ( 'NONE',  ( -42.34874870218063592, -26.64985754041175525, 6.700000000000000178 ) ) ;
#22000 = CARTESIAN_POINT ( 'NONE',  ( 4.583196249787880205, -31.37254857199200231, 7.757178535559535071 ) ) ;
#22001 = EDGE_CURVE ( 'NONE', #16672, #17495, #11680, .T. ) ;
#22002 = EDGE_LOOP ( 'NONE', ( #16569, #6205, #36682, #29547 ) ) ;
#22003 = DIRECTION ( 'NONE',  ( -0.000000000000000000, 0.000000000000000000, 1.000000000000000000 ) ) ;
#22004 = EDGE_CURVE ( 'NONE', #12066, #25120, #8818, .T. ) ;
#22005 = CARTESIAN_POINT ( 'NONE',  ( 1.090397816225957550, 0.5999999999999995337, 4.012069227840649788 ) ) ;
#22006 = CARTESIAN_POINT ( 'NONE',  ( 4.702906489365862974, -27.97465601193010798, 7.757178535559532406 ) ) ;
#22007 = CARTESIAN_POINT ( 'NONE',  ( -4.878675913592187108, -24.55319635012989110, 6.700000000000000178 ) ) ;
#22008 = CARTESIAN_POINT ( 'NONE',  ( 36.79751133535093288, -2.556301215552558848, 5.949539613692945039 ) ) ;
#22009 = EDGE_CURVE ( 'NONE', #40651, #25150, #9467, .T. ) ;
#22010 = AXIS2_PLACEMENT_3D ( 'NONE', #17958, #20855, #11770 ) ;
#22011 = CARTESIAN_POINT ( 'NONE',  ( 87.46579090913228072, 0.1119968706995537605, 4.710562776971725540 ) ) ;
#22012 = ORIENTED_EDGE ( 'NONE', *, *, #15068, .F. ) ;
#22013 = LINE ( 'NONE', #18913, #17787 ) ;
#22014 = CARTESIAN_POINT ( 'NONE',  ( -1.351882211874637418, -31.25406282615607267, 7.784725160561909441 ) ) ;
#22015 = FACE_OUTER_BOUND ( 'NONE', #28858, .T. ) ;
#22016 = CARTESIAN_POINT ( 'NONE',  ( 14.71881405247904340, 13.02603684036817633, -2.499237524637579533 ) ) ;
#22017 = VERTEX_POINT ( 'NONE', #34631 ) ;
#22018 = CARTESIAN_POINT ( 'NONE',  ( 25.30743677325165208, -5.496855584100603487, -2.999765155844900555 ) ) ;
#22019 = AXIS2_PLACEMENT_3D ( 'NONE', #16700, #7655, #10531 ) ;
#22020 = ORIENTED_EDGE ( 'NONE', *, *, #16552, .T. ) ;
#22021 = DIRECTION ( 'NONE',  ( 0.000000000000000000, 0.000000000000000000, 1.000000000000000000 ) ) ;
#22023 = VERTEX_POINT ( 'NONE', #4136 ) ;
#22022 = VERTEX_POINT ( 'NONE', #12975 ) ;
#22024 = CARTESIAN_POINT ( 'NONE',  ( 79.62856576210180037, 64.96968976106111882, -3.364061116559609932 ) ) ;
#22025 = CARTESIAN_POINT ( 'NONE',  ( -62.92837670882106238, 13.37661300689599742, 6.000000000000000000 ) ) ;
#22027 = CARTESIAN_POINT ( 'NONE',  ( -12.99139449055068241, 13.37661300689600097, -2.500000000000000444 ) ) ;
#22026 = CARTESIAN_POINT ( 'NONE',  ( 22.65299298941167550, 3.119508358272978121, 4.311559539158433374 ) ) ;
#22028 = ORIENTED_EDGE ( 'NONE', *, *, #17745, .F. ) ;
#22029 = CARTESIAN_POINT ( 'NONE',  ( 81.39647959751735584, 65.22731470771807949, -2.622983904469595284 ) ) ;
#22030 = CARTESIAN_POINT ( 'NONE',  ( 3.055030623276686619, -26.34271016697629619, 7.013842709614101167 ) ) ;
#22032 = CARTESIAN_POINT ( 'NONE',  ( 85.88576331275629627, 1.886758859582599479, -4.135933360337332942 ) ) ;
#22031 = DIRECTION ( 'NONE',  ( 1.000000000000000000, -0.000000000000000000, 0.000000000000000000 ) ) ;
#22033 = DIRECTION ( 'NONE',  ( 0.000000000000000000, -0.000000000000000000, 1.000000000000000000 ) ) ;
#22034 = CARTESIAN_POINT ( 'NONE',  ( -71.92837670882107659, -20.78299143688747819, 5.916079783099617906 ) ) ;
#22035 = CARTESIAN_POINT ( 'NONE',  ( 73.28665133690081745, 61.87344754340890773, 3.624554307483654814 ) ) ;
#22036 = B_SPLINE_CURVE_WITH_KNOTS ( 'NONE', 3,
 ( #23599, #1392, #4860, #14519, #17394, #11423, #19903, #26298, #4274, #32677, #38830, #13923, #32876, #27091, #16797, #29378, #29974, #4666, #10624, #33499, #9165, #5267, #37369, #8337, #18221 ),
 .UNSPECIFIED., .F., .F.,
 ( 4, 3, 3, 3, 3, 3, 3, 3, 4 ),
 ( 6.468151674593845140E-05, 9.076621574721758135E-05, 0.0001210204262067946055, 0.0001512763324577414510, 0.0001815301820994176898, 0.0002117781465860678054, 0.0002420274594459698408, 0.0002722905548971106386, 0.0002816827545175582459 ),
 .UNSPECIFIED. ) ;
#22037 = CARTESIAN_POINT ( 'NONE',  ( 23.02787331254640790, 3.347463497797338761, -3.909392201422248192 ) ) ;
#22038 = ORIENTED_EDGE ( 'NONE', *, *, #7217, .T. ) ;
#22039 = VECTOR ( 'NONE', #29535, 1000.000000000000227 ) ;
#22040 = CARTESIAN_POINT ( 'NONE',  ( 21.85643539959774273, 10.29907807357824723, -3.463423532579224418 ) ) ;
#22041 = CARTESIAN_POINT ( 'NONE',  ( -38.44874870218063734, -26.64985754041175525, 6.700000000000000178 ) ) ;
#22042 = ORIENTED_EDGE ( 'NONE', *, *, #13134, .F. ) ;
#22043 = CARTESIAN_POINT ( 'NONE',  ( -1.450854365928797352, -28.29334945402236556, 7.754798119455333705 ) ) ;
#22044 = CARTESIAN_POINT ( 'NONE',  ( 80.87888400807986500, 65.31646575666034948, 2.869341960395464408 ) ) ;
#22045 = CIRCLE ( 'NONE', #4292, 3.499999999999999556 ) ;
#22046 = CARTESIAN_POINT ( 'NONE',  ( 85.25019696446999262, 2.600657147776545663, -2.704904232406868836 ) ) ;
#22047 = ORIENTED_EDGE ( 'NONE', *, *, #24072, .F. ) ;
#22048 = CIRCLE ( 'NONE', #14782, 3.499999999999999556 ) ;
#22049 = CARTESIAN_POINT ( 'NONE',  ( 0.5182239775374835045, -32.75781001731291298, 7.779495906702013741 ) ) ;
#22050 = CARTESIAN_POINT ( 'NONE',  ( 14.96872153645507630, -6.096775576253210538, 2.530506653653641802 ) ) ;
#22051 = CARTESIAN_POINT ( 'NONE',  ( 36.79872796904915333, -2.554582093385345587, -5.949729498805945482 ) ) ;
#22052 = CARTESIAN_POINT ( 'NONE',  ( 5.100395873294749194, -29.56450258678017562, 7.763628509615285722 ) ) ;
#22053 = B_SPLINE_CURVE_WITH_KNOTS ( 'NONE', 3,
 ( #14247, #26425, #4408, #32811, #38552, #7273, #7876, #38762, #10555, #39359 ),
 .UNSPECIFIED., .F., .F.,
 ( 4, 3, 3, 4 ),
 ( 0.0001585009270395749373, 0.0001815657551981825679, 0.0002118214035944122073, 0.0002170292169044788736 ),
 .UNSPECIFIED. ) ;
#22054 = DIRECTION ( 'NONE',  ( 1.682730792515357087E-16, -1.000000000000000000, 0.000000000000000000 ) ) ;
#22055 = LINE ( 'NONE', #31934, #18915 ) ;
#22056 = EDGE_CURVE ( 'NONE', #27310, #6781, #33180, .T. ) ;
#22057 = EDGE_CURVE ( 'NONE', #5089, #20694, #38285, .T. ) ;
#22058 = CARTESIAN_POINT ( 'NONE',  ( 3.651251297819360531, -26.64985754041175525, 6.700000000000000178 ) ) ;
#22059 = EDGE_CURVE ( 'NONE', #29405, #10219, #13581, .T. ) ;
#22060 = VERTEX_POINT ( 'NONE', #1446 ) ;
#22061 = EDGE_LOOP ( 'NONE', ( #33378, #19557, #26073, #21116 ) ) ;
#22062 = CARTESIAN_POINT ( 'NONE',  ( 30.88230511604370676, 0.6976464429761185526, 4.494867301746904076 ) ) ;
#22063 = DIRECTION ( 'NONE',  ( -0.8660254037844415942, 0.4999999999999950040, -0.000000000000000000 ) ) ;
#22064 = CARTESIAN_POINT ( 'NONE',  ( 1.764879381686311977, -26.17053269682947203, 6.880147297696981745 ) ) ;
#22065 = ORIENTED_EDGE ( 'NONE', *, *, #1576, .T. ) ;
#22066 = CARTESIAN_POINT ( 'NONE',  ( 66.57766344320866381, 57.81227849924184881, -3.999802976169922974 ) ) ;
#22067 = CARTESIAN_POINT ( 'NONE',  ( -0.5298641067787194237, -26.88385662570251711, 7.778495531946298058 ) ) ;
#22068 = VECTOR ( 'NONE', #28631, 1000.000000000000000 ) ;
#22069 = ORIENTED_EDGE ( 'NONE', *, *, #2580, .F. ) ;
#22070 = VECTOR ( 'NONE', #29007, 1000.000000000000000 ) ;
#22071 = CARTESIAN_POINT ( 'NONE',  ( 88.35313037274487158, -0.8847049305017679055, 0.4761908919756944747 ) ) ;
#22072 = CARTESIAN_POINT ( 'NONE',  ( -73.13897352737927804, -2.605432823423965871, -9.755499191730667263 ) ) ;
#22073 = ORIENTED_EDGE ( 'NONE', *, *, #10098, .F. ) ;
#22074 = FACE_BOUND ( 'NONE', #20975, .T. ) ;
#22075 = LINE ( 'NONE', #25149, #40308 ) ;
#22076 = ORIENTED_EDGE ( 'NONE', *, *, #22140, .T. ) ;
#22077 = CARTESIAN_POINT ( 'NONE',  ( 22.64664158185920328, 4.505184941302465162, 3.155068566400609065 ) ) ;
#22078 = AXIS2_PLACEMENT_3D ( 'NONE', #9589, #145, #12479 ) ;
#22079 = CARTESIAN_POINT ( 'NONE',  ( 82.36730661685049881, 64.56044919582427610, -1.633153239555407144 ) ) ;
#22080 = CARTESIAN_POINT ( 'NONE',  ( 81.14259283377289478, 61.75830469257449096, 2.468641556982001273 ) ) ;
#22081 = CARTESIAN_POINT ( 'NONE',  ( 2.832967893104934465, -26.36411242075662642, 7.721096864323907738 ) ) ;
#22082 = ORIENTED_EDGE ( 'NONE', *, *, #24418, .F. ) ;
#22083 = CARTESIAN_POINT ( 'NONE',  ( 77.66280895473879298, 61.33468559051797087, -3.643081266330417289 ) ) ;
#22085 = CYLINDRICAL_SURFACE ( 'NONE', #11173, 3.399999999999999911 ) ;
#22084 = CARTESIAN_POINT ( 'NONE',  ( 3.921528935726882992, -32.26039213087532431, 7.781480525794719050 ) ) ;
#22086 = CARTESIAN_POINT ( 'NONE',  ( 15.93752674114121071, 10.76136407783234361, -2.654679014335209253 ) ) ;
#22087 = CARTESIAN_POINT ( 'NONE',  ( 80.79744990009727701, 64.13345242326634832, -3.486376426170565423 ) ) ;
#22088 = CARTESIAN_POINT ( 'NONE',  ( 78.44508438210816337, 62.63916802445883292, 3.816136337383057686 ) ) ;
#22089 = ORIENTED_EDGE ( 'NONE', *, *, #4058, .T. ) ;
#22090 = CARTESIAN_POINT ( 'NONE',  ( 4.749297472835600331, -31.28869828601962766, 7.695279973900954751 ) ) ;
#22091 = LINE ( 'NONE', #25576, #19052 ) ;
#22092 = CARTESIAN_POINT ( 'NONE',  ( 82.35726419014409316, 62.82676667106981938, 1.646077502935599401 ) ) ;
#22094 = CARTESIAN_POINT ( 'NONE',  ( -1.698345060826572883, -29.47668023426995632, 6.866852738645442322 ) ) ;
#22093 = CARTESIAN_POINT ( 'NONE',  ( 4.269313204158568631, -31.94703641790479764, 6.895394898881674450 ) ) ;
#22095 = CARTESIAN_POINT ( 'NONE',  ( 27.76889013493211067, -0.3210463222110187531, 6.029547961152755597 ) ) ;
#22096 = CARTESIAN_POINT ( 'NONE',  ( -1.404916813412772525, -31.18459841582754422, 6.880828092187095457 ) ) ;
#22097 = CARTESIAN_POINT ( 'NONE',  ( 25.22231346541800434, -5.090807757912027220, 2.500000000020063506 ) ) ;
#22098 = CARTESIAN_POINT ( 'NONE',  ( -63.39880662924651489, 35.63549842397610945, 6.795986594147001014 ) ) ;
#22099 = CARTESIAN_POINT ( 'NONE',  ( 4.679148373602942890, -31.38802211924678787, 7.780491323090170219 ) ) ;
#22100 = AXIS2_PLACEMENT_3D ( 'NONE', #8958, #25041, #37775 ) ;
#22101 = CARTESIAN_POINT ( 'NONE',  ( -70.92837670882107659, -39.37473357531882101, 0.000000000000000000 ) ) ;
#22102 = CIRCLE ( 'NONE', #16804, 3.499999999999999556 ) ;
#22103 = DIRECTION ( 'NONE',  ( 0.000000000000000000, 0.000000000000000000, 1.000000000000000000 ) ) ;
#22104 = DIRECTION ( 'NONE',  ( 0.8831583674551003460, -0.4690749385695657803, 0.000000000000000000 ) ) ;
#22105 = CARTESIAN_POINT ( 'NONE',  ( 35.70151715991190855, -1.358511810577603063, -5.583808527359176210 ) ) ;
#22106 = DIRECTION ( 'NONE',  ( -0.000000000000000000, -0.000000000000000000, 1.000000000000000000 ) ) ;
#22107 = CARTESIAN_POINT ( 'NONE',  ( 27.60344192425479193, 81.15229837709949834, -1.000000000000000000 ) ) ;
#22108 = CARTESIAN_POINT ( 'NONE',  ( 14.60824295769313963, -5.049561965150513920, -2.486367633875753658 ) ) ;
#22109 = DIRECTION ( 'NONE',  ( 1.000000000000000000, -0.000000000000000000, -0.000000000000000000 ) ) ;
#22110 = CARTESIAN_POINT ( 'NONE',  ( 2.083536916395903660, -32.94827280028442829, 6.969307238440508812 ) ) ;
#22111 = AXIS2_PLACEMENT_3D ( 'NONE', #4420, #20237, #16942 ) ;
#22112 = B_SPLINE_CURVE_WITH_KNOTS ( 'NONE', 3,
 ( #20477, #16260, #32144, #40612, #16853, #29435, #25945, #38479, #26352, #23258, #9318, #12417, #29235, #23060, #16647, #19359, #7399, #1043, #31930, #34473, #35625, #1247, #38884, #24988, #32338, #3737, #28832, #31168 ),
 .UNSPECIFIED., .F., .F.,
 ( 4, 2, 2, 1, 1, 1, 2, 2, 2, 2, 1, 1, 1, 2, 2, 2, 4 ),
 ( 0.000000000000000000, 0.1250000000000915101, 0.1875000000001351974, 0.2187500000001550426, 0.2343750000001629530, 0.2421875000001669220, 0.2460937500001669498, 0.2500000000001669775, 0.3750000000001321165, 0.4375000000001147415, 0.4687500000001080247, 0.4843750000001036948, 0.4921875000001015299, 0.4960937500001013634, 0.5000000000001012523, 0.7500000000000506262, 1.000000000000000000 ),
 .UNSPECIFIED. ) ;
#22113 = DIRECTION ( 'NONE',  ( -0.000000000000000000, -0.000000000000000000, 1.000000000000000000 ) ) ;
#22114 = CARTESIAN_POINT ( 'NONE',  ( 21.97379874220277429, -12.00982949064745320, 2.500000000000000444 ) ) ;
#22115 = EDGE_CURVE ( 'NONE', #17544, #22827, #8256, .T. ) ;
#22116 = DIRECTION ( 'NONE',  ( 1.000000000000000000, 0.000000000000000000, 0.000000000000000000 ) ) ;
#22117 = EDGE_LOOP ( 'NONE', ( #38097, #22426, #32557, #31080, #24579 ) ) ;
#22118 = FACE_BOUND ( 'NONE', #28227, .T. ) ;
#22119 = ADVANCED_FACE ( 'NONE', ( #19956 ), #29632, .F. ) ;
#22120 = CARTESIAN_POINT ( 'NONE',  ( 68.64726599134355922, 58.50818873767699557, -3.992679187475168145 ) ) ;
#22121 = VERTEX_POINT ( 'NONE', #25744 ) ;
#22122 = CARTESIAN_POINT ( 'NONE',  ( -0.9099111520310427803, -27.24534035165016377, 7.771081512783699630 ) ) ;
#22123 = DIRECTION ( 'NONE',  ( 1.000000000000000000, 0.000000000000000000, 0.000000000000000000 ) ) ;
#22124 = CARTESIAN_POINT ( 'NONE',  ( 23.73727407787542987, 2.939497050369670017, 3.908896929995592018 ) ) ;
#22125 = CARTESIAN_POINT ( 'NONE',  ( 5.020437716722687682, -28.46205448284394990, 6.863805608295730387 ) ) ;
#22126 = CARTESIAN_POINT ( 'NONE',  ( 3.514196955445712867, -26.57656972717544264, 6.867280401193707640 ) ) ;
#22127 = LINE ( 'NONE', #34701, #5441 ) ;
#22128 = ORIENTED_EDGE ( 'NONE', *, *, #7949, .T. ) ;
#22129 = CARTESIAN_POINT ( 'NONE',  ( 23.43597607405129679, 3.793424526424878263, 3.103042028786229700 ) ) ;
#22130 = DIRECTION ( 'NONE',  ( 1.000000000000000000, -0.000000000000000000, 0.000000000000000000 ) ) ;
#22131 = CARTESIAN_POINT ( 'NONE',  ( 0.4695943777967593880, -26.29347754267606874, 7.695279973900954751 ) ) ;
#22132 = VERTEX_POINT ( 'NONE', #16857 ) ;
#22133 = CARTESIAN_POINT ( 'NONE',  ( 79.88615925706736220, 62.68050235454665398, -3.612066323963901482 ) ) ;
#22134 = B_SPLINE_CURVE_WITH_KNOTS ( 'NONE', 3,
 ( #26222, #13850, #32404, #7467, #19634, #22927, #29694, #38347, #20024, #17123 ),
 .UNSPECIFIED., .F., .F.,
 ( 4, 3, 3, 4 ),
 ( 0.0002170292169044726665, 0.0002420761345915957668, 0.0002723302478206989560, 0.0002816811360866700248 ),
 .UNSPECIFIED. ) ;
#22135 =( BOUNDED_CURVE ( )  B_SPLINE_CURVE ( 3, ( #34424, #25134, #31115, #6808 ),
 .UNSPECIFIED., .F., .T. ) 
 B_SPLINE_CURVE_WITH_KNOTS ( ( 4, 4 ),
 ( 4.708531083176466403, 4.895802057644187855 ),
 .UNSPECIFIED. ) 
 CURVE ( )  GEOMETRIC_REPRESENTATION_ITEM ( )  RATIONAL_B_SPLINE_CURVE ( ( 1.000000000000000000, 0.9970795998553221295, 0.9970795998553221295, 1.000000000000000000 ) ) 
 REPRESENTATION_ITEM ( '' )  );
#22137 = DIRECTION ( 'NONE',  ( -1.000000000000000000, 0.000000000000000000, 0.000000000000000000 ) ) ;
#22136 = CARTESIAN_POINT ( 'NONE',  ( 24.12362351582647335, 0.5386221531753900837, 5.092127627954526226 ) ) ;
#22138 = AXIS2_PLACEMENT_3D ( 'NONE', #20122, #23423, #33097 ) ;
#22139 = CARTESIAN_POINT ( 'NONE',  ( 78.68583465488313777, 66.05536144407732024, -1.071687152255760944 ) ) ;
#22140 = EDGE_CURVE ( 'NONE', #38621, #10601, #35433, .T. ) ;
#22141 = CARTESIAN_POINT ( 'NONE',  ( 80.66846628934483476, 61.48471191768543775, 2.456741006817842354 ) ) ;
#22142 = DIRECTION ( 'NONE',  ( -0.000000000000000000, 1.000000000000000000, -0.000000000000000000 ) ) ;
#22143 = CARTESIAN_POINT ( 'NONE',  ( 2.893445099977317359, -32.75373604287706542, 7.721096864323904185 ) ) ;
#22144 = CARTESIAN_POINT ( 'NONE',  ( 22.31814515643556263, 6.191369071892208531, -1.397765879422002033 ) ) ;
#22145 = CARTESIAN_POINT ( 'NONE',  ( 1.356171688940976727, -33.05979889377250913, 7.501983001166816933 ) ) ;
#22146 = ORIENTED_EDGE ( 'NONE', *, *, #15774, .F. ) ;
#22147 = CARTESIAN_POINT ( 'NONE',  ( -76.51899586397401265, 9.210917537453957138, 9.782013801987098134 ) ) ;
#22148 = CARTESIAN_POINT ( 'NONE',  ( 36.12715512229904391, -3.661643169911928730, 5.700734919021059888 ) ) ;
#22149 = VERTEX_POINT ( 'NONE', #7203 ) ;
#22150 = EDGE_CURVE ( 'NONE', #31898, #9007, #35783, .T. ) ;
#22151 = CARTESIAN_POINT ( 'NONE',  ( -0.1539201161049026934, -32.53808085965915353, 7.754798119455333705 ) ) ;
#22152 = PLANE ( 'NONE',  #36774 ) ;
#22153 = CARTESIAN_POINT ( 'NONE',  ( 32.01236844922196667, -2.960126844666696844, -5.202702337194527793 ) ) ;
#22154 = CARTESIAN_POINT ( 'NONE',  ( 33.68512006240106871, -3.841534318799366687, -5.136340396096415795 ) ) ;
#22155 = DIRECTION ( 'NONE',  ( 1.000000000000000000, 0.000000000000000000, 0.000000000000000000 ) ) ;
#22156 = DIRECTION ( 'NONE',  ( 1.000000000000000000, 0.000000000000000000, 0.000000000000000000 ) ) ;
#22157 = CARTESIAN_POINT ( 'NONE',  ( 79.89212576172680258, 63.66154800590238949, 1.000000000000000000 ) ) ;
#22158 = CARTESIAN_POINT ( 'NONE',  ( -61.24591834330252027, 3.729367930467589076, -2.500000000000000000 ) ) ;
#22159 = DIRECTION ( 'NONE',  ( -1.000000000000000000, -0.000000000000000000, -0.000000000000000000 ) ) ;
#22160 = DIRECTION ( 'NONE',  ( 0.000000000000000000, 1.000000000000000000, 0.000000000000000000 ) ) ;
#22161 = CARTESIAN_POINT ( 'NONE',  ( 7.021324086407807030, -26.64985754041175525, 6.700000000000000178 ) ) ;
#22162 = CARTESIAN_POINT ( 'NONE',  ( 25.85639891750619412, 1.591965851834448165, -4.299200647184679092 ) ) ;
#22163 = CARTESIAN_POINT ( 'NONE',  ( 21.85643539959776760, 1.710603452083953179E-15, -2.500000000000000000 ) ) ;
#22164 = CYLINDRICAL_SURFACE ( 'NONE', #13068, 0.09010775117052947925 ) ;
#22165 = EDGE_CURVE ( 'NONE', #24264, #39701, #10945, .T. ) ;
#22166 = ORIENTED_EDGE ( 'NONE', *, *, #6804, .F. ) ;
#22168 = ORIENTED_EDGE ( 'NONE', *, *, #22706, .T. ) ;
#22167 = CIRCLE ( 'NONE', #33323, 4.075022672948151126 ) ;
#22169 = CARTESIAN_POINT ( 'NONE',  ( 67.11291460916432072, 58.16531518584054794, 3.996350724342222716 ) ) ;
#22170 = CARTESIAN_POINT ( 'NONE',  ( 34.76605832449826750, -3.465236551535387566, 5.619590712300242430 ) ) ;
#22171 = CIRCLE ( 'NONE', #5071, 3.000000000000003109 ) ;
#22172 = AXIS2_PLACEMENT_3D ( 'NONE', #12622, #30773, #25190 ) ;
#22173 = DIRECTION ( 'NONE',  ( 0.000000000000000000, 0.000000000000000000, 1.000000000000000000 ) ) ;
#22174 = CARTESIAN_POINT ( 'NONE',  ( 84.58609069645564205, 2.764543530557054041, -2.886136738505205912 ) ) ;
#22175 = CARTESIAN_POINT ( 'NONE',  ( 36.06197813380387629, -3.149146827136996674, -5.834741868653807728 ) ) ;
#22176 = ORIENTED_EDGE ( 'NONE', *, *, #18496, .T. ) ;
#22177 = CARTESIAN_POINT ( 'NONE',  ( 24.39369049594943206, 2.947980553390389780, 3.706541376397575860 ) ) ;
#22178 = CARTESIAN_POINT ( 'NONE',  ( 0.4918310210129015481, -32.74788313599579936, 6.894806418505344148 ) ) ;
#22179 = CARTESIAN_POINT ( 'NONE',  ( -51.01549048184568846, -38.28842912540938670, 6.800000000000000711 ) ) ;
#22180 = EDGE_CURVE ( 'NONE', #24066, #7569, #4989, .T. ) ;
#22181 = VERTEX_POINT ( 'NONE', #39353 ) ;
#22182 = CARTESIAN_POINT ( 'NONE',  ( 4.024979924976341827, -26.95962893812927774, 7.771081512783698741 ) ) ;
#22183 = B_SPLINE_SURFACE_WITH_KNOTS ( 'NONE', 5, 3, ( 
 ( #9051, #27591, #15848, #5977, #28405, #24293, #2913, #6183, #12551, #2711, #15233, #37653, #18942, #34208, #18517, #27786, #11719, #15646, #9455, #40341, #27994, #30698, #21831, #34617, #34410, #36856, #12134, #31307, #15028, #21425, #40142, #18726, #31103, #3331, #25122, #24501, #6392, #18105, #33999, #8640, #3129, #5564, #28193, #5775, #24921, #21215, #11924 ),
 ( #21, #33786, #22040, #37053, #12349, #15433, #40538, #37456, #31508, #2504, #8839, #18312, #30902, #24711, #37259, #9252, #21628, #425, #16843, #35220, #25331, #25729, #35422, #38672, #7387, #34823, #827, #12964, #25530, #213, #37866, #22653, #6598, #16638, #23051, #35616, #38075, #3933, #10271, #32327, #19348, #6991, #19144, #28617, #13359, #26140, #25934 ),
 ( #22256, #9669, #31709, #29024, #13568, #9876, #7190, #19558, #22450, #19943, #19750, #32134, #29222, #10471, #3525, #38467, #22849, #32522, #4125, #28823, #4321, #16449, #12753, #1034, #35019, #16049, #6794, #31917, #3728, #16252, #627, #13170, #38273, #10068, #1432, #39680, #29814, #39473, #38874, #26533, #5110, #13965, #11064, #11259, #1838, #26736, #7980 ),
 ( #23634, #39272, #17645, #30225, #29425, #14162, #10666, #26930, #1626, #17241, #39067, #36201, #8382, #4901, #8173, #20534, #35813, #7588, #17038, #20143, #10866, #33120, #11463, #24031, #2040, #14359, #23443, #17433, #23246, #14555, #20337, #23825, #36401, #27130, #20957, #32723, #30021, #4518, #7787, #20743, #1239, #36008, #33333, #29615, #32916, #36604, #33540 ),
 ( #5313, #4708, #13774, #26342, #14761, #12081, #24242, #34363, #40702, #25076, #14980, #21581, #27942, #21784, #21370, #24657, #11668, #5514, #18468, #15596, #2863, #34568, #15387, #39894, #27332, #36805, #40484, #31260, #18056, #12297, #34162, #11872, #37608, #24870, #37409, #6133, #27738, #21168, #2458, #28148, #18672, #27540, #17849, #33948, #30431, #33734, #24449 ),
 ( #2241, #5724, #30854, #2661, #15180, #6448, #38320, #22902, #9725, #3979, #3780, #31763, #32376, #16498, #28873, #25988, #19403, #19001, #34873, #35470, #19608, #37918, #16107, #19805, #38125, #7242, #16304, #19199, #10117, #38520, #679, #3579, #22306, #6845, #25379, #13621, #13220, #26195, #22095, #25786, #29075, #10325, #478, #13017, #4174, #16690, #31975 ),
 ( #9513, #13413, #29277, #25580, #22705, #28461, #32182, #1089, #882, #34670, #9927, #31561, #12808, #28672, #6649, #3384, #35273, #15900, #268, #22509, #35073, #7040, #20195, #35669, #33177, #32580, #30083, #32781, #11122, #2096, #1290, #11317, #20802, #1898, #10523, #23883, #10718, #39332, #20393, #32975, #23691, #20592, #17490, #4964, #4375, #38926, #13827 ),
 ( #36456, #23297, #14612, #4760, #23102, #23500, #14420, #8231, #5167, #16897, #36257, #35868, #7646, #38727, #7438, #17294, #29477, #26988, #33395, #17703, #4570, #1688, #8034, #26396, #39535, #30281, #19998, #17097, #14218, #29670, #1482, #14016, #29872, #26588, #39127, #10924, #36067, #7845, #26793, #40346, #8437, #24090, #36658, #15238, #379, #27388, #21636 ) ),
 .UNSPECIFIED., .F., .T., .F.,
 ( 6, 2, 6 ),
 ( 4, 1, 1, 1, 1, 1, 1, 1, 1, 1, 1, 1, 1, 1, 1, 1, 1, 1, 1, 1, 1, 1, 1, 1, 1, 1, 1, 1, 1, 1, 1, 1, 1, 1, 1, 1, 1, 1, 1, 1, 1, 1, 1, 1, 4 ),
 ( 0.000000000000000000, 0.5000000000000000000, 1.000000000000000000 ),
 ( -0.09263217477943377909, -0.08973741931757646395, -0.08732512309936206474, -0.08539528612479052594, -0.08394790839386186143, -0.08250053066293322468, -0.08105315293200456017, -0.07960577520107590954, -0.07815839747014724503, -0.07671101973921859440, -0.07478118276464705561, -0.07285134579007553068, -0.07092150881550399188, -0.06947413108457534126, -0.06802675335364669063, -0.06609691637907515183, -0.06416707940450361303, -0.06223724242993208117, -0.06030740545536053543, -0.05789510923714611540, -0.05548281301893168843, -0.05355297604436015657, -0.05162313906978862471, -0.04921084285157419774, -0.04631608738971689648, -0.04342133192785958135, -0.04052657646600228009, -0.03763182100414497189, -0.03521952478593055186, -0.03328968781135902000, -0.03184231008043036937, -0.03039493234950170833, -0.02846509537493017647, -0.02605279915671574950, -0.02364050293850132947, -0.02171066596392979067, -0.01978082898935825881, -0.01785099201478672001, -0.01592115504021518121, -0.01399131806564364588, -0.01157902184742922412, -0.008684266385571917657, -0.005789510923714612060, -0.002894755461857306030, 0.000000000000000000 ),
 .UNSPECIFIED. ) ;
#22184 = ORIENTED_EDGE ( 'NONE', *, *, #22623, .T. ) ;
#22185 = CARTESIAN_POINT ( 'NONE',  ( 79.10075812992880628, 65.22691190166780473, -3.061371641637540719 ) ) ;
#22186 = DIRECTION ( 'NONE',  ( 0.4690749385695657803, 0.8831583674551003460, 0.000000000000000000 ) ) ;
#22187 = CARTESIAN_POINT ( 'NONE',  ( 79.88758398535436811, 64.02175723273455787, 3.702313260098205827 ) ) ;
#22190 = ORIENTED_EDGE ( 'NONE', *, *, #3402, .T. ) ;
#22189 = ORIENTED_EDGE ( 'NONE', *, *, #12827, .F. ) ;
#22188 = CARTESIAN_POINT ( 'NONE',  ( 14.66504043345067032, 12.84305297963125270, 2.500000000000000000 ) ) ;
#22191 = AXIS2_PLACEMENT_3D ( 'NONE', #19350, #3334, #12755 ) ;
#22192 = DIRECTION ( 'NONE',  ( 0.000000000000000000, 1.000000000000000000, 0.000000000000000000 ) ) ;
#22193 = CARTESIAN_POINT ( 'NONE',  ( -0.5217032702065468319, -32.27405686018897768, 7.695279973900954751 ) ) ;
#22194 = CARTESIAN_POINT ( 'NONE',  ( -1.629504578382812818, -30.64779913458552230, 7.750000000000000888 ) ) ;
#22195 = EDGE_CURVE ( 'NONE', #30906, #25222, #23907, .T. ) ;
#22196 = EDGE_CURVE ( 'NONE', #35702, #16830, #40167, .T. ) ;
#22197 = CARTESIAN_POINT ( 'NONE',  ( -8.448748702180639114, -25.49307895267003587, 6.800000000000000711 ) ) ;
#22198 = VECTOR ( 'NONE', #35920, 1000.000000000000000 ) ;
#22199 = CARTESIAN_POINT ( 'NONE',  ( 21.99661976377250738, 5.574053075156116144, -3.114055112780370838 ) ) ;
#22200 = VERTEX_POINT ( 'NONE', #39150 ) ;
#22201 = FACE_OUTER_BOUND ( 'NONE', #15655, .T. ) ;
#22202 = VECTOR ( 'NONE', #33309, 1000.000000000000000 ) ;
#22203 = EDGE_CURVE ( 'NONE', #12529, #30676, #2400, .T. ) ;
#22204 = LINE ( 'NONE', #34770, #34585 ) ;
#22205 = CARTESIAN_POINT ( 'NONE',  ( -1.651405268677713423, -28.99939339395372784, 7.643333865083954848 ) ) ;
#22206 = CARTESIAN_POINT ( 'NONE',  ( -79.87304265776585055, -6.650848427980711186, -4.489763987400060330 ) ) ;
#22207 = LINE ( 'NONE', #28571, #39251 ) ;
#22208 = CARTESIAN_POINT ( 'NONE',  ( 80.90189697519826950, 63.80306449575954986, 3.509897338574981429 ) ) ;
#22209 = CARTESIAN_POINT ( 'NONE',  ( 84.21365554304541945, 2.879787869890822360, 1.939519519617897592 ) ) ;
#22210 = CARTESIAN_POINT ( 'NONE',  ( -0.5762289783111216313, -26.91154609728502578, 7.710604733652636433 ) ) ;
#22211 = ORIENTED_EDGE ( 'NONE', *, *, #16890, .T. ) ;
#22212 = LINE ( 'NONE', #31467, #13529 ) ;
#22213 = CARTESIAN_POINT ( 'NONE',  ( 24.90937036835209639, 3.542633436675763026, 0.6500615448964709442 ) ) ;
#22214 = CARTESIAN_POINT ( 'NONE',  ( 1.815543965490744593, -26.17188080386636528, 7.761597726988850532 ) ) ;
#22215 = DIRECTION ( 'NONE',  ( 0.7055275666422118341, 0.2567910337120383746, -0.6605219282605402364 ) ) ;
#22216 = CARTESIAN_POINT ( 'NONE',  ( 4.635447563317058872, -27.85370244579436516, 7.748216051605121280 ) ) ;
#22217 = CARTESIAN_POINT ( 'NONE',  ( 85.57702991149881200, 1.013049332619667009, 5.784095605458488443 ) ) ;
#22218 = CARTESIAN_POINT ( 'NONE',  ( 20.42385195123408081, 3.665137036896844336, 3.394034068352853151 ) ) ;
#22219 = VECTOR ( 'NONE', #39679, 1000.000000000000000 ) ;
#22220 = CARTESIAN_POINT ( 'NONE',  ( 87.15505355144220800, 0.4610318193416703680, -5.246243280819175681 ) ) ;
#22221 = ORIENTED_EDGE ( 'NONE', *, *, #12981, .T. ) ;
#22223 = CARTESIAN_POINT ( 'NONE',  ( -61.57369240569498459, -49.47615685354814019, 3.769463484964754141 ) ) ;
#22222 = CARTESIAN_POINT ( 'NONE',  ( 81.15583125883576088, 62.51952284974313301, -3.108243619504619915 ) ) ;
#22224 = AXIS2_PLACEMENT_3D ( 'NONE', #16181, #3055, #558 ) ;
#22225 = CARTESIAN_POINT ( 'NONE',  ( -70.73088139374260663, -45.62685287453590632, 9.998512938616805457 ) ) ;
#22226 = CIRCLE ( 'NONE', #1856, 0.1000000000000028644 ) ;
#22227 = AXIS2_PLACEMENT_3D ( 'NONE', #8316, #20891, #30372 ) ;
#22228 = ORIENTED_EDGE ( 'NONE', *, *, #25527, .T. ) ;
#22229 = CARTESIAN_POINT ( 'NONE',  ( -1.638866927195242296, -28.93003665516189926, 7.785868773668302545 ) ) ;
#22230 = EDGE_CURVE ( 'NONE', #25100, #4684, #2351, .T. ) ;
#22231 = EDGE_LOOP ( 'NONE', ( #3103, #353, #31794, #39619, #34016 ) ) ;
#22232 = CARTESIAN_POINT ( 'NONE',  ( 0.7201709579117279159, -51.60714625320436255, -6.000000000000000000 ) ) ;
#22234 = ORIENTED_EDGE ( 'NONE', *, *, #18114, .F. ) ;
#22233 = ORIENTED_EDGE ( 'NONE', *, *, #38073, .F. ) ;
#22235 = CARTESIAN_POINT ( 'NONE',  ( 78.99368969759478887, 65.72941799158938636, -2.506402126386322760 ) ) ;
#22236 = B_SPLINE_CURVE_WITH_KNOTS ( 'NONE', 3,
 ( #24724, #2932, #31117, #27803, #5996, #37279 ),
 .UNSPECIFIED., .F., .F.,
 ( 4, 2, 4 ),
 ( 0.000000000000000000, 0.0004173165775082530657, 0.0008346331550165061314 ),
 .UNSPECIFIED. ) ;
#22237 = CARTESIAN_POINT ( 'NONE',  ( 36.65031935333231417, -3.107300908937615347, 5.926566745047386675 ) ) ;
#22239 = CARTESIAN_POINT ( 'NONE',  ( 36.60019281065275720, -1.851694985322541287, 5.780171978738543714 ) ) ;
#22238 = CARTESIAN_POINT ( 'NONE',  ( 22.26980982591663505, 1.689402514127164912, 5.821894515090187738 ) ) ;
#22241 = ORIENTED_EDGE ( 'NONE', *, *, #13990, .F. ) ;
#22240 = ORIENTED_EDGE ( 'NONE', *, *, #30022, .T. ) ;
#22242 = ADVANCED_FACE ( 'NONE', ( #37289 ), #15262, .T. ) ;
#22243 = EDGE_CURVE ( 'NONE', #6003, #17955, #12381, .T. ) ;
#22244 = CARTESIAN_POINT ( 'NONE',  ( 2.868207633511080434, -32.86935470785505231, 6.894806418505347700 ) ) ;
#22245 = VECTOR ( 'NONE', #26480, 1000.000000000000000 ) ;
#22247 = FACE_OUTER_BOUND ( 'NONE', #37592, .T. ) ;
#22246 = DIRECTION ( 'NONE',  ( 0.000000000000000000, 1.000000000000000000, 0.000000000000000000 ) ) ;
#22248 = CARTESIAN_POINT ( 'NONE',  ( -30.44874870218064089, -26.64985754041175525, 6.800000000000000711 ) ) ;
#22249 = CARTESIAN_POINT ( 'NONE',  ( 0.5490648462263181262, -26.27994216516969672, 7.785096263473212375 ) ) ;
#22250 = CARTESIAN_POINT ( 'NONE',  ( 70.63497465855112978, 60.23961165191135336, 3.862811858476220550 ) ) ;
#22251 = EDGE_LOOP ( 'NONE', ( #35638, #9076, #32, #20316 ) ) ;
#22252 = CARTESIAN_POINT ( 'NONE',  ( 21.84320482927419604, 4.475403957759267470, -4.050769160178117723 ) ) ;
#22253 = ORIENTED_EDGE ( 'NONE', *, *, #40093, .T. ) ;
#22254 = EDGE_CURVE ( 'NONE', #25957, #9702, #9697, .T. ) ;
#22255 = ORIENTED_EDGE ( 'NONE', *, *, #1161, .T. ) ;
#22256 = CARTESIAN_POINT ( 'NONE',  ( 21.85643539959774273, 9.214175136349357587, -0.8338435668127727185 ) ) ;
#22257 = CARTESIAN_POINT ( 'NONE',  ( 1.121324086407811338, -24.55319635012989110, 6.700000000000000178 ) ) ;
#22258 = CARTESIAN_POINT ( 'NONE',  ( 78.89436432227896034, 66.15509128278824846, 1.313329331391815513 ) ) ;
#22259 = CARTESIAN_POINT ( 'NONE',  ( 85.23697547898807159, 2.562304445728192714, -3.499295437968926947 ) ) ;
#22260 = ORIENTED_EDGE ( 'NONE', *, *, #36036, .T. ) ;
#22261 = EDGE_CURVE ( 'NONE', #18339, #17250, #34031, .T. ) ;
#22262 = CARTESIAN_POINT ( 'NONE',  ( 0.5701619414054610591, -32.77657804911444117, 7.712764235869103757 ) ) ;
#22263 = CARTESIAN_POINT ( 'NONE',  ( 18.24487163080560492, -2.878841870252593527, 3.053951490511794375 ) ) ;
#22264 = CARTESIAN_POINT ( 'NONE',  ( 36.19390568488644533, -2.232540992349622222, -5.855332353680082313 ) ) ;
#22265 = CARTESIAN_POINT ( 'NONE',  ( 5.100230395877511924, -29.53676087646269366, 7.670860738520326905 ) ) ;
#22266 = DIRECTION ( 'NONE',  ( 1.000000000000000000, 0.000000000000000000, 0.000000000000000000 ) ) ;
#22267 = ORIENTED_EDGE ( 'NONE', *, *, #29916, .T. ) ;
#22268 = DIRECTION ( 'NONE',  ( -0.000000000000000000, -0.000000000000000000, -1.000000000000000000 ) ) ;
#22269 = CARTESIAN_POINT ( 'NONE',  ( -1.299983928880091399, -31.16922869443764910, 7.761597726988848756 ) ) ;
#22270 = CARTESIAN_POINT ( 'NONE',  ( 30.76274491791073018, -3.760333558979258139, 4.555209097832164211 ) ) ;
#22271 = ORIENTED_EDGE ( 'NONE', *, *, #116, .F. ) ;
#22272 = CARTESIAN_POINT ( 'NONE',  ( 33.45655213939275541, -3.830548352551304880, 5.092536695668412605 ) ) ;
#22273 = AXIS2_PLACEMENT_3D ( 'NONE', #12405, #27639, #9512 ) ;
#22274 = CYLINDRICAL_SURFACE ( 'NONE', #30396, 0.1000000000000028644 ) ;
#22275 = CARTESIAN_POINT ( 'NONE',  ( 66.42000668879835246, 57.79655248154868730, -4.000000000000018652 ) ) ;
#22276 = ADVANCED_FACE ( 'NONE', ( #14637 ), #34238, .F. ) ;
#22277 = EDGE_LOOP ( 'NONE', ( #15921, #32348, #7152, #4880 ) ) ;
#22278 = CARTESIAN_POINT ( 'NONE',  ( 87.80056509578477630, -0.2640373850900027408, -3.668630654083185672 ) ) ;
#22279 = CARTESIAN_POINT ( 'NONE',  ( -80.92837670882107659, 2.429809908903242555, -12.50000000000000000 ) ) ;
#22280 = LINE ( 'NONE', #454, #16264 ) ;
#22281 = ORIENTED_EDGE ( 'NONE', *, *, #17136, .T. ) ;
#22282 = DIRECTION ( 'NONE',  ( 0.000000000000000000, 0.000000000000000000, 1.000000000000000000 ) ) ;
#22283 = SURFACE_STYLE_FILL_AREA ( #9704 ) ;
#22284 = ORIENTED_EDGE ( 'NONE', *, *, #16004, .T. ) ;
#22285 = CARTESIAN_POINT ( 'NONE',  ( 22.04813532460007863, 5.340643346204053898, 3.227846874785398779 ) ) ;
#22286 = CARTESIAN_POINT ( 'NONE',  ( 82.16824647341034904, 62.22308028923542622, -1.246975333547555742 ) ) ;
#22287 = CIRCLE ( 'NONE', #40655, 0.1000000000000028644 ) ;
#22288 = CARTESIAN_POINT ( 'NONE',  ( 81.13710691025121946, 61.43629694585948187, 1.911132874451712205 ) ) ;
#22289 = ORIENTED_EDGE ( 'NONE', *, *, #21151, .F. ) ;
#22290 = CARTESIAN_POINT ( 'NONE',  ( 76.54556538389314824, 62.22002718612351657, -3.872369636030850160 ) ) ;
#22292 = FACE_OUTER_BOUND ( 'NONE', #16371, .T. ) ;
#22291 = CARTESIAN_POINT ( 'NONE',  ( 3.894751441679935144, -32.27749053463322326, 7.785593909369612931 ) ) ;
#22293 = CARTESIAN_POINT ( 'NONE',  ( 15.30597500999765259, 11.49007520356607692, -2.585737325345484727 ) ) ;
#22294 = CARTESIAN_POINT ( 'NONE',  ( 81.03825699591064335, 63.48946937969521542, -3.448515284080294840 ) ) ;
#22295 = CARTESIAN_POINT ( 'NONE',  ( 77.10371989074782562, 62.50202019409571363, 3.856837490694489556 ) ) ;
#22296 = VERTEX_POINT ( 'NONE', #40173 ) ;
#22297 = ADVANCED_FACE ( 'NONE', ( #31129 ), #24950, .T. ) ;
#22298 = EDGE_CURVE ( 'NONE', #27620, #18445, #11543, .T. ) ;
#22299 = CARTESIAN_POINT ( 'NONE',  ( 4.738207753463742122, -31.30822356001046458, 7.635761828346574021 ) ) ;
#22300 = ADVANCED_FACE ( 'NONE', ( #19583, #37680 ), #7018, .T. ) ;
#22301 = CIRCLE ( 'NONE', #4538, 0.1000000000000028644 ) ;
#22302 = DIRECTION ( 'NONE',  ( 0.000000000000000000, 0.000000000000000000, -1.000000000000000000 ) ) ;
#22303 = CARTESIAN_POINT ( 'NONE',  ( 78.68971998042104588, 66.05812159354533719, 1.027726681410877863 ) ) ;
#22305 = CARTESIAN_POINT ( 'NONE',  ( 18.79220209723194301, 6.725183318188751258, 3.484773800353550222 ) ) ;
#22304 = CARTESIAN_POINT ( 'NONE',  ( 4.255709282003521388, -31.96165711204241333, 6.931070083220559397 ) ) ;
#22306 = CARTESIAN_POINT ( 'NONE',  ( 29.52151182519568096, -2.704869923190903691, 5.373754524306347591 ) ) ;
#22307 = CARTESIAN_POINT ( 'NONE',  ( -1.411982544752807600, -31.17091005906851109, 6.895394898881667345 ) ) ;
#22308 = CARTESIAN_POINT ( 'NONE',  ( -1.788343858407013265, -29.54202564690695354, 7.781480525794717273 ) ) ;
#22309 = CARTESIAN_POINT ( 'NONE',  ( -62.81463675898083210, 36.67811266762163314, 4.600311178732271244 ) ) ;
#22310 = DIRECTION ( 'NONE',  ( -0.000000000000000000, -0.000000000000000000, -1.000000000000000000 ) ) ;
#22311 = ORIENTED_EDGE ( 'NONE', *, *, #20587, .T. ) ;
#22312 = CARTESIAN_POINT ( 'NONE',  ( 11.29080664838498826, -10.90558813203967148, -2.500000000000000000 ) ) ;
#22313 = CYLINDRICAL_SURFACE ( 'NONE', #30863, 3.000000000000000444 ) ;
#22314 = CARTESIAN_POINT ( 'NONE',  ( 34.77014988848376476, -3.601456801931015139, -5.565767284829528094 ) ) ;
#22315 = CARTESIAN_POINT ( 'NONE',  ( -69.42837670882107659, -47.11702805680359063, 9.886859966642603581 ) ) ;
#22316 = CARTESIAN_POINT ( 'NONE',  ( -0.9794948794710025552, -31.66235005623412135, 7.757178535559534183 ) ) ;
#22317 = CARTESIAN_POINT ( 'NONE',  ( -63.05049812975200041, 38.43447230638179235, 4.010972415401512059 ) ) ;
#22318 = CARTESIAN_POINT ( 'NONE',  ( -36.87867591359218977, -26.64985754041175525, 6.700000000000000178 ) ) ;
#22319 = CARTESIAN_POINT ( 'NONE',  ( -81.75358215887496272, 10.46790825574969119, 1.500190250375194712 ) ) ;
#22320 = B_SPLINE_CURVE_WITH_KNOTS ( 'NONE', 3,
 ( #23024, #26509, #798, #20309, #38442, #35590, #10246, #22825, #1006, #13541, #26114, #38645, #10443, #7361, #40069, #20928, #27305, #33922, #5286, #2430, #18238, #5698, #2213, #39653, #14950, #23800, #30623, #14531, #30828, #39445, #5488 ),
 .UNSPECIFIED., .F., .F.,
 ( 4, 3, 3, 3, 3, 3, 3, 3, 3, 3, 4 ),
 ( 0.000000000000000000, 2.999644130997945415E-05, 6.002588995695307074E-05, 8.960886084588327871E-05, 0.0001190604700446532943, 0.0001489538463052769788, 0.0001796139255494003486, 0.0002109707048517106293, 0.0002426195318110385007, 0.0002740640997890078645, 0.0002849778069099876180 ),
 .UNSPECIFIED. ) ;
#22321 = DIRECTION ( 'NONE',  ( -0.000000000000000000, -0.000000000000000000, 1.000000000000000000 ) ) ;
#22322 = VECTOR ( 'NONE', #33407, 1000.000000000000000 ) ;
#22323 = CARTESIAN_POINT ( 'NONE',  ( 1.720540564825900454, -33.91097937392895290, 7.013842709614101167 ) ) ;
#22324 = ORIENTED_EDGE ( 'NONE', *, *, #14588, .T. ) ;
#22325 = ORIENTED_EDGE ( 'NONE', *, *, #22395, .F. ) ;
#22326 = CARTESIAN_POINT ( 'NONE',  ( 3.300000000000000711, 0.000000000000000000, -4.250000000000000000 ) ) ;
#22327 = CARTESIAN_POINT ( 'NONE',  ( 68.13924211849639789, 58.08649371134929140, -3.978477839347963840 ) ) ;
#22328 = CARTESIAN_POINT ( 'NONE',  ( 2.957564255009486942, -26.30349574841345728, 6.870737987065013819 ) ) ;
#22329 = ORIENTED_EDGE ( 'NONE', *, *, #22180, .T. ) ;
#22330 = CARTESIAN_POINT ( 'NONE',  ( -0.9261155348575771384, -27.27773970951159654, 7.784725160561909441 ) ) ;
#22331 = CARTESIAN_POINT ( 'NONE',  ( -1.599636697286329401, -28.40380913581408606, 7.720710062488896241 ) ) ;
#22332 = CARTESIAN_POINT ( 'NONE',  ( 22.63675764000105772, 3.280949574944325153, 4.200075021517235108 ) ) ;
#22333 = CARTESIAN_POINT ( 'NONE',  ( -1.428174809773816500, -28.23871018788941356, 6.887945620086119547 ) ) ;
#22334 = CARTESIAN_POINT ( 'NONE',  ( 1.207759159255195724, -26.20579572742846608, 7.774064877406527074 ) ) ;
#22335 = DIRECTION ( 'NONE',  ( -0.6502177225477943079, 0.3754033771448263557, 0.6605219282605377940 ) ) ;
#22336 = ORIENTED_EDGE ( 'NONE', *, *, #34294, .T. ) ;
#22337 = CARTESIAN_POINT ( 'NONE',  ( 21.99022176547038399, 5.605367161166800116, 3.096869486298271745 ) ) ;
#22338 = DIRECTION ( 'NONE',  ( -0.7660444431189813441, 0.6427876096865353661, -0.000000000000000000 ) ) ;
#22339 = CARTESIAN_POINT ( 'NONE',  ( 78.73750597996149736, 66.05139304066524630, 1.520709669156477428 ) ) ;
#22340 = ORIENTED_EDGE ( 'NONE', *, *, #10590, .F. ) ;
#22341 = CARTESIAN_POINT ( 'NONE',  ( -70.92837670882107659, -56.35932253828836025, 0.000000000000000000 ) ) ;
#22342 = EDGE_LOOP ( 'NONE', ( #4442, #6528, #12993, #11666 ) ) ;
#22343 = CARTESIAN_POINT ( 'NONE',  ( 80.30053069885687478, 62.24503436470105555, -3.340572457511948201 ) ) ;
#22345 = CARTESIAN_POINT ( 'NONE',  ( -1.670147819023525271, -30.01655550963544172, 6.868387053540520704 ) ) ;
#22344 = CARTESIAN_POINT ( 'NONE',  ( 22.01703001042701757, 0.2566429920367864215, 7.603351845833338452 ) ) ;
#22346 = CARTESIAN_POINT ( 'NONE',  ( 79.50049935622257635, 66.06919348782189161, -2.170472567296708011 ) ) ;
#22347 = CARTESIAN_POINT ( 'NONE',  ( 78.44523713320049296, 65.65863411530537519, 2.218931858625904585 ) ) ;
#22348 = VECTOR ( 'NONE', #30964, 1000.000000000000114 ) ;
#22349 = EDGE_CURVE ( 'NONE', #18413, #33687, #9484, .T. ) ;
#22350 = ADVANCED_FACE ( 'NONE', ( #25761 ), #18972, .F. ) ;
#22351 = CARTESIAN_POINT ( 'NONE',  ( 81.16957891225079891, 61.30398062001319914, 1.000000000000000000 ) ) ;
#22352 = CARTESIAN_POINT ( 'NONE',  ( -64.08758708074093136, 41.34485010641581937, 2.999999996672334746 ) ) ;
#22353 = CARTESIAN_POINT ( 'NONE',  ( 24.65869693034278143, -1.551691026114866201, -6.728867248637652843 ) ) ;
#22354 = DIRECTION ( 'NONE',  ( 0.000000000000000000, 0.000000000000000000, 1.000000000000000000 ) ) ;
#22355 = ORIENTED_EDGE ( 'NONE', *, *, #24253, .F. ) ;
#22356 = CARTESIAN_POINT ( 'NONE',  ( -76.30046984573570512, 10.53876514546700527, 8.436514736823731653 ) ) ;
#22357 = CARTESIAN_POINT ( 'NONE',  ( 27.44646592037410215, 0.9065689399580380003, -4.490082820797807628 ) ) ;
#22358 = ORIENTED_EDGE ( 'NONE', *, *, #40558, .F. ) ;
#22359 = CARTESIAN_POINT ( 'NONE',  ( 0.6185823884176052667, -26.24155567332487493, 7.754798119455333705 ) ) ;
#22360 = CARTESIAN_POINT ( 'NONE',  ( -80.91149519099745646, 11.45826392489275136, -0.9973769203057932797 ) ) ;
#22361 = CIRCLE ( 'NONE', #20350, 12.73502530973474300 ) ;
#22362 = CARTESIAN_POINT ( 'NONE',  ( 30.73690320840939094, -3.644613918395323893, -4.722495812001631599 ) ) ;
#22363 = CARTESIAN_POINT ( 'NONE',  ( 32.06850821402472462, 0.2517114437988486331, -4.728941223353197998 ) ) ;
#22364 = PLANE ( 'NONE',  #40014 ) ;
#22365 = CARTESIAN_POINT ( 'NONE',  ( 15.85770990068897568, 10.71461798967161627, 2.668183247020202042 ) ) ;
#22366 = CARTESIAN_POINT ( 'NONE',  ( 5.200252094213874798, -29.60101030711846448, 6.894806418505347700 ) ) ;
#22367 = CARTESIAN_POINT ( 'NONE',  ( -0.9006701161811203615, -27.22837715677322379, 7.754798119455333705 ) ) ;
#22368 = CARTESIAN_POINT ( 'NONE',  ( 1.700390093233090871, -29.56993018339339940, 7.750000000000000888 ) ) ;
#22369 = PLANE ( 'NONE',  #35542 ) ;
#22370 = CARTESIAN_POINT ( 'NONE',  ( 29.68316414800138858, 1.144177792258728843, -4.265623084207747162 ) ) ;
#22371 = DIRECTION ( 'NONE',  ( 1.000000000000000000, 0.000000000000000000, 0.000000000000000000 ) ) ;
#22372 = ORIENTED_EDGE ( 'NONE', *, *, #15419, .T. ) ;
#22373 = B_SPLINE_CURVE_WITH_KNOTS ( 'NONE', 3,
 ( #9949, #32603, #3605, #19427, #34899, #35494, #1116, #13648, #16131, #7263, #29503, #28695, #38752, #7465, #26220, #37944, #10546, #22532, #26015, #7063, #4005, #506, #31998, #13041 ),
 .UNSPECIFIED., .F., .F.,
 ( 4, 2, 2, 2, 2, 2, 2, 2, 2, 2, 2, 4 ),
 ( 0.000000000000000000, 0.1249999999999756028, 0.1874999999999667211, 0.2187499999999662770, 0.2499999999999658051, 0.3749999999999674150, 0.3906249999999655831, 0.4062499999999636957, 0.4374999999999693578, 0.4999999999999727995, 0.7499999999999863443, 1.000000000000000000 ),
 .UNSPECIFIED. ) ;
#22374 = CARTESIAN_POINT ( 'NONE',  ( 66.72049918463439155, 57.87600310258397940, 3.999713739232678034 ) ) ;
#22375 = EDGE_CURVE ( 'NONE', #8526, #13304, #1647, .T. ) ;
#22376 = AXIS2_PLACEMENT_3D ( 'NONE', #12693, #27724, #8774 ) ;
#22377 = DIRECTION ( 'NONE',  ( -0.3420201433256725987, 0.9396926207859068736, -0.000000000000000000 ) ) ;
#22378 = CARTESIAN_POINT ( 'NONE',  ( 85.17963886742116131, 2.035184340541872139, -4.783483324554544502 ) ) ;
#22379 =( BOUNDED_CURVE ( )  B_SPLINE_CURVE ( 3, ( #13780, #26348, #38881, #10673 ),
 .UNSPECIFIED., .F., .T. ) 
 B_SPLINE_CURVE_WITH_KNOTS ( ( 4, 4 ),
 ( 4.748221474220560623, 4.941946782021394924 ),
 .UNSPECIFIED. ) 
 CURVE ( )  GEOMETRIC_REPRESENTATION_ITEM ( )  RATIONAL_B_SPLINE_CURVE ( ( 1.000000000000000000, 0.9968749865767494445, 0.9968749865767494445, 1.000000000000000000 ) ) 
 REPRESENTATION_ITEM ( '' )  );
#22380 = VERTEX_POINT ( 'NONE', #16278 ) ;
#22381 = CARTESIAN_POINT ( 'NONE',  ( 24.37965766804015288, 2.942655792175109308, 3.717632330914962147 ) ) ;
#22382 = DIRECTION ( 'NONE',  ( 1.000000000000000000, 0.000000000000000000, 0.000000000000000000 ) ) ;
#22383 = DIRECTION ( 'NONE',  ( 0.000000000000000000, 0.000000000000000000, 1.000000000000000000 ) ) ;
#22384 = ORIENTED_EDGE ( 'NONE', *, *, #36534, .T. ) ;
#22385 = CARTESIAN_POINT ( 'NONE',  ( 3.953335785500533994, -26.89871648206090171, 7.773839561854631874 ) ) ;
#22386 = EDGE_CURVE ( 'NONE', #35661, #6366, #2839, .T. ) ;
#22387 = VECTOR ( 'NONE', #31345, 1000.000000000000000 ) ;
#22388 = VERTEX_POINT ( 'NONE', #15674 ) ;
#22389 = CARTESIAN_POINT ( 'NONE',  ( 79.85475324883658743, 64.00275885990843960, -3.706996517075250352 ) ) ;
#22390 = DIRECTION ( 'NONE',  ( -0.000000000000000000, -1.000000000000000000, -0.000000000000000000 ) ) ;
#22391 = CARTESIAN_POINT ( 'NONE',  ( 78.55684871931622126, 65.96378271911972035, 1.386845825021860490 ) ) ;
#22393 = ORIENTED_EDGE ( 'NONE', *, *, #5642, .F. ) ;
#22392 = DIRECTION ( 'NONE',  ( -0.000000000000000000, -0.000000000000000000, 1.000000000000000000 ) ) ;
#22394 = CARTESIAN_POINT ( 'NONE',  ( 0.01625745047043060387, -26.51765787828566445, 7.784725160561910329 ) ) ;
#22395 = EDGE_CURVE ( 'NONE', #28485, #34557, #27932, .T. ) ;
#22396 = DIRECTION ( 'NONE',  ( 0.000000000000000000, 0.000000000000000000, 1.000000000000000000 ) ) ;
#22397 = CARTESIAN_POINT ( 'NONE',  ( 3.433582406314023228, -26.52919928344892142, 7.643192810543816940 ) ) ;
#22398 = CARTESIAN_POINT ( 'NONE',  ( 21.85643539959778536, -9.383538770078029501, -13.42257110913290141 ) ) ;
#22399 = CARTESIAN_POINT ( 'NONE',  ( 22.19935042935221858, 5.213326102501693704, -3.111963524547389781 ) ) ;
#22400 = DIRECTION ( 'NONE',  ( 0.000000000000000000, 0.000000000000000000, -1.000000000000000000 ) ) ;
#22401 = CARTESIAN_POINT ( 'NONE',  ( -1.751698146652124866, -30.14706689514045479, 6.894806418505347700 ) ) ;
#22402 = CARTESIAN_POINT ( 'NONE',  ( -1.565604181971737008, -30.54008291720758095, 7.386948897581447682 ) ) ;
#22403 = CARTESIAN_POINT ( 'NONE',  ( -35.07867591359219972, -26.64985754041175525, 6.700000000000000178 ) ) ;
#22404 = CARTESIAN_POINT ( 'NONE',  ( 1.700390093233090871, -29.56993018339339940, 7.800000000000000711 ) ) ;
#22405 = DIRECTION ( 'NONE',  ( -0.000000000000000000, -0.000000000000000000, -1.000000000000000000 ) ) ;
#22406 = CARTESIAN_POINT ( 'NONE',  ( 81.31240362382359876, 61.49079461182719797, 1.766895996212472175 ) ) ;
#22407 = CARTESIAN_POINT ( 'NONE',  ( 88.05006142693602555, -2.316660831613085225, -1.868938639203592489 ) ) ;
#22408 = CARTESIAN_POINT ( 'NONE',  ( -0.5714989174472279165, -26.90750265890564208, 7.730015791551954507 ) ) ;
#22409 = VERTEX_POINT ( 'NONE', #35447 ) ;
#22410 = CARTESIAN_POINT ( 'NONE',  ( -1.332552448688619329, -27.82589715396020225, 7.762796336881261361 ) ) ;
#22411 = DIRECTION ( 'NONE',  ( 0.000000000000000000, 0.000000000000000000, 1.000000000000000000 ) ) ;
#22412 = CARTESIAN_POINT ( 'NONE',  ( 1.770820908965922591, -26.17064486340278862, 7.784476445165072533 ) ) ;
#22413 = AXIS2_PLACEMENT_3D ( 'NONE', #27604, #8654, #14621 ) ;
#22414 = CARTESIAN_POINT ( 'NONE',  ( 24.75830837035764276, 3.019210359990082804, 3.350572556515618583 ) ) ;
#22415 = LINE ( 'NONE', #25895, #32683 ) ;
#22416 = CARTESIAN_POINT ( 'NONE',  ( -0.1576164094376339420, -32.53604074034053895, 7.750000000000000888 ) ) ;
#22417 = CARTESIAN_POINT ( 'NONE',  ( 37.04329737603605111, -2.892586564141972350, 5.987900469699707351 ) ) ;
#22418 = DIRECTION ( 'NONE',  ( 1.000000000000000000, 0.000000000000000000, 0.000000000000000000 ) ) ;
#22419 = CARTESIAN_POINT ( 'NONE',  ( 85.49511565994269802, 2.325552844478905090, -3.343772400554256397 ) ) ;
#22420 = VERTEX_POINT ( 'NONE', #858 ) ;
#22422 = CARTESIAN_POINT ( 'NONE',  ( 14.77500745536057813, -5.175466302041957789, 2.500000552286355759 ) ) ;
#22421 = CARTESIAN_POINT ( 'NONE',  ( 81.26478070948648735, 61.47323240028521241, -1.804401104814721712 ) ) ;
#22423 = EDGE_CURVE ( 'NONE', #35515, #15871, #20507, .T. ) ;
#22424 = CARTESIAN_POINT ( 'NONE',  ( -69.42837670882106238, -47.01908264895750023, 9.886859966642600028 ) ) ;
#22425 = DIRECTION ( 'NONE',  ( -0.000000000000000000, -0.000000000000000000, 1.000000000000000000 ) ) ;
#22426 = ORIENTED_EDGE ( 'NONE', *, *, #32993, .T. ) ;
#22427 = EDGE_CURVE ( 'NONE', #19656, #32235, #26565, .T. ) ;
#22428 = VECTOR ( 'NONE', #29934, 1000.000000000000000 ) ;
#22429 = CARTESIAN_POINT ( 'NONE',  ( -54.01549048184568846, -30.38627270959228710, -4.152976064860135708 ) ) ;
#22430 = VERTEX_POINT ( 'NONE', #10696 ) ;
#22431 = CARTESIAN_POINT ( 'NONE',  ( -76.50596395675130168, -5.795592924334072471, 8.309263729044971569 ) ) ;
#22432 = ORIENTED_EDGE ( 'NONE', *, *, #19621, .T. ) ;
#22433 = CARTESIAN_POINT ( 'NONE',  ( 81.10356443252386782, 61.32192396066504614, -1.621665796799206305 ) ) ;
#22434 = DIRECTION ( 'NONE',  ( 1.000000000000000000, 0.000000000000000000, 0.000000000000000000 ) ) ;
#22435 = CARTESIAN_POINT ( 'NONE',  ( 22.24790050656625695, 1.172224622543360129, 6.341858785536460985 ) ) ;
#22436 = EDGE_LOOP ( 'NONE', ( #19183, #14911, #3958, #4689 ) ) ;
#22437 = CARTESIAN_POINT ( 'NONE',  ( 81.16729622508351838, 61.30314466175458676, -1.045986116561645529 ) ) ;
#22438 = DIRECTION ( 'NONE',  ( -0.000000000000000000, -0.000000000000000000, -1.000000000000000000 ) ) ;
#22439 = AXIS2_PLACEMENT_3D ( 'NONE', #28380, #21804, #21602 ) ;
#22440 = CARTESIAN_POINT ( 'NONE',  ( 4.731166529110806707, -28.02900214338483664, 6.887945620086118659 ) ) ;
#22441 = EDGE_CURVE ( 'NONE', #14269, #39459, #33151, .T. ) ;
#22443 = CARTESIAN_POINT ( 'NONE',  ( 86.40625215706664619, 1.302121085762450114, 4.853768006845460725 ) ) ;
#22442 = CARTESIAN_POINT ( 'NONE',  ( -57.80362650821757597, 30.11637991209972753, -4.211916349762224954 ) ) ;
#22444 = CARTESIAN_POINT ( 'NONE',  ( -16.24874870218063450, -26.64985754041175525, 6.700000000000000178 ) ) ;
#22445 = CARTESIAN_POINT ( 'NONE',  ( 0.5333944940907733301, -26.28204871958340050, 7.781480525794718162 ) ) ;
#22446 = CARTESIAN_POINT ( 'NONE',  ( 71.00148000485552302, 59.33579794997937995, 3.971832046809253391 ) ) ;
#22447 = CARTESIAN_POINT ( 'NONE',  ( 23.19876663987166054, 3.510391698098890956, -3.664004875277358408 ) ) ;
#22448 = ORIENTED_EDGE ( 'NONE', *, *, #17927, .F. ) ;
#22449 = ORIENTED_EDGE ( 'NONE', *, *, #18065, .F. ) ;
#22450 = CARTESIAN_POINT ( 'NONE',  ( 21.85643539959779602, 4.838159542671753854, -10.55000746994157979 ) ) ;
#22451 = CARTESIAN_POINT ( 'NONE',  ( 21.85643539961850479, 4.025506921146978279, 3.384544483176039620 ) ) ;
#22452 = ORIENTED_EDGE ( 'NONE', *, *, #19028, .F. ) ;
#22453 = CARTESIAN_POINT ( 'NONE',  ( 66.27376694608931018, 57.73522568913554665, 4.000000000000000000 ) ) ;
#22454 = CARTESIAN_POINT ( 'NONE',  ( 81.29034902430632314, 64.00233822785270377, 3.292658836682930357 ) ) ;
#22455 = CARTESIAN_POINT ( 'NONE',  ( 87.65094362820954643, -0.09597545124639318692, -4.742286025697146634 ) ) ;
#22456 = ORIENTED_EDGE ( 'NONE', *, *, #31430, .T. ) ;
#22457 = AXIS2_PLACEMENT_3D ( 'NONE', #1648, #1053, #14184 ) ;
#22458 = CARTESIAN_POINT ( 'NONE',  ( 0.4257515640715447969, -32.72196143500892163, 7.757178535559534183 ) ) ;
#22459 = ORIENTED_EDGE ( 'NONE', *, *, #19715, .T. ) ;
#22460 = CARTESIAN_POINT ( 'NONE',  ( 17.10475337451625322, -3.043619170508630400, 2.876008462753611994 ) ) ;
#22461 = CARTESIAN_POINT ( 'NONE',  ( 31.71966209317523422, -0.5565497988919112515, -5.157018431203386655 ) ) ;
#22462 = CARTESIAN_POINT ( 'NONE',  ( 5.162032219521623944, -29.07102167996093911, 7.766640943994643997 ) ) ;
#22463 = DIRECTION ( 'NONE',  ( -0.9848077530122142376, 0.1736481776668952204, 0.000000000000000000 ) ) ;
#22464 = PRODUCT ( 'Ruler Clamping Screw', 'Ruler Clamping Screw', '', ( #4641 ) ) ;
#22465 = VERTEX_POINT ( 'NONE', #30057 ) ;
#22466 = CARTESIAN_POINT ( 'NONE',  ( -32.34874870218063592, -26.64985754041175525, 6.700000000000000178 ) ) ;
#22467 = FACE_OUTER_BOUND ( 'NONE', #13989, .T. ) ;
#22468 = AXIS2_PLACEMENT_3D ( 'NONE', #4577, #28878, #36072 ) ;
#22469 = CARTESIAN_POINT ( 'NONE',  ( 28.74930798315838132, -3.747080672683058555, 4.540790173945463692 ) ) ;
#22470 = ORIENTED_EDGE ( 'NONE', *, *, #26829, .F. ) ;
#22471 = ORIENTED_EDGE ( 'NONE', *, *, #34855, .T. ) ;
#22472 = CARTESIAN_POINT ( 'NONE',  ( 37.10898288256137079, -2.404723019174210830, 5.951907613904549699 ) ) ;
#22473 = CARTESIAN_POINT ( 'NONE',  ( 1.625050579259687433, -33.05680123510155255, 7.782861076432730840 ) ) ;
#22474 = EDGE_CURVE ( 'NONE', #23718, #16154, #7415, .T. ) ;
#22475 = CARTESIAN_POINT ( 'NONE',  ( 66.41604928081308401, 57.80773248233377615, -4.000000000000022204 ) ) ;
#22476 = DIRECTION ( 'NONE',  ( -0.000000000000000000, -0.000000000000000000, -1.000000000000000000 ) ) ;
#22477 = EDGE_CURVE ( 'NONE', #393, #22149, #3000, .T. ) ;
#22478 = VERTEX_POINT ( 'NONE', #1868 ) ;
#22479 = LINE ( 'NONE', #28644, #17334 ) ;
#22480 = CARTESIAN_POINT ( 'NONE',  ( 3.015109609237833332, -26.32624206733842698, 7.750000000000000888 ) ) ;
#22481 = CARTESIAN_POINT ( 'NONE',  ( -0.07645708395594488782, -32.58535952412007930, 6.894806418505347700 ) ) ;
#22482 = DIRECTION ( 'NONE',  ( 0.4582725098355734938, -0.8888117386314180468, 0.000000000000000000 ) ) ;
#22483 = EDGE_LOOP ( 'NONE', ( #16125, #5664, #22972, #37143, #23735 ) ) ;
#22484 = FACE_BOUND ( 'NONE', #17456, .T. ) ;
#22485 = EDGE_CURVE ( 'NONE', #24953, #530, #31248, .T. ) ;
#22486 = EDGE_CURVE ( 'NONE', #16194, #20410, #23666, .T. ) ;
#22487 = FILL_AREA_STYLE_COLOUR ( '', #37660 ) ;
#22488 = EDGE_LOOP ( 'NONE', ( #29171, #405, #24713, #14404 ) ) ;
#22489 = CARTESIAN_POINT ( 'NONE',  ( 23.42158288118685050, 3.688889536555259419, 3.302951128627464872 ) ) ;
#22490 = CARTESIAN_POINT ( 'NONE',  ( 81.56437483599468408, 65.67932636690369463, -1.586031901070164674 ) ) ;
#22491 = CARTESIAN_POINT ( 'NONE',  ( 78.61080321328475407, 66.00207709680661594, 1.298998371267750640 ) ) ;
#22492 = CARTESIAN_POINT ( 'NONE',  ( -70.05509079466530409, -21.28757458321500451, 3.936323582624761119 ) ) ;
#22493 = ORIENTED_EDGE ( 'NONE', *, *, #33249, .T. ) ;
#22494 = VERTEX_POINT ( 'NONE', #39507 ) ;
#22495 = CARTESIAN_POINT ( 'NONE',  ( 74.78802096516436393, 63.01683072882820369, -3.322260703561485062 ) ) ;
#22497 = CARTESIAN_POINT ( 'NONE',  ( -0.9606818258635283492, -27.29645349747919170, 6.894806418505347700 ) ) ;
#22496 = DIRECTION ( 'NONE',  ( -0.000000000000000000, -0.000000000000000000, -1.000000000000000000 ) ) ;
#22498 = CARTESIAN_POINT ( 'NONE',  ( 19.86836432286185783, 6.624182616967236648, -3.307336789426305934 ) ) ;
#22499 = CARTESIAN_POINT ( 'NONE',  ( 81.25681022244550888, 61.36874951788873034, -1.439474762807439134 ) ) ;
#22500 = CARTESIAN_POINT ( 'NONE',  ( 76.91271350297705567, 62.89131350122330133, 3.776276000685970136 ) ) ;
#22501 = ORIENTED_EDGE ( 'NONE', *, *, #1551, .T. ) ;
#22502 = ORIENTED_EDGE ( 'NONE', *, *, #19307, .F. ) ;
#22503 = FACE_OUTER_BOUND ( 'NONE', #4773, .T. ) ;
#22504 = VECTOR ( 'NONE', #36798, 1000.000000000000000 ) ;
#22505 = CARTESIAN_POINT ( 'NONE',  ( 0.5371711504799139281, -32.87097875789517332, 7.695279973900954751 ) ) ;
#22506 = CARTESIAN_POINT ( 'NONE',  ( 79.23414132050105252, 66.25012704882071546, 1.421876342974069507 ) ) ;
#22508 = CARTESIAN_POINT ( 'NONE',  ( 18.26922817967627921, 11.64739335993193947, 2.499999999999998668 ) ) ;
#22507 = CARTESIAN_POINT ( 'NONE',  ( -0.1988289257493946471, -32.50982254841889585, 7.006908160621415860 ) ) ;
#22509 = CARTESIAN_POINT ( 'NONE',  ( 31.64923038865762805, -3.528005414130610529, -5.019302312848182623 ) ) ;
#22510 = CARTESIAN_POINT ( 'NONE',  ( -1.699415837186460942, -29.60626003165447173, 7.701140543647732706 ) ) ;
#22511 = CARTESIAN_POINT ( 'NONE',  ( 3.565483696522954826, -26.72714530743686012, 6.903372536218455480 ) ) ;
#22512 = FACE_OUTER_BOUND ( 'NONE', #25091, .T. ) ;
#22513 = PLANE ( 'NONE',  #38835 ) ;
#22514 = CARTESIAN_POINT ( 'NONE',  ( -0.4487487021806388365, -26.64985754041175525, 6.800000000000000711 ) ) ;
#22515 = CARTESIAN_POINT ( 'NONE',  ( 36.78040056622536014, -2.229284608445112781, -5.922136277988401254 ) ) ;
#22516 = LINE ( 'NONE', #31774, #32532 ) ;
#22517 = CARTESIAN_POINT ( 'NONE',  ( 1.716602532315689267, -33.06989263416611635, 7.638991368224661294 ) ) ;
#22518 = CARTESIAN_POINT ( 'NONE',  ( 1.736346942945643512, -32.96974004645320377, 7.693875151218753317 ) ) ;
#22519 = CARTESIAN_POINT ( 'NONE',  ( 2.089729628487263735, -32.94756467017376167, 6.988553391373224066 ) ) ;
#22520 = EDGE_CURVE ( 'NONE', #26610, #9487, #18045, .T. ) ;
#22521 = CARTESIAN_POINT ( 'NONE',  ( 22.23218040091930092, -10.39938183745549694, -2.500000000000000000 ) ) ;
#22522 = CARTESIAN_POINT ( 'NONE',  ( 21.87789367320688072, -13.40669691499416061, 2.499999999999999556 ) ) ;
#22523 = EDGE_CURVE ( 'NONE', #37904, #21904, #39185, .T. ) ;
#22524 = B_SPLINE_SURFACE_WITH_KNOTS ( 'NONE', 5, 3, ( 
 ( #36759, #1581, #14112, #17805, #30390, #33692, #36965, #11015, #8744, #21328, #39226, #36160, #33073, #4857, #39426, #29971, #1786, #11216, #9573, #18219, #2616, #31211, #9781, #40441, #28311, #25031, #12250, #15340, #24822, #15550, #6505, #37166, #21944, #3240 ),
 ( #34517, #22154, #37566, #27895, #5887, #3032, #8951, #37976, #28104, #33903, #5677, #9361, #129, #34726, #37367, #9163, #19054, #328, #40659, #12461, #21737, #30811, #37767, #31617, #34318, #6294, #12033, #15757, #15956, #15135, #18842, #27691, #6088, #12660 ),
 ( #18622, #31412, #25236, #3440, #21537, #28518, #12868, #25433, #40247, #24611, #34115, #18423, #31011, #2816, #22560, #13074, #1150, #35125, #38578, #16958, #13472, #38786, #26252, #13684, #6903, #32636, #22764, #32428, #31823, #19459, #10581, #32033, #4036, #4225 ),
 ( #16749, #4431, #29331, #34928, #13269, #23153, #25636, #3840, #9981, #35720, #936, #13881, #7496, #16357, #29534, #28726, #28931, #19254, #20059, #16162, #1347, #732, #35526, #26448, #38178, #38975, #22363, #6706, #3637, #538, #25839, #22960, #16553, #29131 ),
 ( #38373, #10174, #35330, #7099, #10384, #19662, #32236, #26047, #7296, #19857, #8289, #10976, #14069, #2153, #36517, #4818, #5021, #36121, #5225, #20450, #27451, #27242, #11378, #23557, #24154, #26843, #39383, #1955, #33651, #11175, #17760, #10774, #23353, #23746 ),
 ( #23943, #36714, #20864, #14881, #33456, #32834, #7701, #20250, #39593, #8497, #7901, #30347, #17553, #33028, #5427, #14473, #14673, #11578, #1743, #14274, #21080, #17966, #33236, #30139, #36317, #35924, #39809, #30552, #8087, #27047, #29725, #2363, #4626, #17153 ),
 ( #20654, #1536, #26648, #39182, #17347, #29925, #37521, #40402, #27850, #8907, #21696, #19009, #15502, #18794, #31166, #5635, #18174, #27649, #30766, #21491, #12206, #22105, #34682, #12616, #12415, #24568, #24778, #8701, #25183, #30966, #9316, #6246, #37714, #31570 ),
 ( #2568, #2772, #40610, #9521, #40205, #15911, #34275, #24360, #37323, #34471, #6457, #3395, #33854, #24986, #11988, #37119, #40007, #36923, #6044, #15090, #15708, #11779, #21281, #34067, #2984, #21893, #31368, #18380, #18578, #5842, #15298, #3192, #9120, #28262 ),
 ( #86, #28060, #35281, #22314, #9934, #29283, #25389, #19615, #4181, #12815, #37928, #25793, #4383, #35082, #22908, #32189, #6857, #22515, #19411, #10126, #1097, #31773, #16508, #38530, #26204, #32387, #16312, #7449, #22714, #20005, #3987, #28680, #19208, #7248 ),
 ( #3788, #28880, #29084, #10529, #689, #35476, #28470, #277, #13227, #7048, #31984, #13632, #34883, #38326, #887, #13420, #25996, #10336, #6657, #19811, #38733, #9735, #16697, #23109, #3589, #16114, #35676, #490, #32586, #13024, #25589, #38133, #39134, #36074 ),
 ( #27193, #4767, #30286, #11128, #26596, #17498, #33403, #8042, #10931, #29678, #14227, #32788, #21028, #23698, #33601, #29487, #20600, #11325, #17707, #7851, #20403, #2102, #24095, #39338, #36266, #32983, #16908, #20806, #14617, #17302, #33184, #35874, #26993, #39751 ),
 ( #29880, #36461, #20204, #23510, #4579, #39540, #4971, #8444, #11528, #1489, #36663, #23307, #1693, #13834, #23890, #10725, #8236, #26800, #30095, #1297, #17106, #26403, #38932, #5176, #7653, #14023, #1904, #14424, #27799, #40350, #5991, #28006, #24935, #12361 ),
 ( #21641, #8651, #24513, #37468, #5376, #40155, #2928, #5578, #21228, #9264, #31113, #11939, #12147, #30711, #40549, #15040, #22051, #21844, #18529, #18118, #18741, #34422, #15447, #2516, #31318, #21436, #34012, #37269, #28203, #5786, #6196, #17915, #30497, #18324 ),
 ( #3140, #15657, #35, #9465, #12562, #27393, #2305, #14828, #34221, #25132, #27601, #37664, #24720, #37064, #39957, #11730, #9065, #24305, #15243, #36870, #8853, #33799, #30914, #2722, #433, #4134, #22461, #7201, #28833, #3535, #35232, #10284, #25742, #28630 ),
 ( #34831, #25340, #13371, #6607, #10080, #29237, #38283, #22859, #38480, #25946, #19154, #16649, #35028, #3942, #3340, #31721, #35431, #16061, #16261, #16463, #7002, #31931, #13179, #12973, #25542, #643, #3738, #19760, #32341, #34629, #19361, #15860, #32145, #6806 ),
 ( #1045, #223, #38083, #31517, #29035, #28417, #13579, #9885, #19568, #38685, #37874, #26153, #10482, #6402, #18953, #12763, #22666, #839, #9681, #22264, #23645, #4914, #1850, #30035, #29437, #23260, #26354, #26545, #36212, #36412, #35827, #39692, #17253, #7401 ),
 ( #20756, #30238, #16855, #7992, #7602, #20154, #23062, #14372, #1250, #32736, #38886, #39083, #20548, #8184, #4531, #35627, #29826, #19954, #7799, #17445, #33347, #2053, #13787, #33132, #17054, #29630, #32536, #4335, #4719, #10679, #39484, #5123, #17656, #1444 ),
 ( #26942, #13976, #10880, #36022, #1639, #23454, #14566, #20352, #32931, #14178, #11273, #26748, #39287, #11075, #23837, #27140, #8397, #2674, #27955, #36613, #20971, #8801, #28160, #18070, #5941, #15193, #30660, #33747, #2469, #33961, #24884, #14776, #40304, #21593 ) ),
 .UNSPECIFIED., .F., .F., .F.,
 ( 6, 5, 2, 5, 6 ),
 ( 4, 1, 1, 1, 1, 1, 1, 1, 1, 1, 1, 1, 1, 1, 1, 1, 1, 1, 1, 1, 1, 1, 1, 1, 1, 1, 1, 1, 1, 1, 1, 4 ),
 ( -0.01000000000000000021, 0.000000000000000000, 0.5000000000000000000, 1.000000000000000000, 1.010000000000000009 ),
 ( 0.000000000000000000, 0.0006830978666945804927, 0.001366195733389160985, 0.001935443955634644784, 0.002390842533431031345, 0.002732391466778321971, 0.003017015577901063870, 0.003244714866799257909, 0.003387026922360628425, 0.003500876566809725445, 0.003586263800146547668, 0.003671651033483370324, 0.003757038266820192981, 0.003842425500157015204, 0.003956275144606112223, 0.004098587200167483173, 0.004269361666841127619, 0.004497060955739321658, 0.004781685066862063557, 0.005123234000209354183, 0.005578632578005740528, 0.006147880800251224326, 0.006830978666945805577, 0.007514076533640385962, 0.008424873689233159518, 0.009563370133724125380, 0.01092956586711328788, 0.01229576160050244865, 0.01411735591168799576, 0.01639434880066993269, 0.01912674026744825076, 0.02185913173422657577 ),
 .UNSPECIFIED. ) ;
#22525 = ORIENTED_EDGE ( 'NONE', *, *, #33683, .F. ) ;
#22526 = CARTESIAN_POINT ( 'NONE',  ( -12.87867591359218977, -26.64985754041175525, 6.700000000000000178 ) ) ;
#22527 = CARTESIAN_POINT ( 'NONE',  ( 67.94738262351316394, 58.59965392607728063, -3.985705108533788898 ) ) ;
#22528 = EDGE_CURVE ( 'NONE', #14780, #18906, #29848, .T. ) ;
#22529 = ORIENTED_EDGE ( 'NONE', *, *, #35482, .T. ) ;
#22530 = DIRECTION ( 'NONE',  ( -1.000000000000000000, 0.000000000000000000, 0.000000000000000000 ) ) ;
#22531 = EDGE_CURVE ( 'NONE', #3507, #12043, #8705, .T. ) ;
#22532 = CARTESIAN_POINT ( 'NONE',  ( 30.73821809742792510, -3.303287531218632278, 4.965085915138678807 ) ) ;
#22533 = CARTESIAN_POINT ( 'NONE',  ( 23.77293744817952970, 2.857359405969741584, 3.961609048350384743 ) ) ;
#22534 = CARTESIAN_POINT ( 'NONE',  ( 1.078322358366002653, -26.22732166111063989, 7.721096864323905962 ) ) ;
#22535 = AXIS2_PLACEMENT_3D ( 'NONE', #6868, #28690, #700 ) ;
#22536 = PLANE ( 'NONE',  #36329 ) ;
#22537 = EDGE_LOOP ( 'NONE', ( #4138, #17126 ) ) ;
#22538 = CARTESIAN_POINT ( 'NONE',  ( 23.75094394727146252, 3.570271603488096801, 3.156956672783068019 ) ) ;
#22539 = DIRECTION ( 'NONE',  ( 0.000000000000000000, 0.000000000000000000, 1.000000000000000000 ) ) ;
#22540 = CARTESIAN_POINT ( 'NONE',  ( 78.85897125043999267, 66.02047811250265852, 1.830101370957687879 ) ) ;
#22541 = ADVANCED_BREP_SHAPE_REPRESENTATION ( '', ( #39670, #30744 ), #18224 ) ;
#22542 = CARTESIAN_POINT ( 'NONE',  ( -59.93345510331042902, 24.73247967741478703, 12.49999999999999645 ) ) ;
#22543 = EDGE_LOOP ( 'NONE', ( #27434, #3467, #13552, #33308, #30043 ) ) ;
#22544 = CARTESIAN_POINT ( 'NONE',  ( 78.53692321045886615, 63.86140601108343873, -3.670385203786640904 ) ) ;
#22546 = CARTESIAN_POINT ( 'NONE',  ( -1.664445652997000646, -30.05777379808717242, 6.864651958020303368 ) ) ;
#22545 = CARTESIAN_POINT ( 'NONE',  ( 23.07526676296097179, 0.3585942713019621975, 5.936990365695360872 ) ) ;
#22547 = CARTESIAN_POINT ( 'NONE',  ( 81.57279438772125957, 63.75980975930797712, -3.125232205748940117 ) ) ;
#22548 = CARTESIAN_POINT ( 'NONE',  ( 80.21769632236900804, 61.97993766192919907, 3.195657361810719799 ) ) ;
#22549 = DIRECTION ( 'NONE',  ( 1.000000000000000000, 0.000000000000000000, 0.000000000000000000 ) ) ;
#22550 = CARTESIAN_POINT ( 'NONE',  ( 80.71704827558885142, 66.21292280724348700, 1.000000000000000000 ) ) ;
#22551 = CARTESIAN_POINT ( 'NONE',  ( 1.551251297819356001, -26.64985754041175525, 6.700000000000000178 ) ) ;
#22552 = CARTESIAN_POINT ( 'NONE',  ( 25.11613067079463590, -2.903500246237137983, -5.705645831387469613 ) ) ;
#22553 = CARTESIAN_POINT ( 'NONE',  ( -42.83131703149249603, -29.56993018339339940, 6.800000000000000711 ) ) ;
#22554 = ORIENTED_EDGE ( 'NONE', *, *, #16875, .T. ) ;
#22555 = CARTESIAN_POINT ( 'NONE',  ( -73.74378307871597826, -3.485633296868869468, 9.598859659615810003 ) ) ;
#22556 = CARTESIAN_POINT ( 'NONE',  ( 27.44318568885298504, 0.9300194081793810019, -4.489570861336245500 ) ) ;
#22557 = CARTESIAN_POINT ( 'NONE',  ( 0.6225211420409756391, -26.24003551177748861, 7.750000000000000888 ) ) ;
#22558 = DIRECTION ( 'NONE',  ( -0.000000000000000000, 1.000000000000000000, 0.000000000000000000 ) ) ;
#22559 = CARTESIAN_POINT ( 'NONE',  ( 30.76389835349712243, -3.760085712427588600, -4.556058237597376603 ) ) ;
#22560 = CARTESIAN_POINT ( 'NONE',  ( 37.17658989031565397, -2.564865607421146887, -5.981013799454680147 ) ) ;
#22561 = CARTESIAN_POINT ( 'NONE',  ( 3.744196778873498666, -32.28708296902909325, 6.887945620086123100 ) ) ;
#22562 = CARTESIAN_POINT ( 'NONE',  ( 17.10386648299642687, 9.264936115020711682, 2.854956177116559690 ) ) ;
#22563 = FACE_OUTER_BOUND ( 'NONE', #21453, .T. ) ;
#22564 = CARTESIAN_POINT ( 'NONE',  ( -0.9128197825508301833, -27.39481314169073300, 7.635761828346577573 ) ) ;
#22565 = DIRECTION ( 'NONE',  ( -0.3420201433256601087, -0.9396926207859114255, -0.000000000000000000 ) ) ;
#22566 = AXIS2_PLACEMENT_3D ( 'NONE', #28901, #38350, #3608 ) ;
#22567 = CYLINDRICAL_SURFACE ( 'NONE', #11161, 0.09010775117052825800 ) ;
#22568 = CARTESIAN_POINT ( 'NONE',  ( 23.56275793004198249, 1.092801103661935391, -5.226603514420215646 ) ) ;
#22569 = CARTESIAN_POINT ( 'NONE',  ( 29.64729738269542381, 1.157578426279490147, -4.258750744271380562 ) ) ;
#22570 = CARTESIAN_POINT ( 'NONE',  ( -41.07867591359219972, -24.55319635012989110, 6.700000000000000178 ) ) ;
#22571 = VERTEX_POINT ( 'NONE', #11095 ) ;
#22572 = CARTESIAN_POINT ( 'NONE',  ( 66.84954949145740954, 57.97782447864501165, 3.999382933223862846 ) ) ;
#22573 = EDGE_CURVE ( 'NONE', #5350, #15998, #10816, .T. ) ;
#22574 = EDGE_CURVE ( 'NONE', #7218, #34783, #32755, .T. ) ;
#22575 = CARTESIAN_POINT ( 'NONE',  ( 21.76158391687864579, 5.855790371669074901, -3.369038255546072946 ) ) ;
#22576 = CARTESIAN_POINT ( 'NONE',  ( 84.31734228151684363, 3.084090681639994003, 0.3216814846013044127 ) ) ;
#22577 = EDGE_CURVE ( 'NONE', #5492, #11497, #6261, .T. ) ;
#22578 = EDGE_LOOP ( 'NONE', ( #7829, #40031, #29484, #19699 ) ) ;
#22579 = CARTESIAN_POINT ( 'NONE',  ( 27.41857586891900667, 1.095318458406062456, 4.485729903744793745 ) ) ;
#22580 = AXIS2_PLACEMENT_3D ( 'NONE', #13509, #23185, #22593 ) ;
#22581 = CARTESIAN_POINT ( 'NONE',  ( 2.319617088658799453, -32.91306737433055929, 7.730758795053806587 ) ) ;
#22582 = CARTESIAN_POINT ( 'NONE',  ( 1.207584434645498028, -26.10564138716367211, 7.761113333116787416 ) ) ;
#22583 = ORIENTED_EDGE ( 'NONE', *, *, #12068, .F. ) ;
#22584 = CARTESIAN_POINT ( 'NONE',  ( 3.973940671657854029, -26.92785926235529104, 7.785096263473212375 ) ) ;
#22585 = ORIENTED_EDGE ( 'NONE', *, *, #17741, .T. ) ;
#22586 = ORIENTED_EDGE ( 'NONE', *, *, #34112, .T. ) ;
#22587 = CARTESIAN_POINT ( 'NONE',  ( 80.41811942164733296, 62.87504864752338563, -3.537885823842629396 ) ) ;
#22588 = CARTESIAN_POINT ( 'NONE',  ( -1.720325740817129301, -28.89808781674439686, 7.784725160561909441 ) ) ;
#22589 = CARTESIAN_POINT ( 'NONE',  ( 80.11945187304060312, 63.42025125984827838, 3.710743084827279326 ) ) ;
#22592 = VERTEX_POINT ( 'NONE', #2076 ) ;
#22591 = ORIENTED_EDGE ( 'NONE', *, *, #4776, .T. ) ;
#22590 = DIRECTION ( 'NONE',  ( 0.000000000000000000, 0.000000000000000000, 1.000000000000000000 ) ) ;
#22593 = DIRECTION ( 'NONE',  ( 1.000000000000000000, 0.000000000000000000, -0.000000000000000000 ) ) ;
#22594 = DIRECTION ( 'NONE',  ( 0.000000000000000000, 0.000000000000000000, 1.000000000000000000 ) ) ;
#22595 = CARTESIAN_POINT ( 'NONE',  ( 33.78796187971178000, -4.855747518448159994, -3.446936011855299853 ) ) ;
#22596 = CARTESIAN_POINT ( 'NONE',  ( 22.62429625317078674, 4.579493676427568438, -3.091892255925898336 ) ) ;
#22597 = VERTEX_POINT ( 'NONE', #31438 ) ;
#22598 = LINE ( 'NONE', #25073, #30106 ) ;
#22599 = ORIENTED_EDGE ( 'NONE', *, *, #27281, .T. ) ;
#22600 = CARTESIAN_POINT ( 'NONE',  ( -1.034105916944730863, -31.59045773092190856, 6.959317978105167946 ) ) ;
#22601 = CARTESIAN_POINT ( 'NONE',  ( -13.07867591359219617, -24.55319635012989110, 6.700000000000000178 ) ) ;
#22602 = CIRCLE ( 'NONE', #34455, 0.1000000000000028644 ) ;
#22603 = CARTESIAN_POINT ( 'NONE',  ( -72.89750464017865283, 3.404720670759703527, -9.864174393176885047 ) ) ;
#22604 = CARTESIAN_POINT ( 'NONE',  ( -73.45070404594234503, 38.65432087843067421, -8.800414904976364028 ) ) ;
#22605 = CARTESIAN_POINT ( 'NONE',  ( -1.799609906766908685, -29.56993018339339940, 7.620413589471895399 ) ) ;
#22606 = CARTESIAN_POINT ( 'NONE',  ( 80.49267809498162762, 64.35807816991642483, 3.549391953833850977 ) ) ;
#22607 = CARTESIAN_POINT ( 'NONE',  ( 85.86655237490620607, 0.5075193453549979861, -5.999391133436077439 ) ) ;
#22608 = DIRECTION ( 'NONE',  ( 0.000000000000000000, 0.000000000000000000, 1.000000000000000000 ) ) ;
#22609 = CARTESIAN_POINT ( 'NONE',  ( -1.306989867689303697, -27.80139717009528511, 7.781480525794717273 ) ) ;
#22610 = CARTESIAN_POINT ( 'NONE',  ( 22.06611006309120171, 4.208718600211970973, -2.305420481420197731 ) ) ;
#22611 = CARTESIAN_POINT ( 'NONE',  ( 33.61618589921860689, -1.223535437620471011, 5.453016838738055760 ) ) ;
#22612 = DIRECTION ( 'NONE',  ( -0.000000000000000000, -0.000000000000000000, 1.000000000000000000 ) ) ;
#22613 = CARTESIAN_POINT ( 'NONE',  ( -0.3206046116097268639, -26.83577804592309590, 6.939395833800441338 ) ) ;
#22614 = CARTESIAN_POINT ( 'NONE',  ( 4.701862308883337782, -27.97269194523573432, 7.759451378593094972 ) ) ;
#22615 = CARTESIAN_POINT ( 'NONE',  ( -0.9931795851432037026, -27.33505157645927142, 7.643192810543826710 ) ) ;
#22616 =( BOUNDED_CURVE ( )  B_SPLINE_CURVE ( 3, ( #4894, #14353, #33532, #27323 ),
 .UNSPECIFIED., .F., .T. ) 
 B_SPLINE_CURVE_WITH_KNOTS ( ( 4, 4 ),
 ( 4.708531083176465515, 4.895802057644186966 ),
 .UNSPECIFIED. ) 
 CURVE ( )  GEOMETRIC_REPRESENTATION_ITEM ( )  RATIONAL_B_SPLINE_CURVE ( ( 1.000000000000000000, 0.9970795998553221295, 0.9970795998553221295, 1.000000000000000000 ) ) 
 REPRESENTATION_ITEM ( '' )  );
#22617 = ORIENTED_EDGE ( 'NONE', *, *, #5120, .T. ) ;
#22618 = CARTESIAN_POINT ( 'NONE',  ( 68.71160781503239434, 58.33825098880495119, 3.980709302925375503 ) ) ;
#22619 = CARTESIAN_POINT ( 'NONE',  ( 34.13625311161768394, -3.134515127487323749, 5.534185905105376335 ) ) ;
#22620 = CARTESIAN_POINT ( 'NONE',  ( 73.64144479846403613, 59.51803038729781292, -3.736020861036525531 ) ) ;
#22621 = CARTESIAN_POINT ( 'NONE',  ( -64.08758708074093136, 42.07456177364299066, -2.837280265527672540 ) ) ;
#22622 = CARTESIAN_POINT ( 'NONE',  ( 88.25065740119208613, -0.7696024251930051463, 2.713887439742028285 ) ) ;
#22623 = EDGE_CURVE ( 'NONE', #16334, #13771, #12684, .T. ) ;
#22624 = VERTEX_POINT ( 'NONE', #33371 ) ;
#22626 = CARTESIAN_POINT ( 'NONE',  ( -0.4171441595639596156, -26.78316706317107787, 7.013842709614101167 ) ) ;
#22625 = CARTESIAN_POINT ( 'NONE',  ( 80.95462345035979013, 63.09697225074528859, -3.406228740995798532 ) ) ;
#22627 = CARTESIAN_POINT ( 'NONE',  ( -69.47662317642280527, -46.72710078822078827, 9.894078484842815158 ) ) ;
#22628 = EDGE_CURVE ( 'NONE', #16824, #18814, #34279, .T. ) ;
#22629 = ORIENTED_EDGE ( 'NONE', *, *, #8162, .F. ) ;
#22630 = CARTESIAN_POINT ( 'NONE',  ( 10.50357756723356140, 59.39757829809867928, 1.000000000000000000 ) ) ;
#22631 = ORIENTED_EDGE ( 'NONE', *, *, #38344, .F. ) ;
#22632 = LINE ( 'NONE', #22232, #10358 ) ;
#22633 = VECTOR ( 'NONE', #10943, 1000.000000000000000 ) ;
#22634 = CIRCLE ( 'NONE', #29203, 2.500000000000002220 ) ;
#22635 = ORIENTED_EDGE ( 'NONE', *, *, #34210, .F. ) ;
#22636 = CARTESIAN_POINT ( 'NONE',  ( 79.46693819636867318, 65.20858797830474884, -3.188730975143405200 ) ) ;
#22637 = CARTESIAN_POINT ( 'NONE',  ( 5.150522559231670350, -30.15864875804516032, 7.747520101777648271 ) ) ;
#22638 = CARTESIAN_POINT ( 'NONE',  ( 21.81293742820567871, 1.745484945909191676, 6.400703180478840792 ) ) ;
#22640 = ORIENTED_EDGE ( 'NONE', *, *, #11139, .F. ) ;
#22639 = ORIENTED_EDGE ( 'NONE', *, *, #31118, .F. ) ;
#22641 = AXIS2_PLACEMENT_3D ( 'NONE', #5653, #25001, #18191 ) ;
#22642 = CARTESIAN_POINT ( 'NONE',  ( 4.741504651846523366, -28.04952573427642193, 6.920489980334477487 ) ) ;
#22643 = AXIS2_PLACEMENT_3D ( 'NONE', #31141, #2959, #15475 ) ;
#22645 = CARTESIAN_POINT ( 'NONE',  ( 3.977572546501451978, -32.22783162523180778, 7.686927408461907696 ) ) ;
#22644 = CARTESIAN_POINT ( 'NONE',  ( 4.569457157119717117, -31.39433534204675524, 6.868387053540519815 ) ) ;
#22646 = DIRECTION ( 'NONE',  ( 0.000000000000000000, 1.000000000000000000, 0.000000000000000000 ) ) ;
#22647 = CARTESIAN_POINT ( 'NONE',  ( -63.66761068000498369, 44.17545465894031764, -2.094006737888894687 ) ) ;
#22648 = CARTESIAN_POINT ( 'NONE',  ( 72.54144496250529528, 58.88102433069186503, 3.699617110138615939 ) ) ;
#22649 = EDGE_CURVE ( 'NONE', #36238, #19982, #17883, .T. ) ;
#22650 = CARTESIAN_POINT ( 'NONE',  ( 23.90047232000282662, 3.021372428902185714, -3.777954186841565587 ) ) ;
#22651 = ORIENTED_EDGE ( 'NONE', *, *, #27748, .T. ) ;
#22652 = ORIENTED_EDGE ( 'NONE', *, *, #26785, .T. ) ;
#22653 = CARTESIAN_POINT ( 'NONE',  ( 21.85643539959774273, -7.955861821551272861, 12.12136874776577322 ) ) ;
#22654 = CARTESIAN_POINT ( 'NONE',  ( 21.86870537174298335, 3.698784010477664808, -3.388912068454548621 ) ) ;
#22655 = CARTESIAN_POINT ( 'NONE',  ( 1.120206005321838783, -33.02151157302147055, 7.733670252284491120 ) ) ;
#22656 = CARTESIAN_POINT ( 'NONE',  ( 80.85068185324867329, 64.93836743322185612, 3.187395722566882750 ) ) ;
#22657 = CARTESIAN_POINT ( 'NONE',  ( 88.87549651282381546, -1.666836616135117799, 1.222388837546040330 ) ) ;
#22658 = ORIENTED_EDGE ( 'NONE', *, *, #24979, .T. ) ;
#22659 = CARTESIAN_POINT ( 'NONE',  ( 0.4809726510178614634, -32.74373249318228574, 7.785172627573962778 ) ) ;
#22660 = ORIENTED_EDGE ( 'NONE', *, *, #125, .T. ) ;
#22661 = CARTESIAN_POINT ( 'NONE',  ( 15.05324942562365464, -4.021369621152198981, 2.555821655718428342 ) ) ;
#22662 = EDGE_CURVE ( 'NONE', #28211, #4500, #5141, .T. ) ;
#22663 = VECTOR ( 'NONE', #10140, 1000.000000000000000 ) ;
#22664 = CARTESIAN_POINT ( 'NONE',  ( 36.94849503072852315, -2.665731531992193926, 5.973104270911074209 ) ) ;
#22665 = CARTESIAN_POINT ( 'NONE',  ( 5.078470208622237969, -29.18445660682317211, 6.979335674598004857 ) ) ;
#22666 = CARTESIAN_POINT ( 'NONE',  ( 36.79757171488110146, -2.556340929038857901, -5.949549037378906391 ) ) ;
#22667 = CARTESIAN_POINT ( 'NONE',  ( 0.5708372184697405594, -32.77681504654623268, 7.680992449362118890 ) ) ;
#22668 = CARTESIAN_POINT ( 'NONE',  ( 84.10560360838722715, 3.011181495113149698, -0.2494236887672163505 ) ) ;
#22669 = DIRECTION ( 'NONE',  ( -0.000000000000000000, -1.000000000000000000, -0.000000000000000000 ) ) ;
#22670 = ORIENTED_EDGE ( 'NONE', *, *, #22180, .F. ) ;
#22671 = CARTESIAN_POINT ( 'NONE',  ( -1.267760583032661037, -27.71561997405539302, 7.754798119455333705 ) ) ;
#22672 = TOROIDAL_SURFACE ( 'NONE', #28567, 31.02204673211315011, 3.000000000000000000 ) ;
#22673 = DIRECTION ( 'NONE',  ( 1.000000000000000000, 0.000000000000000000, 0.000000000000000000 ) ) ;
#22674 = CARTESIAN_POINT ( 'NONE',  ( 31.98929602146294116, -3.342055116537107295, 5.177998144997084218 ) ) ;
#22675 = EDGE_CURVE ( 'NONE', #2698, #2900, #36635, .T. ) ;
#22676 = ORIENTED_EDGE ( 'NONE', *, *, #14160, .T. ) ;
#22677 = ORIENTED_EDGE ( 'NONE', *, *, #23300, .F. ) ;
#22678 = CARTESIAN_POINT ( 'NONE',  ( 23.38377539308148201, 3.557990533569439506, 3.100742785337903928 ) ) ;
#22679 = DIRECTION ( 'NONE',  ( -0.000000000000000000, -0.000000000000000000, 1.000000000000000000 ) ) ;
#22680 = CARTESIAN_POINT ( 'NONE',  ( 66.42891085676521357, 57.77139747978225870, -4.000000000000010658 ) ) ;
#22681 = CARTESIAN_POINT ( 'NONE',  ( 87.09538489576669917, -1.473322093048123005, -4.746830818090543858 ) ) ;
#22682 = ORIENTED_EDGE ( 'NONE', *, *, #31587, .T. ) ;
#22683 =( NAMED_UNIT ( * ) PLANE_ANGLE_UNIT ( ) SI_UNIT ( $, .RADIAN. ) );
#22684 = ORIENTED_EDGE ( 'NONE', *, *, #4058, .F. ) ;
#22685 = FACE_BOUND ( 'NONE', #15360, .T. ) ;
#22686 = DIRECTION ( 'NONE',  ( 1.000000000000000000, 0.000000000000000000, 0.000000000000000000 ) ) ;
#22687 = VERTEX_POINT ( 'NONE', #37035 ) ;
#22688 = CARTESIAN_POINT ( 'NONE',  ( 80.93658766080253031, 66.04709959793316898, -1.728104186158372579 ) ) ;
#22689 = ADVANCED_FACE ( 'NONE', ( #34752 ), #2488, .F. ) ;
#22690 = AXIS2_PLACEMENT_3D ( 'NONE', #36318, #11379, #14674 ) ;
#22691 = CARTESIAN_POINT ( 'NONE',  ( 2.972966256002666618, -26.41706555567719050, 7.759451378593095860 ) ) ;
#22692 = ORIENTED_EDGE ( 'NONE', *, *, #26045, .T. ) ;
#22693 = CARTESIAN_POINT ( 'NONE',  ( 76.15169681074901575, 61.58848496619829405, -3.887901781369006660 ) ) ;
#22694 = VECTOR ( 'NONE', #39815, 1000.000000000000000 ) ;
#22696 = FACE_OUTER_BOUND ( 'NONE', #27665, .T. ) ;
#22695 = CARTESIAN_POINT ( 'NONE',  ( 2.491849584607222834, -26.16059047924537140, 6.984548363133216142 ) ) ;
#22697 = CARTESIAN_POINT ( 'NONE',  ( 16.37661538275509443, 9.897519661642579791, -2.762364919055407597 ) ) ;
#22698 = CARTESIAN_POINT ( 'NONE',  ( 77.42503339237353543, 60.33561942134746658, 3.121245467013677111 ) ) ;
#22699 = CARTESIAN_POINT ( 'NONE',  ( 4.430837595856232269, -27.54393501177549908, 6.988553391373218737 ) ) ;
#22700 = VECTOR ( 'NONE', #8618, 1000.000000000000114 ) ;
#22701 = CARTESIAN_POINT ( 'NONE',  ( -12.99139449055068241, -10.90558813203967148, 6.000000000000000000 ) ) ;
#22702 = LINE ( 'NONE', #1683, #22993 ) ;
#22703 = CARTESIAN_POINT ( 'NONE',  ( 82.22574661183178080, 63.03983423078060611, 2.217414436011084788 ) ) ;
#22704 = CARTESIAN_POINT ( 'NONE',  ( 87.00441857019603731, 0.6302321798448609069, -4.918210918608230564 ) ) ;
#22705 = CARTESIAN_POINT ( 'NONE',  ( 28.10206848396558499, 1.736549293047330300, -3.980455106513370200 ) ) ;
#22706 = EDGE_CURVE ( 'NONE', #31748, #35240, #30257, .T. ) ;
#22707 = EDGE_CURVE ( 'NONE', #16761, #8120, #33980, .T. ) ;
#22708 = CARTESIAN_POINT ( 'NONE',  ( 2.340283621464598340, -26.23067316296506846, 7.785868773668302545 ) ) ;
#22709 = CARTESIAN_POINT ( 'NONE',  ( 3.578439373864104045, -26.73568756415219738, 6.969307238440505259 ) ) ;
#22710 = EDGE_CURVE ( 'NONE', #17652, #38094, #21405, .T. ) ;
#22711 = DIRECTION ( 'NONE',  ( -0.4690749385695654472, -0.8831583674551004570, 0.000000000000000000 ) ) ;
#22712 = CARTESIAN_POINT ( 'NONE',  ( 0.7341752703951600623, -26.31010747957196827, 6.979335674598004857 ) ) ;
#22713 = CARTESIAN_POINT ( 'NONE',  ( 0.000000000000000000, 10.37661300689600097, 2.500000000000000000 ) ) ;
#22714 = CARTESIAN_POINT ( 'NONE',  ( 29.34601568743050493, 0.9961685670913987822, -4.626954042955691015 ) ) ;
#22715 = LINE ( 'NONE', #31985, #23319 ) ;
#22716 = CARTESIAN_POINT ( 'NONE',  ( -0.9060015222600810159, -31.75321274565758856, 7.769368695748492648 ) ) ;
#22717 = DIRECTION ( 'NONE',  ( 0.8660254037844450359, -0.4999999999999888978, -0.000000000000000000 ) ) ;
#22718 = CARTESIAN_POINT ( 'NONE',  ( -81.20922607448022745, 10.50636700977107196, 3.841544977761441437 ) ) ;
#22719 = ADVANCED_FACE ( 'NONE', ( #8821 ), #14587, .F. ) ;
#22720 = CARTESIAN_POINT ( 'NONE',  ( 21.94901396481228417, -12.22285702164925958, -2.500000000000000000 ) ) ;
#22721 = DIRECTION ( 'NONE',  ( 1.000000000000000000, 0.000000000000000000, 0.000000000000000000 ) ) ;
#22722 = AXIS2_PLACEMENT_3D ( 'NONE', #24275, #21402, #23852 ) ;
#22723 = EDGE_LOOP ( 'NONE', ( #34707, #11135, #28347, #36235 ) ) ;
#22724 = ORIENTED_EDGE ( 'NONE', *, *, #33345, .T. ) ;
#22725 = DIRECTION ( 'NONE',  ( -0.000000000000000000, 1.000000000000000000, -0.000000000000000000 ) ) ;
#22726 = CARTESIAN_POINT ( 'NONE',  ( 68.50220056233268906, 58.89075781393282227, -3.976359261632471220 ) ) ;
#22727 = VECTOR ( 'NONE', #25901, 1000.000000000000000 ) ;
#22728 = CARTESIAN_POINT ( 'NONE',  ( 3.061823518957293100, -26.34556267481334757, 6.903112506833887885 ) ) ;
#22729 = ORIENTED_EDGE ( 'NONE', *, *, #24487, .F. ) ;
#22730 = DIRECTION ( 'NONE',  ( -0.3754033771448240797, -0.6502177225477954181, 0.6605219282605377940 ) ) ;
#22731 = LINE ( 'NONE', #35295, #37709 ) ;
#22732 = CARTESIAN_POINT ( 'NONE',  ( 23.45399895271802748, 3.179065097157539821, 3.819164652932915072 ) ) ;
#22733 = CARTESIAN_POINT ( 'NONE',  ( 5.043922214925016689, -28.53513699343982779, 7.011627023500182077 ) ) ;
#22734 =( BOUNDED_CURVE ( )  B_SPLINE_CURVE ( 3, ( #7550, #32885, #39030, #26304 ),
 .UNSPECIFIED., .F., .F. ) 
 B_SPLINE_CURVE_WITH_KNOTS ( ( 4, 4 ),
 ( 4.708531083176467291, 4.895802057644187855 ),
 .UNSPECIFIED. ) 
 CURVE ( )  GEOMETRIC_REPRESENTATION_ITEM ( )  RATIONAL_B_SPLINE_CURVE ( ( 1.000000000000000000, 0.9970795998553221295, 0.9970795998553221295, 1.000000000000000000 ) ) 
 REPRESENTATION_ITEM ( '' )  );
#22735 = CARTESIAN_POINT ( 'NONE',  ( 1.091512329210375665, -26.22489388037982749, 7.748216051605120391 ) ) ;
#22736 = CARTESIAN_POINT ( 'NONE',  ( 1.147042297102817354, -26.11394895998986598, 6.875671892026061549 ) ) ;
#22737 = VERTEX_POINT ( 'NONE', #20990 ) ;
#22738 = CARTESIAN_POINT ( 'NONE',  ( 23.43551384144531369, 3.792528780310672865, 3.105475544838504298 ) ) ;
#22739 = PLANE ( 'NONE',  #30013 ) ;
#22740 = CARTESIAN_POINT ( 'NONE',  ( 80.34143827441934604, 64.27643806731579446, 3.602832836245130288 ) ) ;
#22741 = CARTESIAN_POINT ( 'NONE',  ( 0.4741610271200560334, -32.84809465111302984, 6.894806418505347700 ) ) ;
#22742 = ORIENTED_EDGE ( 'NONE', *, *, #5627, .T. ) ;
#22743 = CARTESIAN_POINT ( 'NONE',  ( 78.08876170118931270, 64.69829802809502439, -3.164065397988976791 ) ) ;
#22745 = LINE ( 'NONE', #29517, #12490 ) ;
#22744 = CARTESIAN_POINT ( 'NONE',  ( 24.12522002703219570, 0.5066050462473785654, 5.093085906072658986 ) ) ;
#22746 = CARTESIAN_POINT ( 'NONE',  ( 81.55127126996082154, 61.75833066297040119, -1.907437723456241185 ) ) ;
#22747 = CARTESIAN_POINT ( 'NONE',  ( 79.34756916856697728, 63.37933396398980079, 3.765547211956733697 ) ) ;
#22748 = EDGE_CURVE ( 'NONE', #26805, #13108, #5755, .T. ) ;
#22749 = CARTESIAN_POINT ( 'NONE',  ( 3.551251297819357777, -26.64985754041175525, 6.800000000000000711 ) ) ;
#22750 = AXIS2_PLACEMENT_3D ( 'NONE', #19831, #7069, #38349 ) ;
#22751 = ADVANCED_FACE ( 'NONE', ( #20777 ), #27160, .F. ) ;
#22752 = CARTESIAN_POINT ( 'NONE',  ( 79.68325118717130806, 66.33239387230221951, 1.129532193886028102 ) ) ;
#22753 = CARTESIAN_POINT ( 'NONE',  ( -1.482088180267138622, -30.76652202637871625, 7.695279973900954751 ) ) ;
#22754 = CARTESIAN_POINT ( 'NONE',  ( 22.82155563815204502, -7.011124981618892527, 0.5620805258418327677 ) ) ;
#22755 = CARTESIAN_POINT ( 'NONE',  ( -62.96789184024967057, 35.54107112332027896, -6.131023528871231143 ) ) ;
#22756 = ORIENTED_EDGE ( 'NONE', *, *, #6630, .F. ) ;
#22757 = CARTESIAN_POINT ( 'NONE',  ( -79.24449270190245898, -6.613341267620478803, 5.568385975749495564 ) ) ;
#22758 = DIRECTION ( 'NONE',  ( -0.000000000000000000, -1.000000000000000000, -0.000000000000000000 ) ) ;
#22759 = AXIS2_PLACEMENT_3D ( 'NONE', #38193, #1167, #9994 ) ;
#22760 = EDGE_CURVE ( 'NONE', #22022, #13175, #22048, .T. ) ;
#22761 = DIRECTION ( 'NONE',  ( 1.000000000000000000, 0.000000000000000000, 0.000000000000000000 ) ) ;
#22762 = EDGE_LOOP ( 'NONE', ( #10345, #23759, #35923, #23706 ) ) ;
#22763 = CARTESIAN_POINT ( 'NONE',  ( -1.007170258006738095, -31.76429153184023946, 7.785593909369613819 ) ) ;
#22764 = CARTESIAN_POINT ( 'NONE',  ( 32.06915089713219658, 0.2527768776864406375, -4.727205254402804258 ) ) ;
#22765 = CYLINDRICAL_SURFACE ( 'NONE', #13468, 0.09010775117053029803 ) ;
#22766 = CARTESIAN_POINT ( 'NONE',  ( 3.848298546108438245, -32.20554951821143419, 6.894806418505343260 ) ) ;
#22767 = CARTESIAN_POINT ( 'NONE',  ( -16.34874870218063592, -25.49307895267003587, 6.800000000000000711 ) ) ;
#22768 = CARTESIAN_POINT ( 'NONE',  ( 5.195486027961456088, -29.75516796582088475, 6.989977667959438534 ) ) ;
#22769 = LINE ( 'NONE', #7501, #18732 ) ;
#22770 = CARTESIAN_POINT ( 'NONE',  ( 3.469506075866656936, -32.58990542741018714, 7.743886751744251562 ) ) ;
#22771 = DIRECTION ( 'NONE',  ( 1.000000000000000000, 0.000000000000000000, 0.000000000000000000 ) ) ;
#22772 = CARTESIAN_POINT ( 'NONE',  ( 25.04937939002015668, 1.718265418675629652, -4.340997593773719743 ) ) ;
#22773 = CARTESIAN_POINT ( 'NONE',  ( 35.50970222813752031, -1.197800581197451031, -5.486251443588301413 ) ) ;
#22774 = FACE_OUTER_BOUND ( 'NONE', #9606, .T. ) ;
#22775 = VERTEX_POINT ( 'NONE', #33568 ) ;
#22776 = CARTESIAN_POINT ( 'NONE',  ( 66.56983546066652480, 57.83423415266778278, 3.999917672784519596 ) ) ;
#22777 = VECTOR ( 'NONE', #27769, 1000.000000000000114 ) ;
#22778 = CARTESIAN_POINT ( 'NONE',  ( 86.17157777234386629, 0.6269314577163517255, 5.990399513018050293 ) ) ;
#22779 = CARTESIAN_POINT ( 'NONE',  ( 3.751251297819363728, -26.64985754041175525, 6.700000000000000178 ) ) ;
#22780 = ORIENTED_EDGE ( 'NONE', *, *, #14619, .F. ) ;
#22781 = CARTESIAN_POINT ( 'NONE',  ( 2.863753781421408462, -26.26893261765590282, 7.700536657684216024 ) ) ;
#22782 = SHAPE_DEFINITION_REPRESENTATION ( #28523, #29798 ) ;
#22783 = VECTOR ( 'NONE', #24976, 1000.000000000000000 ) ;
#22784 = PLANE ( 'NONE',  #33870 ) ;
#22785 = ORIENTED_EDGE ( 'NONE', *, *, #26729, .T. ) ;
#22786 = FILL_AREA_STYLE ('',( #25862 ) ) ;
#22787 = VERTEX_POINT ( 'NONE', #30464 ) ;
#22788 = CARTESIAN_POINT ( 'NONE',  ( 78.66571724150243483, 65.64011997358944939, -2.392122129321805790 ) ) ;
#22789 = CARTESIAN_POINT ( 'NONE',  ( 80.38728350982691495, 62.86383526565676760, 3.543129918318839611 ) ) ;
#22791 = VERTEX_POINT ( 'NONE', #2271 ) ;
#22790 = CARTESIAN_POINT ( 'NONE',  ( -1.289625865479514744, -31.18854093558072904, 6.866852738645443210 ) ) ;
#22792 = CARTESIAN_POINT ( 'NONE',  ( 25.62749773886924842, 1.970388730450938430, 4.206188844162269014 ) ) ;
#22793 = CARTESIAN_POINT ( 'NONE',  ( 0.9037396047256786025, -32.97806002456835017, 6.955226052476382925 ) ) ;
#22794 = FACE_OUTER_BOUND ( 'NONE', #12385, .T. ) ;
#22795 = CARTESIAN_POINT ( 'NONE',  ( 21.85643539959776760, -14.20048109512665135, 6.697783101734796851 ) ) ;
#22796 = CARTESIAN_POINT ( 'NONE',  ( 22.38767867107881671, 4.911711129367581918, -3.073573574929423735 ) ) ;
#22797 = ORIENTED_EDGE ( 'NONE', *, *, #26701, .F. ) ;
#22798 = CARTESIAN_POINT ( 'NONE',  ( 5.200364047366366371, -29.55642757665872722, 7.635761828346577573 ) ) ;
#22799 = EDGE_CURVE ( 'NONE', #15995, #12484, #14794, .T. ) ;
#22800 = ORIENTED_EDGE ( 'NONE', *, *, #22230, .F. ) ;
#22801 = EDGE_CURVE ( 'NONE', #16705, #14656, #40125, .T. ) ;
#22802 = CARTESIAN_POINT ( 'NONE',  ( -1.032131559973606727, -31.59312701384676103, 6.929923840112067523 ) ) ;
#22803 = DIRECTION ( 'NONE',  ( -0.000000000000000000, -0.000000000000000000, 1.000000000000000000 ) ) ;
#22804 = EDGE_CURVE ( 'NONE', #37085, #5530, #35150, .T. ) ;
#22805 = CARTESIAN_POINT ( 'NONE',  ( -71.81742943715566696, 1.311122306527585213, -9.960446608825028747 ) ) ;
#22806 = CARTESIAN_POINT ( 'NONE',  ( 6.921324086407803833, -24.55319635012989110, 6.700000000000000178 ) ) ;
#22807 = CARTESIAN_POINT ( 'NONE',  ( 11.65737507970504439, -32.06993018339339585, 6.800000000000000711 ) ) ;
#22808 = CARTESIAN_POINT ( 'NONE',  ( 80.74417485493698621, 64.10566034184276418, 3.509897338574980985 ) ) ;
#22809 = CARTESIAN_POINT ( 'NONE',  ( 84.13636243568421946, 2.973867306686137191, 1.134085816324387430 ) ) ;
#22810 = CARTESIAN_POINT ( 'NONE',  ( -43.84925787048184986, -39.21126558444150589, -9.800414904976365804 ) ) ;
#22811 = CARTESIAN_POINT ( 'NONE',  ( 2.924663588294490246, -32.84882548658472246, 7.730015791551949178 ) ) ;
#22812 = CARTESIAN_POINT ( 'NONE',  ( -1.641630102650725176, -30.19515113050700705, 7.680992449362118890 ) ) ;
#22813 = CIRCLE ( 'NONE', #8308, 12.80480339192541628 ) ;
#22814 = CARTESIAN_POINT ( 'NONE',  ( -65.04873975080082005, 34.92043383559660441, 6.752938550805159146 ) ) ;
#22815 = CARTESIAN_POINT ( 'NONE',  ( -0.3498495389373063036, -26.85764010844238214, 6.882085323592685100 ) ) ;
#22816 = DIRECTION ( 'NONE',  ( 1.000000000000000000, 0.000000000000000000, 0.000000000000000000 ) ) ;
#22817 = LINE ( 'NONE', #32483, #5594 ) ;
#22818 = AXIS2_PLACEMENT_3D ( 'NONE', #13210, #3018, #3974 ) ;
#22819 = CARTESIAN_POINT ( 'NONE',  ( 68.95366548541680629, 59.44408286695458798, 3.907754234428187257 ) ) ;
#22820 = CARTESIAN_POINT ( 'NONE',  ( 30.51641733573469040, -0.1366954951678319985, 4.969222986220390048 ) ) ;
#22821 = CARTESIAN_POINT ( 'NONE',  ( -17.07867591359219617, -26.64985754041175525, 6.700000000000000178 ) ) ;
#22822 = CARTESIAN_POINT ( 'NONE',  ( 87.25792211136258913, 0.3454849704027515567, -4.698443967043519187 ) ) ;
#22823 = ORIENTED_EDGE ( 'NONE', *, *, #3800, .F. ) ;
#22825 = CARTESIAN_POINT ( 'NONE',  ( 4.817241837858415643, -30.92832464666959780, 6.949473656533212917 ) ) ;
#22824 = CARTESIAN_POINT ( 'NONE',  ( 78.75316082766835279, 66.06368344870412557, -1.496866203714572574 ) ) ;
#22826 = CARTESIAN_POINT ( 'NONE',  ( -1.230064425333113221, -27.65618090132562301, 6.951256099901589991 ) ) ;
#22827 = VERTEX_POINT ( 'NONE', #31843 ) ;
#22828 = DIRECTION ( 'NONE',  ( -0.000000000000000000, -0.000000000000000000, 1.000000000000000000 ) ) ;
#22829 = CARTESIAN_POINT ( 'NONE',  ( -71.98686916902434518, 0.1712994517134147909, 9.947269908901157365 ) ) ;
#22831 = ORIENTED_EDGE ( 'NONE', *, *, #10918, .T. ) ;
#22830 = ORIENTED_EDGE ( 'NONE', *, *, #40516, .F. ) ;
#22832 = CARTESIAN_POINT ( 'NONE',  ( 80.59816347408047932, 62.94305116675459288, -3.503057693382716664 ) ) ;
#22833 = AXIS2_PLACEMENT_3D ( 'NONE', #28997, #800, #13332 ) ;
#22834 = CARTESIAN_POINT ( 'NONE',  ( -8.448748702180639114, -26.64985754041175525, 6.700000000000000178 ) ) ;
#22835 = VECTOR ( 'NONE', #9358, 1000.000000000000000 ) ;
#22836 = CARTESIAN_POINT ( 'NONE',  ( 21.79934511777053174, 1.490787985410582994, 6.749058457536040834 ) ) ;
#22837 = VERTEX_POINT ( 'NONE', #4057 ) ;
#22838 = AXIS2_PLACEMENT_3D ( 'NONE', #38837, #11585, #30560 ) ;
#22839 = CARTESIAN_POINT ( 'NONE',  ( 78.68849923766543952, 66.05725436416432217, -1.045986116561646639 ) ) ;
#22840 = CARTESIAN_POINT ( 'NONE',  ( -0.06024744239608810503, -32.47858221735037887, 7.784476445165072533 ) ) ;
#22842 = CARTESIAN_POINT ( 'NONE',  ( 4.381563664431031846, -27.47916279290977570, 7.754798119455333705 ) ) ;
#22841 = CARTESIAN_POINT ( 'NONE',  ( 4.620198719170100610, -31.31197426661971761, 6.894806418505346812 ) ) ;
#22843 = CARTESIAN_POINT ( 'NONE',  ( -64.08758708074093136, 43.61223004741319897, -0.9999999999999937828 ) ) ;
#22844 = CARTESIAN_POINT ( 'NONE',  ( 69.75093826875801994, 59.10798165618643907, 3.985452289341158139 ) ) ;
#22845 = CARTESIAN_POINT ( 'NONE',  ( 24.11137768457082942, 2.995069816642412786, -3.734747807212182913 ) ) ;
#22846 = ORIENTED_EDGE ( 'NONE', *, *, #13776, .F. ) ;
#22847 = CARTESIAN_POINT ( 'NONE',  ( 2.333773081392421567, -33.01214383003427599, 7.737115613922531665 ) ) ;
#22848 = ORIENTED_EDGE ( 'NONE', *, *, #29344, .F. ) ;
#22849 = CARTESIAN_POINT ( 'NONE',  ( 21.85643539959777470, -4.742028430345498258, -11.91557605213902882 ) ) ;
#22851 = ADVANCED_FACE ( 'NONE', ( #26271 ), #29353, .F. ) ;
#22850 = CARTESIAN_POINT ( 'NONE',  ( 21.66074814249151714, 7.048403176780774437, 2.215087588513221758E-12 ) ) ;
#22852 = CARTESIAN_POINT ( 'NONE',  ( -8.248748702180632719, -25.49307895267003587, 6.800000000000000711 ) ) ;
#22853 = CARTESIAN_POINT ( 'NONE',  ( 81.46069228692957154, 61.55470069442174719, 1.644402879622030911 ) ) ;
#22854 = CARTESIAN_POINT ( 'NONE',  ( 88.65680102019307185, -1.418189719613276223, -2.767552868364703045 ) ) ;
#22855 = ORIENTED_EDGE ( 'NONE', *, *, #32792, .T. ) ;
#22856 = CARTESIAN_POINT ( 'NONE',  ( 14.68773611674814283, 12.90757323260954514, 2.500000034667914761 ) ) ;
#22857 = CARTESIAN_POINT ( 'NONE',  ( 31.37338404834114769, -3.012165633454263247, 5.102973367540887928 ) ) ;
#22858 = CARTESIAN_POINT ( 'NONE',  ( 5.078732710124126193, -29.18678336023061348, 6.969307238440507035 ) ) ;
#22859 = CARTESIAN_POINT ( 'NONE',  ( 36.42081795466733496, -3.114981983614129035, -5.890747501273418507 ) ) ;
#22860 = DIRECTION ( 'NONE',  ( 1.000000000000000000, 0.000000000000000000, 0.000000000000000000 ) ) ;
#22861 = CARTESIAN_POINT ( 'NONE',  ( 84.92084393738451809, 1.980781149894611959, 4.774541556935223419 ) ) ;
#22862 = PRODUCT_DEFINITION_FORMATION_WITH_SPECIFIED_SOURCE ( 'ANY', '', #19157, .NOT_KNOWN. ) ;
#22863 = CARTESIAN_POINT ( 'NONE',  ( -74.68562510149382661, -2.717749937412478722, 10.59137344923616375 ) ) ;
#22864 = CARTESIAN_POINT ( 'NONE',  ( 1.300000000000000044, -0.5999999999999994227, -4.250000000000000000 ) ) ;
#22865 = VECTOR ( 'NONE', #30341, 999.9999999999998863 ) ;
#22866 = VECTOR ( 'NONE', #30365, 1000.000000000000000 ) ;
#22867 = DIRECTION ( 'NONE',  ( -0.000000000000000000, -1.000000000000000000, -0.000000000000000000 ) ) ;
#22868 = CARTESIAN_POINT ( 'NONE',  ( 32.90341992358483481, -3.215921544857364811, 5.341772469908477206 ) ) ;
#22869 = ORIENTED_EDGE ( 'NONE', *, *, #24214, .F. ) ;
#22870 = ORIENTED_EDGE ( 'NONE', *, *, #21355, .F. ) ;
#22871 = CARTESIAN_POINT ( 'NONE',  ( 37.10938198393888854, -2.404265875854591172, 5.951784697920204259 ) ) ;
#22872 = CARTESIAN_POINT ( 'NONE',  ( 1.665030044868864634, -33.05676478451892564, 7.783750581861600182 ) ) ;
#22873 = ADVANCED_FACE ( 'NONE', ( #3656 ), #22784, .T. ) ;
#22874 = DIRECTION ( 'NONE',  ( 0.000000000000000000, 0.000000000000000000, -1.000000000000000000 ) ) ;
#22875 = ORIENTED_EDGE ( 'NONE', *, *, #40292, .T. ) ;
#22876 = ORIENTED_EDGE ( 'NONE', *, *, #7526, .T. ) ;
#22877 = DIRECTION ( 'NONE',  ( 0.000000000000000000, 0.000000000000000000, -1.000000000000000000 ) ) ;
#22878 = CARTESIAN_POINT ( 'NONE',  ( 2.294856720451861953, -26.12078399496891734, 7.635761828346576685 ) ) ;
#22879 = AXIS2_PLACEMENT_3D ( 'NONE', #18665, #12700, #28352 ) ;
#22880 = ORIENTED_EDGE ( 'NONE', *, *, #13488, .F. ) ;
#22881 = CYLINDRICAL_SURFACE ( 'NONE', #35278, 15.73502530973474478 ) ;
#22882 = CARTESIAN_POINT ( 'NONE',  ( 3.837038864732983612, -32.34206510565962844, 6.875780273367530171 ) ) ;
#22883 = VERTEX_POINT ( 'NONE', #13497 ) ;
#22884 = CARTESIAN_POINT ( 'NONE',  ( 78.98807859296742606, 66.20728402696080650, -1.114595100209339495 ) ) ;
#22885 = ADVANCED_FACE ( 'NONE', ( #10199 ), #35742, .F. ) ;
#22886 = VECTOR ( 'NONE', #578, 1000.000000000000000 ) ;
#22887 = DIRECTION ( 'NONE',  ( 0.000000000000000000, 0.000000000000000000, 1.000000000000000000 ) ) ;
#22888 = ORIENTED_EDGE ( 'NONE', *, *, #11586, .F. ) ;
#22889 = CARTESIAN_POINT ( 'NONE',  ( 75.05654786057638717, 62.45444674818786268, -3.685888554891597835 ) ) ;
#22891 = CYLINDRICAL_SURFACE ( 'NONE', #15039, 27.95745752244933868 ) ;
#22890 = CARTESIAN_POINT ( 'NONE',  ( 2.425674012770692833, -26.14588693425077892, 6.865706122441728176 ) ) ;
#22892 = CARTESIAN_POINT ( 'NONE',  ( 76.81831744871803380, 63.08285468194208079, 3.722835383484662142 ) ) ;
#22893 = VECTOR ( 'NONE', #25951, 1000.000000000000000 ) ;
#22894 = CARTESIAN_POINT ( 'NONE',  ( 4.407694157253644107, -27.51309448911002065, 6.876076431790002275 ) ) ;
#22895 = B_SPLINE_CURVE_WITH_KNOTS ( 'NONE', 3,
 ( #34601, #24485, #18092, #30685, #34195, #27772, #37041, #18927 ),
 .UNSPECIFIED., .F., .F.,
 ( 4, 2, 2, 4 ),
 ( -2.215204784179636180E-05, 0.0001932311667254880505, 0.0004086143812927724899, 0.0008393808104273412602 ),
 .UNSPECIFIED. ) ;
#22896 = CARTESIAN_POINT ( 'NONE',  ( 1.822194502883780931, -26.07228119081829476, 7.754798119455333705 ) ) ;
#22898 = EDGE_CURVE ( 'NONE', #23332, #5710, #18736, .T. ) ;
#22897 = CARTESIAN_POINT ( 'NONE',  ( -1.799583860900191734, -29.58343279012807159, 7.635761828346577573 ) ) ;
#22899 = LINE ( 'NONE', #32778, #8997 ) ;
#22900 = CARTESIAN_POINT ( 'NONE',  ( 81.16877391194421421, 61.30368580354083008, 1.027726681410876308 ) ) ;
#22901 = CARTESIAN_POINT ( 'NONE',  ( -0.1134167689795140821, -32.56329063961136683, 6.867280401193707640 ) ) ;
#22902 = CARTESIAN_POINT ( 'NONE',  ( 27.13744335700502219, 0.8961374054434056990, -5.485310518450965844 ) ) ;
#22903 = CARTESIAN_POINT ( 'NONE',  ( -1.699609906766908818, -29.57706174694755674, 7.761939382804113663 ) ) ;
#22904 = CARTESIAN_POINT ( 'NONE',  ( 3.578914694166553723, -26.73600263956173606, 6.959317978105163505 ) ) ;
#22905 = DIRECTION ( 'NONE',  ( -0.000000000000000000, -0.000000000000000000, -1.000000000000000000 ) ) ;
#22906 = LINE ( 'NONE', #26594, #107 ) ;
#22907 = CARTESIAN_POINT ( 'NONE',  ( 3.935268700167234623, -26.87636050501711793, 7.643192810543824045 ) ) ;
#22908 = CARTESIAN_POINT ( 'NONE',  ( 37.10285757261533490, -2.625508518994315477, -5.990196095338164106 ) ) ;
#22909 = CARTESIAN_POINT ( 'NONE',  ( 1.089753260929022360, -32.91465995119874322, 7.779495906702012853 ) ) ;
#22910 = PLANE ( 'NONE',  #16067 ) ;
#22911 = CARTESIAN_POINT ( 'NONE',  ( 3.313913495458963077, -32.56269280434947433, 7.774064877406527074 ) ) ;
#22912 = PLANE ( 'NONE',  #30267 ) ;
#22913 = CARTESIAN_POINT ( 'NONE',  ( 21.90967695140060201, -12.75691164195780303, -2.500000000000000444 ) ) ;
#22914 = EDGE_CURVE ( 'NONE', #14282, #7409, #13480, .T. ) ;
#22915 = CARTESIAN_POINT ( 'NONE',  ( -63.06901714727352015, 38.60153782280345780, -4.000000000000000888 ) ) ;
#22916 = CARTESIAN_POINT ( 'NONE',  ( 30.84950422756433142, -2.934832344082245026, 5.021209251427320552 ) ) ;
#22917 = ORIENTED_EDGE ( 'NONE', *, *, #18684, .T. ) ;
#22918 = CARTESIAN_POINT ( 'NONE',  ( 30.74493630087459906, 0.4681640684078945958, 4.860621472976927038 ) ) ;
#22919 = DIRECTION ( 'NONE',  ( -0.000000000000000000, -1.000000000000000000, -0.000000000000000000 ) ) ;
#22920 = CARTESIAN_POINT ( 'NONE',  ( 67.93540907064681278, 58.63163702635943508, -3.982418445723137967 ) ) ;
#22921 = VECTOR ( 'NONE', #20292, 1000.000000000000000 ) ;
#22922 = CARTESIAN_POINT ( 'NONE',  ( 3.076197136650148156, -26.35167677831728383, 6.951256099901586438 ) ) ;
#22923 = ORIENTED_EDGE ( 'NONE', *, *, #8590, .F. ) ;
#22924 = CARTESIAN_POINT ( 'NONE',  ( -0.4487487021806388365, -26.64985754041175525, 6.700000000000000178 ) ) ;
#22925 = CARTESIAN_POINT ( 'NONE',  ( -18.48280404870591553, -63.98126818465317456, -2.500000000000000000 ) ) ;
#22926 = CARTESIAN_POINT ( 'NONE',  ( 23.04163317972315994, 3.256728484989337868, 3.973781910508482174 ) ) ;
#22927 = CARTESIAN_POINT ( 'NONE',  ( 0.4796627190948448138, -26.28970783387809007, 7.651421919295143148 ) ) ;
#22928 = CARTESIAN_POINT ( 'NONE',  ( -1.449731085724313751, -28.29053751634241820, 6.863904403958575706 ) ) ;
#22929 =( REPRESENTATION_RELATIONSHIP ('NONE','NONE', #24012, #32460 ) REPRESENTATION_RELATIONSHIP_WITH_TRANSFORMATION ( #27475 )SHAPE_REPRESENTATION_RELATIONSHIP( ) );
#22930 = EDGE_CURVE ( 'NONE', #7709, #26563, #29271, .T. ) ;
#22931 = EDGE_CURVE ( 'NONE', #8713, #34290, #7123, .T. ) ;
#22932 = CARTESIAN_POINT ( 'NONE',  ( 3.497962998608483698, -26.56680986448170501, 6.875671892026061549 ) ) ;
#22933 = DIRECTION ( 'NONE',  ( -0.000000000000000000, -0.000000000000000000, -1.000000000000000000 ) ) ;
#22934 = VERTEX_POINT ( 'NONE', #26070 ) ;
#22935 = EDGE_CURVE ( 'NONE', #20708, #38802, #38200, .T. ) ;
#22936 = CARTESIAN_POINT ( 'NONE',  ( 22.18636049064522453, 5.270353752318829521, 3.074731245731978646 ) ) ;
#22937 = CARTESIAN_POINT ( 'NONE',  ( 82.18775271763095702, 62.23297483488567394, -1.000000000000000000 ) ) ;
#22938 = CARTESIAN_POINT ( 'NONE',  ( 15.01546246723575173, -4.177556355646068198, 2.539460141531804105 ) ) ;
#22939 = CARTESIAN_POINT ( 'NONE',  ( 81.14234681338471944, 61.29401378075402818, 1.159471704397071035 ) ) ;
#22940 = CLOSED_SHELL ( 'NONE', ( #34578, #2805, #2694, #11871, #32109, #21545, #10687, #26953, #22751, #10592, #5242, #36723, #12884, #16593, #15200, #22851, #4149, #6070, #32381, #28953, #6018, #27933, #4392, #8735, #14947, #6304, #3770, #27565, #32325, #12226, #24206, #7907, #13168, #12009, #31720, #26686, #36963, #32380, #23961, #22719, #19215, #31259, #27697, #38164, #39493, #36017, #11744, #4791, #38833, #29211, #19332, #14118, #16952, #37094, #8769, #9579, #2590, #26773, #16214, #40104, #34008, #36451, #1798, #25153, #14175, #13214, #34283, #36539, #11693, #18872, #3344, #2211, #8584, #2591, #26920, #24430, #32548, #6105, #8109, #13192, #35280, #3511, #39640, #35002, #19895, #12347, #11360, #5687, #26532, #21821, #27845, #20435, #5069, #21695, #30211, #19734, #16191, #39440, #34062, #6058, #39508, #8816, #26776, #27227, #5263, #21022, #15150, #22689, #22119, #24018, #14860, #36705, #25991, #5869, #33213, #31942, #33762, #4575, #26239, #29568, #30450, #2577, #13487, #6890, #36259, #26832, #26236, #4258, #21941, #33869, #4075, #1502, #11938, #36917, #16348, #8687, #16581, #5901, #35362, #34773, #36196, #33291, #8304, #37690, #18215, #31576, #284, #5111, #10615, #4169, #16457, #7302, #11349, #16653, #15431, #23244, #36991, #4331, #9385, #13299, #24665, #29146, #7172, #27007, #10259, #38334, #1136, #19545, #19202, #27471, #33715, #20636, #16411, #36535, #5563, #19542, #14292, #1549, #24261, #15385, #20716, #9479, #37744, #11506, #30300, #29121, #30314, #25191, #24475, #8830, #29071, #11190, #6276, #6939, #8626, #15189, #19888, #7163, #16184, #1048, #29846, #1812, #4707, #31868, #25254, #6334, #10875, #25437, #14076, #4658, #4612, #29048, #30374, #35762, #35231, #6492, #16139, #3030, #16913, #33488, #38967, #27793, #17313, #13726, #298, #30137, #18365, #688, #1201, #28926, #14623 ) ) ;
#22941 = CARTESIAN_POINT ( 'NONE',  ( 0.4695943777967604427, -26.29347754267606874, 7.697032948437506406 ) ) ;
#22942 = ORIENTED_EDGE ( 'NONE', *, *, #4539, .T. ) ;
#22943 = CARTESIAN_POINT ( 'NONE',  ( 77.75442706423145012, 65.27774734742538953, -2.313798345564205494 ) ) ;
#22945 = CARTESIAN_POINT ( 'NONE',  ( 14.61824258762769091, -4.523863395544843513, -2.500000000000095035 ) ) ;
#22944 = CARTESIAN_POINT ( 'NONE',  ( 25.38719211221763317, 0.7154116930338988434, 4.601124151639230497 ) ) ;
#22946 = CARTESIAN_POINT ( 'NONE',  ( 78.68499968550160872, 66.05476829360677016, -1.077711394953983604 ) ) ;
#22947 = CARTESIAN_POINT ( 'NONE',  ( 78.00211021922338261, 65.46497694724934036, 2.177161688561012998 ) ) ;
#22948 = CARTESIAN_POINT ( 'NONE',  ( -69.92837670882107659, -0.7829914368874778541, 3.916079783099621014 ) ) ;
#22949 = EDGE_CURVE ( 'NONE', #19287, #24258, #17082, .T. ) ;
#22950 = CARTESIAN_POINT ( 'NONE',  ( 81.16955088369260807, 61.30397035488353197, 1.005837412005772258 ) ) ;
#22952 = ORIENTED_EDGE ( 'NONE', *, *, #21391, .F. ) ;
#22951 = CARTESIAN_POINT ( 'NONE',  ( 3.301837905240542881, -32.68206207414233688, 7.013842709614101167 ) ) ;
#22953 = CARTESIAN_POINT ( 'NONE',  ( 24.43246502961036626, -0.4583524411608039251, -6.968550363799582925 ) ) ;
#22954 = CARTESIAN_POINT ( 'NONE',  ( -1.434056508659582674, -31.14254555582535389, 7.387053503561885393 ) ) ;
#22955 = ORIENTED_EDGE ( 'NONE', *, *, #40511, .T. ) ;
#22956 = CARTESIAN_POINT ( 'NONE',  ( -74.63738614184299536, -2.659024657488486376, 9.335863256658281983 ) ) ;
#22957 = CARTESIAN_POINT ( 'NONE',  ( -1.642550015356792681, -30.60663237321507069, 7.013842709614101167 ) ) ;
#22958 = ORIENTED_EDGE ( 'NONE', *, *, #32968, .F. ) ;
#22959 = CARTESIAN_POINT ( 'NONE',  ( -40.44874870218063734, -26.64985754041175525, 6.700000000000000178 ) ) ;
#22960 = CARTESIAN_POINT ( 'NONE',  ( 23.38513527390059821, 3.559322506240827799, -3.095448560026594631 ) ) ;
#22961 = CARTESIAN_POINT ( 'NONE',  ( -1.749609906766908640, -29.56993018339339940, 7.800000000000000711 ) ) ;
#22962 = DIRECTION ( 'NONE',  ( 1.000000000000000000, 0.000000000000000000, 0.000000000000000000 ) ) ;
#22963 = CARTESIAN_POINT ( 'NONE',  ( 5.112182647635235000, -30.35077483426318778, 6.903112506833887885 ) ) ;
#22964 = CARTESIAN_POINT ( 'NONE',  ( 8.290806648384990041, -10.90558813203967148, 6.000000000000000000 ) ) ;
#22965 = DIRECTION ( 'NONE',  ( 1.000000000000000000, 0.000000000000000000, 0.000000000000000000 ) ) ;
#22966 = EDGE_CURVE ( 'NONE', #33369, #38905, #32058, .T. ) ;
#22967 = CYLINDRICAL_SURFACE ( 'NONE', #5929, 5.000000000000000000 ) ;
#22968 = CARTESIAN_POINT ( 'NONE',  ( 22.19836525915095393, 0.7666314114482586373, -6.808643381459575039 ) ) ;
#22969 = CARTESIAN_POINT ( 'NONE',  ( 35.52266373076683692, -1.204347071998821628, -5.489450149774045329 ) ) ;
#22970 = AXIS2_PLACEMENT_3D ( 'NONE', #15798, #34154, #2856 ) ;
#22971 = CARTESIAN_POINT ( 'NONE',  ( 2.737092283054774811, -32.91287029198328185, 7.013842709614101167 ) ) ;
#22972 = ORIENTED_EDGE ( 'NONE', *, *, #14119, .F. ) ;
#22973 =( BOUNDED_SURFACE ( )  B_SPLINE_SURFACE ( 3, 2, ( 
 ( #25049, #13696, #1362 ),
 ( #4050, #3649, #38596 ),
 ( #32441, #28945, #35143 ),
 ( #748, #4239, #38989 ) ),
 .UNSPECIFIED., .F., .F., .F. ) 
 B_SPLINE_SURFACE_WITH_KNOTS ( ( 4, 4 ),
 ( 3, 3 ),
 ( 4.564251139902668619, 4.712388980384689674 ),
 ( 0.000000000000000000, 1.000000000000000000 ),
 .UNSPECIFIED. ) 
 GEOMETRIC_REPRESENTATION_ITEM ( )  RATIONAL_B_SPLINE_SURFACE ( (
 ( 1.000000000000000000, 0.6872206705710377506, 1.000000000000000000),
 ( 1.000000000000000000, 0.6938961412926133443, 1.000000000000000000),
 ( 1.000000000000000000, 0.7005474459265356169, 1.000000000000000000),
 ( 1.000000000000000000, 0.7071067811865475727, 1.000000000000000000) ) ) 
 REPRESENTATION_ITEM ( '' )  SURFACE ( )  );
#22974 = ORIENTED_EDGE ( 'NONE', *, *, #6814, .T. ) ;
#22975 = CARTESIAN_POINT ( 'NONE',  ( 66.55809347730310321, 57.86716763633229021, 3.999802976172706082 ) ) ;
#22977 = EDGE_CURVE ( 'NONE', #4684, #30447, #30598, .T. ) ;
#22976 = CARTESIAN_POINT ( 'NONE',  ( 87.32347380307142259, -1.421525632644524251, -4.720772940814831564 ) ) ;
#22978 = VERTEX_POINT ( 'NONE', #36338 ) ;
#22979 = CARTESIAN_POINT ( 'NONE',  ( -74.18786092369259677, 6.905699905533330352, -10.73326951011580555 ) ) ;
#22980 = PRODUCT_CONTEXT ( 'NONE', #1895, 'mechanical' ) ;
#22981 = CARTESIAN_POINT ( 'NONE',  ( 2.919829066420930541, -26.30113654672046408, 7.781480525794719050 ) ) ;
#22982 = EDGE_CURVE ( 'NONE', #2693, #34412, #7566, .T. ) ;
#22983 = CARTESIAN_POINT ( 'NONE',  ( -66.99872204295122913, 28.48507918597134037, -6.999999999999999112 ) ) ;
#22984 = AXIS2_PLACEMENT_3D ( 'NONE', #2242, #9405, #18469 ) ;
#22985 = VERTEX_POINT ( 'NONE', #39833 ) ;
#22986 = LINE ( 'NONE', #16774, #445 ) ;
#22987 = VERTEX_POINT ( 'NONE', #23372 ) ;
#22988 = CARTESIAN_POINT ( 'NONE',  ( 79.26327435592848758, 64.69753611046425590, -3.458772244351173697 ) ) ;
#22989 = CARTESIAN_POINT ( 'NONE',  ( 33.79294173806484736, -4.878189388823929384, 3.391004255377942922 ) ) ;
#22990 = CARTESIAN_POINT ( 'NONE',  ( 79.16440527908353886, 64.96746831917783993, 3.289664858626308419 ) ) ;
#22991 = CARTESIAN_POINT ( 'NONE',  ( -1.271991893282980790, -31.22067102502625957, 6.887041543973314361 ) ) ;
#22992 = CARTESIAN_POINT ( 'NONE',  ( -27.07867591359219972, -26.64985754041175525, 6.700000000000000178 ) ) ;
#22993 = VECTOR ( 'NONE', #33172, 999.9999999999998863 ) ;
#22994 = ADVANCED_BREP_SHAPE_REPRESENTATION ( '', ( #26090, #30744 ), #40552 ) ;
#22995 = DIRECTION ( 'NONE',  ( -0.000000000000000000, -1.000000000000000000, -0.000000000000000000 ) ) ;
#22996 = CARTESIAN_POINT ( 'NONE',  ( 1.123288416806107026, -32.92059484209399045, 7.635761828346577573 ) ) ;
#22997 = CARTESIAN_POINT ( 'NONE',  ( 33.78816593493456111, -4.856674916897421035, -3.444637928637498181 ) ) ;
#22998 = CARTESIAN_POINT ( 'NONE',  ( -0.4487487021806388365, -25.49307895267003587, 6.700000000000000178 ) ) ;
#22999 = ORIENTED_EDGE ( 'NONE', *, *, #24548, .F. ) ;
#23000 = CARTESIAN_POINT ( 'NONE',  ( 74.91297039797925095, 63.41901279415932891, -3.016929835169668728 ) ) ;
#23001 = DIRECTION ( 'NONE',  ( 0.000000000000000000, 0.000000000000000000, 1.000000000000000000 ) ) ;
#23002 = CARTESIAN_POINT ( 'NONE',  ( 4.281682929012584182, -27.35702998321412593, 7.693875151218753317 ) ) ;
#23003 = CARTESIAN_POINT ( 'NONE',  ( -72.05444927908816055, 4.856418035946385103, -9.936797814648945959 ) ) ;
#23004 = CARTESIAN_POINT ( 'NONE',  ( 5.144476794586663182, -28.94681611416600830, 7.638132480492515697 ) ) ;
#23005 = CYLINDRICAL_SURFACE ( 'NONE', #12266, 3.399999999999999911 ) ;
#23006 = CARTESIAN_POINT ( 'NONE',  ( 81.32112198246272783, 62.31825444738112907, 2.836177733672701429 ) ) ;
#23007 = CARTESIAN_POINT ( 'NONE',  ( 86.38495421312710221, -0.4360953479145894263, -5.826368990767747391 ) ) ;
#23008 = CARTESIAN_POINT ( 'NONE',  ( 24.75848867132678421, 3.019268511056711901, -3.350244135560401126 ) ) ;
#23009 = CARTESIAN_POINT ( 'NONE',  ( 2.918216031185672410, -32.85122898407183101, 7.743886751744253338 ) ) ;
#23010 = CARTESIAN_POINT ( 'NONE',  ( 5.123097946374971734, -30.30141562551846235, 7.750000000000000888 ) ) ;
#23011 = AXIS2_PLACEMENT_3D ( 'NONE', #32065, #3666, #13715 ) ;
#23012 = ADVANCED_FACE ( 'NONE', ( #26467 ), #36141, .F. ) ;
#23013 = CARTESIAN_POINT ( 'NONE',  ( 1.799419147782851391, -26.17136002503600523, 7.774064877406527962 ) ) ;
#23014 = DIRECTION ( 'NONE',  ( 1.000000000000000000, 0.000000000000000000, 0.000000000000000000 ) ) ;
#23015 = DIRECTION ( 'NONE',  ( -1.000000000000000000, 0.000000000000000000, 0.000000000000000000 ) ) ;
#23016 = VERTEX_POINT ( 'NONE', #39205 ) ;
#23017 = CARTESIAN_POINT ( 'NONE',  ( 32.78029040100151548, -0.9298081016050898651, 5.322555130032219139 ) ) ;
#23018 = ADVANCED_FACE ( 'NONE', ( #14295 ), #36740, .F. ) ;
#23019 = CARTESIAN_POINT ( 'NONE',  ( -64.08758708074093136, 41.64075302391485423, -2.960467334047197419 ) ) ;
#23021 = EDGE_CURVE ( 'NONE', #22465, #13345, #28627, .T. ) ;
#23020 = CARTESIAN_POINT ( 'NONE',  ( 84.98726364908050357, 2.895996327189970021, 0.3032432708941606436 ) ) ;
#23022 = VECTOR ( 'NONE', #5872, 1000.000000000000000 ) ;
#23024 = CARTESIAN_POINT ( 'NONE',  ( 4.826555071938813946, -30.90675198375193844, 7.013842709614101167 ) ) ;
#23023 = CARTESIAN_POINT ( 'NONE',  ( 79.78769048662040575, 65.07306089581300057, -3.312281065658527091 ) ) ;
#23025 = CARTESIAN_POINT ( 'NONE',  ( 1.700390093233090871, -29.56993018339339940, -6.000000000000001776 ) ) ;
#23026 = CARTESIAN_POINT ( 'NONE',  ( -4.248748702180636272, -26.64985754041175525, 6.800000000000000711 ) ) ;
#23027 = VERTEX_POINT ( 'NONE', #23576 ) ;
#23028 = CARTESIAN_POINT ( 'NONE',  ( 4.907464300517769829, -30.69894525369553762, 7.695279973900954751 ) ) ;
#23029 = ADVANCED_FACE ( 'NONE', ( #30580 ), #33258, .F. ) ;
#23030 = ORIENTED_EDGE ( 'NONE', *, *, #35718, .F. ) ;
#23031 = CARTESIAN_POINT ( 'NONE',  ( -80.13811754935157694, -6.651623698664113071, 3.918677847151820881 ) ) ;
#23032 = EDGE_CURVE ( 'NONE', #4122, #12351, #35861, .T. ) ;
#23033 = ORIENTED_EDGE ( 'NONE', *, *, #30978, .F. ) ;
#23034 = CARTESIAN_POINT ( 'NONE',  ( 78.60310727342863402, 65.99661392892440404, -1.312782405654899121 ) ) ;
#23035 = CARTESIAN_POINT ( 'NONE',  ( 3.551251297819357777, -26.64985754041175525, 6.800000000000000711 ) ) ;
#23036 = CARTESIAN_POINT ( 'NONE',  ( 25.23678314328794059, 2.025140460799608189, 4.185677819315343662 ) ) ;
#23038 = VERTEX_POINT ( 'NONE', #23964 ) ;
#23037 = EDGE_LOOP ( 'NONE', ( #36726, #36527, #32521, #33328 ) ) ;
#23039 = CIRCLE ( 'NONE', #21093, 3.000000000000002665 ) ;
#23040 = DIRECTION ( 'NONE',  ( -0.000000000000000000, -0.000000000000000000, -1.000000000000000000 ) ) ;
#23042 = CARTESIAN_POINT ( 'NONE',  ( 3.974925472835492801, -32.23009724712022006, 7.670465701733754749 ) ) ;
#23041 = CARTESIAN_POINT ( 'NONE',  ( -59.01947560891952804, 27.90920910948504385, -6.147301388271595890 ) ) ;
#23043 = CARTESIAN_POINT ( 'NONE',  ( -22.24874870218063450, -25.49307895267003587, 6.700000000000000178 ) ) ;
#23044 = B_SPLINE_SURFACE_WITH_KNOTS ( 'NONE', 5, 3, ( 
 ( #3527, #27995, #12965, #40539, #30904, #24922, #2712 ),
 ( #9253, #21832, #31308, #31919, #38469, #13569, #4519 ),
 ( #19752, #35617, #3729, #35814, #17039, #32329, #39069 ),
 ( #10272, #4126, #29223, #16639, #23053, #1037, #7590 ),
 ( #26344, #26141, #38673, #25730, #26534, #1433, #10472 ),
 ( #23248, #32135, #38875, #22850, #13966, #6992, #13775 ),
 ( #20144, #7389, #3934, #19944, #25935, #32523, #629 ),
 ( #29617, #22451, #16452, #32724, #38274, #35020, #13171 ),
 ( #10069, #29025, #828, #4323, #6795, #16844, #29426 ),
 ( #19349, #1240, #16253, #10667, #28824, #22654, #35222 ),
 ( #35423, #13360, #19559, #7191, #20338, #11464, #14360 ),
 ( #29815, #33121, #39274, #20535, #30023, #11261, #17850 ),
 ( #10901, #20995, #26968, #26568, #4550, #14593, #14397 ) ),
 .UNSPECIFIED., .F., .F., .F.,
 ( 6, 2, 5, 6 ),
 ( 4, 1, 1, 1, 4 ),
 ( 0.000000000000000000, 0.5000000000000000000, 1.000000000000000000, 1.064435095764829642 ),
 ( -0.001274899269766986438, 0.0006125503651162966887, 0.002499999999999579815, 0.004387449634882863159, 0.006274899269766145635 ),
 .UNSPECIFIED. ) ;
#23045 = CARTESIAN_POINT ( 'NONE',  ( 70.53871541878200446, 60.47550293342311534, 3.775670717450619218 ) ) ;
#23046 = CARTESIAN_POINT ( 'NONE',  ( 24.14380846906243150, 3.078890981682416150, -3.628619729749268608 ) ) ;
#23047 = VERTEX_POINT ( 'NONE', #8522 ) ;
#23048 = CARTESIAN_POINT ( 'NONE',  ( 2.343537225896454856, -33.01033157941493101, 7.697032948437507294 ) ) ;
#23049 = B_SPLINE_CURVE_WITH_KNOTS ( 'NONE', 3,
 ( #12469, #18431, #2417, #24618, #31422, #25039, #15142, #24830, #36768, #21952 ),
 .UNSPECIFIED., .F., .F.,
 ( 4, 3, 3, 4 ),
 ( 1.939479807224432123E-18, 3.025570593003372544E-05, 6.051145698344380657E-05, 6.468151674593654050E-05 ),
 .UNSPECIFIED. ) ;
#23050 = ORIENTED_EDGE ( 'NONE', *, *, #32614, .F. ) ;
#23051 = CARTESIAN_POINT ( 'NONE',  ( 21.85643539959776049, -3.417000210761661272, 14.19984240075801374 ) ) ;
#23052 = CIRCLE ( 'NONE', #22413, 0.1000000000000028644 ) ;
#23053 = CARTESIAN_POINT ( 'NONE',  ( 20.05068032856350513, 11.88301801996953344, -1.993596777108510576 ) ) ;
#23054 = CARTESIAN_POINT ( 'NONE',  ( 1.124000490775577399, -33.02214389350386625, 7.724038915126860694 ) ) ;
#23055 = CARTESIAN_POINT ( 'NONE',  ( 81.31796987085604655, 61.39415816021645611, 1.370814772368732948 ) ) ;
#23056 = CARTESIAN_POINT ( 'NONE',  ( 88.90249899953845159, -1.697492344831515121, -0.8687328377452782080 ) ) ;
#23057 = CARTESIAN_POINT ( 'NONE',  ( -1.784597664094826008, -29.51857049915745890, 7.785344483711591934 ) ) ;
#23058 = ORIENTED_EDGE ( 'NONE', *, *, #7396, .T. ) ;
#23059 = DIRECTION ( 'NONE',  ( 0.6502177225477924205, -0.3754033771448251899, -0.6605219282605403475 ) ) ;
#23060 = CARTESIAN_POINT ( 'NONE',  ( 31.84879310987939149, -3.762318538055401618, 4.773639746032809938 ) ) ;
#23061 = CARTESIAN_POINT ( 'NONE',  ( 33.11561061937418060, -3.385635371879725408, -5.363104269438873750 ) ) ;
#23062 = CARTESIAN_POINT ( 'NONE',  ( 36.14138348061285200, -3.141491348386876936, -5.847134993448860563 ) ) ;
#23063 = FACE_OUTER_BOUND ( 'NONE', #23672, .T. ) ;
#23064 = CARTESIAN_POINT ( 'NONE',  ( 84.47471770354184173, 2.556968559651632944, -3.354246977694447462 ) ) ;
#23065 = DIRECTION ( 'NONE',  ( 0.000000000000000000, 0.000000000000000000, 1.000000000000000000 ) ) ;
#23066 = CARTESIAN_POINT ( 'NONE',  ( 7.121324086407810228, -24.55319635012989110, 6.800000000000000711 ) ) ;
#23067 = AXIS2_PLACEMENT_3D ( 'NONE', #6202, #12982, #31322 ) ;
#23068 = DIRECTION ( 'NONE',  ( 1.000000000000000000, 0.000000000000000000, 0.000000000000000000 ) ) ;
#23069 = CARTESIAN_POINT ( 'NONE',  ( 29.48897355024926270, -3.189277998897150912, 4.808865534657858376 ) ) ;
#23070 = ORIENTED_EDGE ( 'NONE', *, *, #11131, .F. ) ;
#23071 = B_SPLINE_CURVE_WITH_KNOTS ( 'NONE', 3,
 ( #7125, #6922, #31845, #13290, #22385, #9387, #37792, #32260, #22584, #154, #19076, #4060, #12895, #16575, #19279, #22182, #13099, #37590, #16187 ),
 .UNSPECIFIED., .F., .F.,
 ( 4, 3, 3, 3, 3, 3, 4 ),
 ( 1.226634733346699349E-18, 2.546128104244621453E-05, 5.711050680483870356E-05, 8.113074941675817360E-05, 0.0001053129305727074034, 0.0001360598016347105499, 0.0001612931755701972581 ),
 .UNSPECIFIED. ) ;
#23072 = VERTEX_POINT ( 'NONE', #21106 ) ;
#23073 = CARTESIAN_POINT ( 'NONE',  ( 36.44519052358557332, -1.732482462384099975, 5.730822330882753057 ) ) ;
#23074 = DIRECTION ( 'NONE',  ( -0.000000000000000000, -0.000000000000000000, -1.000000000000000000 ) ) ;
#23075 = CARTESIAN_POINT ( 'NONE',  ( 33.45304404609620263, -3.772033185430891500, 5.158132413726952414 ) ) ;
#23076 = CARTESIAN_POINT ( 'NONE',  ( 86.82478445301771330, -1.108591820897244062, 5.258890510423615439 ) ) ;
#23077 = EDGE_CURVE ( 'NONE', #14763, #32941, #10846, .T. ) ;
#23078 = ORIENTED_EDGE ( 'NONE', *, *, #40496, .T. ) ;
#23079 = CIRCLE ( 'NONE', #4052, 0.1000000000000028644 ) ;
#23080 = ADVANCED_FACE ( 'NONE', ( #38996 ), #7721, .F. ) ;
#23081 = CARTESIAN_POINT ( 'NONE',  ( -64.08758708074093136, 36.14363715547680300, -3.800414904976364028 ) ) ;
#23082 = ORIENTED_EDGE ( 'NONE', *, *, #9858, .F. ) ;
#23083 = CARTESIAN_POINT ( 'NONE',  ( -55.42153689335680156, 31.50958069423707641, -3.999999999999998224 ) ) ;
#23084 = CARTESIAN_POINT ( 'NONE',  ( 3.823044550204501402, -32.35280395774920237, 6.887547729233690852 ) ) ;
#23085 = ORIENTED_EDGE ( 'NONE', *, *, #21442, .F. ) ;
#23086 = CARTESIAN_POINT ( 'NONE',  ( 21.91074531573966766, 5.459064786471969022, 3.355207856022180302 ) ) ;
#23087 = CARTESIAN_POINT ( 'NONE',  ( 82.17153865661288137, 64.85009419791096263, -1.775718711110015224 ) ) ;
#23088 = DIRECTION ( 'NONE',  ( -0.8660254037844377084, 0.000000000000000000, 0.5000000000000015543 ) ) ;
#23089 = ORIENTED_EDGE ( 'NONE', *, *, #38389, .T. ) ;
#23090 = CARTESIAN_POINT ( 'NONE',  ( 75.52602547247359155, 59.92744485144773847, -3.494507759123859802 ) ) ;
#23092 = DIRECTION ( 'NONE',  ( 1.000000000000000000, 0.000000000000000000, 0.000000000000000000 ) ) ;
#23091 = CARTESIAN_POINT ( 'NONE',  ( 2.445140233331022372, -26.15008410077153300, 6.872971584836693459 ) ) ;
#23093 = CYLINDRICAL_SURFACE ( 'NONE', #17170, 6.000000000000002665 ) ;
#23094 = CARTESIAN_POINT ( 'NONE',  ( 76.36824339142353324, 62.58715529212010864, 3.801074476319127093 ) ) ;
#23095 = CARTESIAN_POINT ( 'NONE',  ( -1.666958026621576883, -30.04000107135736641, 7.754798119455333705 ) ) ;
#23096 = AXIS2_PLACEMENT_3D ( 'NONE', #4262, #2348, #33640 ) ;
#23097 = CARTESIAN_POINT ( 'NONE',  ( -25.39999999999996305, 0.000000000000000000, 0.000000000000000000 ) ) ;
#23098 = CARTESIAN_POINT ( 'NONE',  ( 24.20108879139602465, 2.667881056255625438, -3.983563230078315698 ) ) ;
#23099 = DIRECTION ( 'NONE',  ( -0.000000000000000000, -0.000000000000000000, -1.000000000000000000 ) ) ;
#23100 = CARTESIAN_POINT ( 'NONE',  ( 79.49585004866924010, 66.23094581382579804, 1.662695954554603617 ) ) ;
#23101 = CARTESIAN_POINT ( 'NONE',  ( 3.739317481034212243, -32.29073431218959911, 7.013842709614101167 ) ) ;
#23102 = CARTESIAN_POINT ( 'NONE',  ( 29.46612689758034875, 1.430465584783186639, -3.840811867917949929 ) ) ;
#23103 = CARTESIAN_POINT ( 'NONE',  ( 4.514135614585971013, -27.47691543170328643, 7.387053503561888057 ) ) ;
#23104 = CARTESIAN_POINT ( 'NONE',  ( -70.05493584469058987, -21.28726706566848748, 9.961909801952206323 ) ) ;
#23105 = CARTESIAN_POINT ( 'NONE',  ( 4.674695785371929979, -31.40593021786562744, 7.771081512783701406 ) ) ;
#23106 = CARTESIAN_POINT ( 'NONE',  ( 0.6657407460327561255, -26.33116491667136216, 6.865312560952602894 ) ) ;
#23107 = CARTESIAN_POINT ( 'NONE',  ( 68.91489483114931147, 58.10232893654896458, 3.936674041830252158 ) ) ;
#23108 = VECTOR ( 'NONE', #33765, 1000.000000000000000 ) ;
#23109 = CARTESIAN_POINT ( 'NONE',  ( 34.45378869156874657, -1.156911132109146312, -5.566333934908320735 ) ) ;
#23110 = CARTESIAN_POINT ( 'NONE',  ( 1.070632901679560378, -32.91111266939319080, 7.784838882742139532 ) ) ;
#23111 = CARTESIAN_POINT ( 'NONE',  ( 4.712346640638399364, -31.35267092476172479, 6.887161170156907097 ) ) ;
#23112 = CARTESIAN_POINT ( 'NONE',  ( 0.6225211420409756391, -26.24003551177748861, 7.750000000000000888 ) ) ;
#23113 = CARTESIAN_POINT ( 'NONE',  ( -1.546174839641468735, -28.26456800474412034, 7.761113333116787416 ) ) ;
#23114 = DIRECTION ( 'NONE',  ( -1.000000000000000000, 0.000000000000000000, 0.000000000000000000 ) ) ;
#23115 = CARTESIAN_POINT ( 'NONE',  ( -0.4578616284939905356, -32.19708638888766217, 7.680992449362111785 ) ) ;
#23116 = ORIENTED_EDGE ( 'NONE', *, *, #23514, .F. ) ;
#23117 = CARTESIAN_POINT ( 'NONE',  ( 27.58409624374816360, 1.448159382144707186, 4.473608046789665060 ) ) ;
#23118 = CARTESIAN_POINT ( 'NONE',  ( 67.66997365410338716, 58.45410198214950981, -3.990378031984448182 ) ) ;
#23119 = B_SPLINE_CURVE_WITH_KNOTS ( 'NONE', 3,
 ( #2721, #27117, #5500, #17420 ),
 .UNSPECIFIED., .F., .F.,
 ( 4, 4 ),
 ( 0.0008960438496711642777, 0.001150058339056989976 ),
 .UNSPECIFIED. ) ;
#23120 = CARTESIAN_POINT ( 'NONE',  ( 4.722665460610376620, -27.80475174052855536, 7.640616322432100205 ) ) ;
#23121 = VERTEX_POINT ( 'NONE', #20271 ) ;
#23122 = FACE_OUTER_BOUND ( 'NONE', #12656, .T. ) ;
#23124 = ADVANCED_FACE ( 'NONE', ( #5045 ), #16128, .T. ) ;
#23123 = CARTESIAN_POINT ( 'NONE',  ( -70.92837670882107659, 3.729367930467589076, 0.000000000000000000 ) ) ;
#23125 = CARTESIAN_POINT ( 'NONE',  ( 85.38650254764779390, 1.316965040104128626, -5.564122293564899735 ) ) ;
#23126 = CARTESIAN_POINT ( 'NONE',  ( -61.00670947824507806, 24.84364830758654108, -8.800414904976364028 ) ) ;
#23127 = CARTESIAN_POINT ( 'NONE',  ( 0.4012375803829261178, -32.81988445204935800, 6.864673517077424236 ) ) ;
#23128 = CYLINDRICAL_SURFACE ( 'NONE', #22566, 0.1000000000000028644 ) ;
#23129 = EDGE_LOOP ( 'NONE', ( #5330, #6481, #38895, #34720 ) ) ;
#23130 = CARTESIAN_POINT ( 'NONE',  ( 23.43505160883933058, 3.791633034196467467, 3.107909060890779340 ) ) ;
#23131 = CYLINDRICAL_SURFACE ( 'NONE', #26100, 1.500000000000001332 ) ;
#23132 = CARTESIAN_POINT ( 'NONE',  ( 78.87101214850905251, 66.02979514927503146, 1.817988788077138596 ) ) ;
#23133 = AXIS2_PLACEMENT_3D ( 'NONE', #2285, #8634, #15226 ) ;
#23134 = CARTESIAN_POINT ( 'NONE',  ( -63.54361195871889834, 43.49475130726206373, 3.057987111335950026 ) ) ;
#23135 = ORIENTED_EDGE ( 'NONE', *, *, #23966, .F. ) ;
#23136 = CARTESIAN_POINT ( 'NONE',  ( 79.79883522896109582, 62.08831372790998415, -3.424416364708440685 ) ) ;
#23138 = CARTESIAN_POINT ( 'NONE',  ( -1.707939823346567021, -28.77413670247031519, 6.966757512882405301 ) ) ;
#23137 = CARTESIAN_POINT ( 'NONE',  ( 22.61475275727087464, 0.2954930242483900238, 6.495504608876625952 ) ) ;
#23139 = CARTESIAN_POINT ( 'NONE',  ( 81.56578493135152996, 62.15373153752272373, -2.499697124808072157 ) ) ;
#23140 = CARTESIAN_POINT ( 'NONE',  ( 80.15150095960399312, 61.72183351646653904, 3.055712048904937195 ) ) ;
#23141 = ORIENTED_EDGE ( 'NONE', *, *, #31294, .T. ) ;
#23142 = CARTESIAN_POINT ( 'NONE',  ( -26.87867591359219333, -26.64985754041175525, 6.700000000000000178 ) ) ;
#23143 = CARTESIAN_POINT ( 'NONE',  ( 82.49284700683531923, 64.23424719397920057, 1.468380750527791268 ) ) ;
#23144 = DIRECTION ( 'NONE',  ( -0.000000000000000000, -1.000000000000000000, -0.000000000000000000 ) ) ;
#23145 = CARTESIAN_POINT ( 'NONE',  ( 24.25791012409692371, 0.7154099962172090210, -6.776768987914707942 ) ) ;
#23146 = EDGE_CURVE ( 'NONE', #9291, #34893, #30158, .T. ) ;
#23147 = CYLINDRICAL_SURFACE ( 'NONE', #33828, 0.9999999999999998890 ) ;
#23148 = ORIENTED_EDGE ( 'NONE', *, *, #37881, .F. ) ;
#23149 = CARTESIAN_POINT ( 'NONE',  ( -77.42388607530644151, -4.859301208013656392, 9.188011873594817303 ) ) ;
#23150 = CYLINDRICAL_SURFACE ( 'NONE', #35793, 9.386006772603931125 ) ;
#23151 = CARTESIAN_POINT ( 'NONE',  ( -1.035018467416049415, -31.74189774292361577, 7.776484688137389689 ) ) ;
#23152 = ORIENTED_EDGE ( 'NONE', *, *, #35047, .T. ) ;
#23153 = CARTESIAN_POINT ( 'NONE',  ( 35.83227016345950489, -3.728989527342261301, -5.623816504269203875 ) ) ;
#23154 = DIRECTION ( 'NONE',  ( -0.000000000000000000, -0.000000000000000000, -1.000000000000000000 ) ) ;
#23155 = CARTESIAN_POINT ( 'NONE',  ( 3.301369968908216990, -32.68230282137928810, 6.895394898881662016 ) ) ;
#23156 = CARTESIAN_POINT ( 'NONE',  ( -1.090829593295360223, -31.68159764409877255, 6.903112506833894102 ) ) ;
#23157 = CARTESIAN_POINT ( 'NONE',  ( 5.196611068567014158, -29.73267931344627613, 6.887547729233683746 ) ) ;
#23158 = CARTESIAN_POINT ( 'NONE',  ( -0.5641756119095632238, -26.90127093817460135, 7.643192810543826710 ) ) ;
#23159 = EDGE_CURVE ( 'NONE', #29402, #39054, #29746, .T. ) ;
#23160 = FACE_OUTER_BOUND ( 'NONE', #39171, .T. ) ;
#23161 = EDGE_CURVE ( 'NONE', #29464, #9354, #11430, .T. ) ;
#23162 = CARTESIAN_POINT ( 'NONE',  ( -71.72837670882105954, -34.30579396504363388, 1.385640646055090519 ) ) ;
#23163 = LINE ( 'NONE', #17711, #22322 ) ;
#23164 = ORIENTED_EDGE ( 'NONE', *, *, #23953, .F. ) ;
#23165 = VERTEX_POINT ( 'NONE', #14696 ) ;
#23166 = CARTESIAN_POINT ( 'NONE',  ( 66.88492799900151908, 57.87961537897388808, 3.998747512900713730 ) ) ;
#23167 = CIRCLE ( 'NONE', #32379, 5.950000000000010836 ) ;
#23168 = CARTESIAN_POINT ( 'NONE',  ( 21.78047233922835346, 5.616103166486084319, -3.473245622192032034 ) ) ;
#23169 = CARTESIAN_POINT ( 'NONE',  ( 84.44530234979703209, 2.765803402995568927, 2.732740112990733383 ) ) ;
#23170 = ADVANCED_FACE ( 'NONE', ( #33050 ), #9151, .F. ) ;
#23171 = ORIENTED_EDGE ( 'NONE', *, *, #8536, .T. ) ;
#23172 = CARTESIAN_POINT ( 'NONE',  ( 2.863657326339113851, -26.26889862419239918, 7.698786668945012401 ) ) ;
#23173 = SHAPE_DEFINITION_REPRESENTATION ( #30987, #24012 ) ;
#23174 = DIRECTION ( 'NONE',  ( -0.000000000000000000, -0.000000000000000000, 1.000000000000000000 ) ) ;
#23175 = CARTESIAN_POINT ( 'NONE',  ( -2.673316637388258865, -27.10729750018004935, 7.695279973900954751 ) ) ;
#23176 = ORIENTED_EDGE ( 'NONE', *, *, #1328, .F. ) ;
#23177 = ORIENTED_EDGE ( 'NONE', *, *, #4047, .T. ) ;
#23178 = CARTESIAN_POINT ( 'NONE',  ( 79.16440527908333991, 64.96746831917748466, -3.289664858626429211 ) ) ;
#23179 = CARTESIAN_POINT ( 'NONE',  ( 33.68904022949467958, -4.468562645166327840, 4.246708699803020792 ) ) ;
#23180 = CARTESIAN_POINT ( 'NONE',  ( 79.23217405491450904, 65.02354781853230747, 3.268578535636609494 ) ) ;
#23182 = ORIENTED_EDGE ( 'NONE', *, *, #4826, .T. ) ;
#23181 = FACE_OUTER_BOUND ( 'NONE', #29851, .T. ) ;
#23183 = EDGE_CURVE ( 'NONE', #30629, #16055, #40584, .T. ) ;
#23184 = EDGE_CURVE ( 'NONE', #19049, #9920, #27374, .T. ) ;
#23185 = DIRECTION ( 'NONE',  ( 0.000000000000000000, 0.000000000000000000, 1.000000000000000000 ) ) ;
#23186 = CARTESIAN_POINT ( 'NONE',  ( 4.042889426911806972, -27.10564586790783892, 6.949473656533219135 ) ) ;
#23187 = CARTESIAN_POINT ( 'NONE',  ( 1.021324086407808585, -24.55319635012989110, 6.800000000000000711 ) ) ;
#23188 = CARTESIAN_POINT ( 'NONE',  ( 33.75963076984755418, -4.729058622324783023, -3.755006780454513304 ) ) ;
#23189 = CARTESIAN_POINT ( 'NONE',  ( 3.384110555093582384, -26.61610462891116313, 7.748216051605124832 ) ) ;
#23190 = CARTESIAN_POINT ( 'NONE',  ( 77.23450810825278268, 65.03073311407490564, -2.276535451367163621 ) ) ;
#23191 = AXIS2_PLACEMENT_3D ( 'NONE', #29550, #23174, #32257 ) ;
#23192 = CARTESIAN_POINT ( 'NONE',  ( 14.71633116765073623, -5.064965072526596224, -2.500000000000000888 ) ) ;
#23193 = CARTESIAN_POINT ( 'NONE',  ( -0.5399441734843601903, -32.25896884755352545, 7.756742906098588186 ) ) ;
#23194 = CARTESIAN_POINT ( 'NONE',  ( -75.36736324129955733, -5.074094651746722917, -8.962379545620084542 ) ) ;
#23195 = CARTESIAN_POINT ( 'NONE',  ( -0.01704589846277644594, -26.63557199280749899, 7.643333865083955736 ) ) ;
#23196 = CARTESIAN_POINT ( 'NONE',  ( -13.07867591359219617, -26.64985754041175525, 6.700000000000000178 ) ) ;
#23197 = CARTESIAN_POINT ( 'NONE',  ( 80.91044703854151976, 63.42644682079063045, 3.500437194783534434 ) ) ;
#23198 = CARTESIAN_POINT ( 'NONE',  ( -4.220127061295482087E-17, 0.7293679304675931840, 6.000000000000000000 ) ) ;
#23199 =( BOUNDED_CURVE ( )  B_SPLINE_CURVE ( 3, ( #28703, #32010, #9761, #13049 ),
 .UNSPECIFIED., .F., .F. ) 
 B_SPLINE_CURVE_WITH_KNOTS ( ( 4, 4 ),
 ( 1.347909859412852907, 1.534781240595298080 ),
 .UNSPECIFIED. ) 
 CURVE ( )  GEOMETRIC_REPRESENTATION_ITEM ( )  RATIONAL_B_SPLINE_CURVE ( ( 1.000000000000000000, 0.9970920404276226723, 0.9970920404276226723, 1.000000000000000000 ) ) 
 REPRESENTATION_ITEM ( '' )  );
#23200 = CARTESIAN_POINT ( 'NONE',  ( -1.284247711295874561, -27.76865114928376599, 7.784725160561910329 ) ) ;
#23201 = CARTESIAN_POINT ( 'NONE',  ( 2.388817387744127441, -25.35382237095210201, 7.695279973900954751 ) ) ;
#23202 = CARTESIAN_POINT ( 'NONE',  ( 33.70353959993166626, -1.254899476156281946, 5.466650496391561198 ) ) ;
#23203 = EDGE_CURVE ( 'NONE', #1317, #218, #40647, .T. ) ;
#23204 = EDGE_CURVE ( 'NONE', #10597, #13756, #10672, .T. ) ;
#23205 = EDGE_CURVE ( 'NONE', #2658, #40515, #30945, .T. ) ;
#23206 = CARTESIAN_POINT ( 'NONE',  ( 4.488362440207297688, -27.45398732327946334, 7.011627023500181188 ) ) ;
#23207 = DIRECTION ( 'NONE',  ( 1.000000000000000000, 0.000000000000000000, 0.000000000000000000 ) ) ;
#23208 = CARTESIAN_POINT ( 'NONE',  ( 4.890934407267558903, -28.39499951105307574, 7.756377446753164762 ) ) ;
#23209 = DIRECTION ( 'NONE',  ( -0.000000000000000000, -1.000000000000000000, -0.000000000000000000 ) ) ;
#23210 = LINE ( 'NONE', #29583, #30050 ) ;
#23211 = EDGE_LOOP ( 'NONE', ( #37148, #27531, #3952, #24105 ) ) ;
#23212 = CARTESIAN_POINT ( 'NONE',  ( 68.47014483779531702, 58.97518246833449496, 3.964410623303925796 ) ) ;
#23213 = CARTESIAN_POINT ( 'NONE',  ( 36.99281227302647324, -2.718855070858015033, 5.980021048388253213 ) ) ;
#23214 = VECTOR ( 'NONE', #11611, 1000.000000000000000 ) ;
#23215 = DIRECTION ( 'NONE',  ( -0.000000000000000000, -0.000000000000000000, 1.000000000000000000 ) ) ;
#23216 = CARTESIAN_POINT ( 'NONE',  ( 86.87490948991990081, 0.7757029256828257280, 5.355124474773749199 ) ) ;
#23218 = CARTESIAN_POINT ( 'NONE',  ( -2.742979246814043925, -31.14891988278930413, 7.695279973900954751 ) ) ;
#23217 = CARTESIAN_POINT ( 'NONE',  ( 79.24015747652954644, 65.65980919716059816, -2.710038060602469656 ) ) ;
#23219 = CARTESIAN_POINT ( 'NONE',  ( -1.232229479062399102, -27.65950027256457844, 6.980586498568968068 ) ) ;
#23220 = VECTOR ( 'NONE', #26337, 1000.000000000000000 ) ;
#23221 = CARTESIAN_POINT ( 'NONE',  ( -58.44033895488189501, 28.22358054771055436, 5.330345403092622725 ) ) ;
#23222 = ORIENTED_EDGE ( 'NONE', *, *, #21156, .F. ) ;
#23223 = CARTESIAN_POINT ( 'NONE',  ( -79.13014441944265798, 11.46068214799393736, -5.736672290455380185 ) ) ;
#23224 = DIRECTION ( 'NONE',  ( 1.241493069327139093E-16, -1.000000000000000000, 0.000000000000000000 ) ) ;
#23225 = EDGE_LOOP ( 'NONE', ( #27612, #13388, #60, #28375 ) ) ;
#23226 = CARTESIAN_POINT ( 'NONE',  ( 3.657089259928787417, -24.90412260081853546, 6.894806418505347700 ) ) ;
#23227 = ORIENTED_EDGE ( 'NONE', *, *, #40215, .T. ) ;
#23228 = ORIENTED_EDGE ( 'NONE', *, *, #37217, .T. ) ;
#23229 = CARTESIAN_POINT ( 'NONE',  ( 80.25680044982675554, 63.48435701671603937, -3.692178340560190009 ) ) ;
#23230 = LINE ( 'NONE', #4305, #36514 ) ;
#23231 = CARTESIAN_POINT ( 'NONE',  ( 80.53350286136132752, 63.24990014040474051, 3.607546830629784207 ) ) ;
#23232 = CARTESIAN_POINT ( 'NONE',  ( 25.12776268638631549, 1.000125724568426078, 4.612937808490496394 ) ) ;
#23233 = VERTEX_POINT ( 'NONE', #37300 ) ;
#23234 = VECTOR ( 'NONE', #20454, 1000.000000000000000 ) ;
#23235 = CARTESIAN_POINT ( 'NONE',  ( -0.09836077524968195318, -32.45515033324894461, 7.761597726988851420 ) ) ;
#23237 = CARTESIAN_POINT ( 'NONE',  ( 3.976673778722537023, -32.22860238476790329, 7.678495282201407868 ) ) ;
#23236 = CARTESIAN_POINT ( 'NONE',  ( 37.83867290611771494, -6.084034091406928191, -6.000000000000000000 ) ) ;
#23238 = CARTESIAN_POINT ( 'NONE',  ( -16.87867591359218977, -26.64985754041175525, 6.800000000000000711 ) ) ;
#23239 = CARTESIAN_POINT ( 'NONE',  ( -64.08758708074093136, 43.59023631735133364, -1.301703137985040781 ) ) ;
#23240 = DIRECTION ( 'NONE',  ( 0.000000000000000000, 0.000000000000000000, 1.000000000000000000 ) ) ;
#23241 = CARTESIAN_POINT ( 'NONE',  ( 23.65147222854444919, 3.378127406782373665, -3.542646716268693208 ) ) ;
#23242 = EDGE_LOOP ( 'NONE', ( #1237, #450, #28272, #30492 ) ) ;
#23243 = CARTESIAN_POINT ( 'NONE',  ( 5.150202707224498688, -30.16051711886163744, 7.750000000000001776 ) ) ;
#23244 = ADVANCED_FACE ( 'NONE', ( #34249 ), #18556, .F. ) ;
#23245 = VECTOR ( 'NONE', #8307, 1000.000000000000000 ) ;
#23246 = CARTESIAN_POINT ( 'NONE',  ( 22.79131883835711037, -5.922936844141047708, 5.170149038749508819 ) ) ;
#23247 = EDGE_CURVE ( 'NONE', #29003, #7610, #14095, .T. ) ;
#23248 = CARTESIAN_POINT ( 'NONE',  ( 21.80570325383046182, 6.356989464231188158, 3.898355529982616918 ) ) ;
#23249 = CARTESIAN_POINT ( 'NONE',  ( 13.80252870930811326, 11.14042161257683006, 2.500000000000004885 ) ) ;
#23250 = CARTESIAN_POINT ( 'NONE',  ( 0.4209974261821289865, -32.72005136235081579, 6.863904403958575706 ) ) ;
#23251 = CARTESIAN_POINT ( 'NONE',  ( 78.84958593098259882, 66.12877247161574701, 1.370814772368738055 ) ) ;
#23252 = CARTESIAN_POINT ( 'NONE',  ( 87.57592060778061693, -0.6244806207018304134, 5.359096402341661403 ) ) ;
#23253 = CARTESIAN_POINT ( 'NONE',  ( -8.248748702180632719, -26.64985754041175525, 6.800000000000000711 ) ) ;
#23254 = ORIENTED_EDGE ( 'NONE', *, *, #25814, .T. ) ;
#23255 = EDGE_CURVE ( 'NONE', #7785, #28942, #38166, .T. ) ;
#23256 = CARTESIAN_POINT ( 'NONE',  ( -77.80754174939649204, -5.030728402074980288, 8.890429129847960965 ) ) ;
#23257 = DIRECTION ( 'NONE',  ( 0.000000000000000000, 0.000000000000000000, 1.000000000000000000 ) ) ;
#23258 = CARTESIAN_POINT ( 'NONE',  ( 32.23520098731326300, -3.776787765129337782, 4.847381814357383689 ) ) ;
#23259 = CARTESIAN_POINT ( 'NONE',  ( 28.89658576139254720, -2.947360769642642708, -4.716409093270361730 ) ) ;
#23260 = CARTESIAN_POINT ( 'NONE',  ( 32.77973188623823120, -0.9315922670084764157, -5.322467960295677258 ) ) ;
#23261 = CARTESIAN_POINT ( 'NONE',  ( -70.92837670882107659, 28.72470171467712063, 0.000000000000000000 ) ) ;
#23262 = CARTESIAN_POINT ( 'NONE',  ( -16.24874870218063450, -25.49307895267003587, 6.700000000000000178 ) ) ;
#23263 = FACE_OUTER_BOUND ( 'NONE', #11721, .T. ) ;
#23264 = ORIENTED_EDGE ( 'NONE', *, *, #36534, .F. ) ;
#23265 = DIRECTION ( 'NONE',  ( 0.000000000000000000, 1.147978770867004622E-16, -1.000000000000000000 ) ) ;
#23266 = CARTESIAN_POINT ( 'NONE',  ( -0.9786759135921931918, -26.64985754041175525, 6.700000000000000178 ) ) ;
#23267 = AXIS2_PLACEMENT_3D ( 'NONE', #15519, #21709, #40628 ) ;
#23268 = CARTESIAN_POINT ( 'NONE',  ( 4.988271557043087334, -28.40293458425108142, 7.781480525794716385 ) ) ;
#23269 = VERTEX_POINT ( 'NONE', #13814 ) ;
#23270 = ORIENTED_EDGE ( 'NONE', *, *, #13429, .T. ) ;
#23271 = CARTESIAN_POINT ( 'NONE',  ( 35.36826174472263062, -3.792953908414599340, 5.510393643995938895 ) ) ;
#23272 = CARTESIAN_POINT ( 'NONE',  ( 4.536655203520439272, -25.19670069055390016, 6.894806418505347700 ) ) ;
#23273 = CARTESIAN_POINT ( 'NONE',  ( 66.27376694609004915, 57.73522568913436004, -4.000000000000000000 ) ) ;
#23274 = VECTOR ( 'NONE', #15463, 1000.000000000000000 ) ;
#23275 = ORIENTED_EDGE ( 'NONE', *, *, #18970, .F. ) ;
#23276 = EDGE_LOOP ( 'NONE', ( #16435, #10244, #36052, #39832, #5906 ) ) ;
#23277 = CARTESIAN_POINT ( 'NONE',  ( -64.08758708074094557, 37.77509509994405335, -3.093168342233789225 ) ) ;
#23278 = DIRECTION ( 'NONE',  ( -0.9396926207859057634, -0.3420201433256757073, -0.000000000000000000 ) ) ;
#23279 = ORIENTED_EDGE ( 'NONE', *, *, #1739, .F. ) ;
#23280 = CARTESIAN_POINT ( 'NONE',  ( 21.75869166788903186, 5.877497079131895674, 3.362859741260915580 ) ) ;
#23281 = CARTESIAN_POINT ( 'NONE',  ( 81.27149311957269617, 65.88890312491017198, -1.680016503630878066 ) ) ;
#23282 = CARTESIAN_POINT ( 'NONE',  ( 6.921324086407803833, -26.64985754041175525, 6.700000000000000178 ) ) ;
#23283 = ORIENTED_EDGE ( 'NONE', *, *, #36793, .T. ) ;
#23285 = CARTESIAN_POINT ( 'NONE',  ( -32.44874870218063734, -26.64985754041175525, 6.700000000000000178 ) ) ;
#23284 = CARTESIAN_POINT ( 'NONE',  ( 2.495056794208367013, -26.16133723403751432, 6.935328752148349096 ) ) ;
#23286 = CARTESIAN_POINT ( 'NONE',  ( 0.2000000000000000111, 0.000000000000000000, 0.000000000000000000 ) ) ;
#23287 = CARTESIAN_POINT ( 'NONE',  ( 74.78802096516436393, 63.01683072882818948, 3.322260703561484618 ) ) ;
#23288 = CARTESIAN_POINT ( 'NONE',  ( 23.68961767579556010, 2.539811605600059252, -4.211040149488679774 ) ) ;
#23289 = CARTESIAN_POINT ( 'NONE',  ( -8.348748702180635917, -25.49307895267003587, 6.700000000000000178 ) ) ;
#23290 = CARTESIAN_POINT ( 'NONE',  ( 2.338742698598176073, -33.27093018339341057, 6.894806418505347700 ) ) ;
#23291 = VECTOR ( 'NONE', #39725, 1000.000000000000000 ) ;
#23292 = CARTESIAN_POINT ( 'NONE',  ( 27.39974682155295582, 1.067777558387527748, -4.482791175521097848 ) ) ;
#23293 = DIRECTION ( 'NONE',  ( 1.000000000000000000, 0.000000000000000000, 0.000000000000000000 ) ) ;
#23294 = DIRECTION ( 'NONE',  ( 1.000000000000000000, 0.000000000000000000, 0.000000000000000000 ) ) ;
#23295 = CARTESIAN_POINT ( 'NONE',  ( 78.68916368339945677, 66.05772639262711721, 1.037317649801914321 ) ) ;
#23296 = CARTESIAN_POINT ( 'NONE',  ( -0.2081541720287059805, -32.50377728021632606, 6.921725064902957136 ) ) ;
#23297 = CARTESIAN_POINT ( 'NONE',  ( 29.21535032918476915, 2.216127810226045547, -1.021449648108430086 ) ) ;
#23298 = CARTESIAN_POINT ( 'NONE',  ( -1.699583094839331787, -29.58343279012807159, 7.635761828346577573 ) ) ;
#23299 = CYLINDRICAL_SURFACE ( 'NONE', #20247, 8.080217238368755162 ) ;
#23300 = EDGE_CURVE ( 'NONE', #26757, #28218, #8789, .T. ) ;
#23301 = EDGE_CURVE ( 'NONE', #4851, #30829, #33441, .T. ) ;
#23302 = VECTOR ( 'NONE', #27652, 1000.000000000000000 ) ;
#23303 = CYLINDRICAL_SURFACE ( 'NONE', #37305, 0.09010775117052866046 ) ;
#23304 = FACE_OUTER_BOUND ( 'NONE', #21669, .T. ) ;
#23305 = DIRECTION ( 'NONE',  ( 1.000000000000000000, -0.000000000000000000, 0.000000000000000000 ) ) ;
#23306 = EDGE_CURVE ( 'NONE', #15332, #30342, #32768, .T. ) ;
#23307 = CARTESIAN_POINT ( 'NONE',  ( 36.99142113593869396, -2.973170736671415071, -5.979803927800903196 ) ) ;
#23308 = CARTESIAN_POINT ( 'NONE',  ( -38.97867591359219119, -26.64985754041175525, 6.800000000000000711 ) ) ;
#23309 = CARTESIAN_POINT ( 'NONE',  ( -1.699609906766908818, -29.56993018339339940, 7.620413589471895399 ) ) ;
#23310 = CARTESIAN_POINT ( 'NONE',  ( -1.799560655197548487, -29.58853437876398118, 7.748475685504735644 ) ) ;
#23311 = CARTESIAN_POINT ( 'NONE',  ( -15.07867591359219439, -24.55319635012989110, 6.700000000000000178 ) ) ;
#23312 = LINE ( 'NONE', #1699, #34934 ) ;
#23313 = ORIENTED_EDGE ( 'NONE', *, *, #32984, .T. ) ;
#23314 = CARTESIAN_POINT ( 'NONE',  ( 36.88183944235395728, -2.428786062484896480, 5.959470125505070826 ) ) ;
#23315 = CARTESIAN_POINT ( 'NONE',  ( -69.98383490720681266, -0.4546002296310912572, 3.925186983125784401 ) ) ;
#23316 = CARTESIAN_POINT ( 'NONE',  ( 67.51064039993573829, 57.98508837280776618, -3.992553130659727945 ) ) ;
#23317 = B_SPLINE_CURVE_WITH_KNOTS ( 'NONE', 3,
 ( #19465, #22770, #32243, #16558, #40664, #12466, #25037, #37571, #3446, #15962 ),
 .UNSPECIFIED., .F., .F.,
 ( 4, 3, 3, 4 ),
 ( 0.0001585009270395762383, 0.0001815657551981843026, 0.0002118214035944171133, 0.0002170292169044785754 ),
 .UNSPECIFIED. ) ;
#23318 = CARTESIAN_POINT ( 'NONE',  ( -1.347936336206764008, -27.85013040703412912, 7.678495282201406091 ) ) ;
#23319 = VECTOR ( 'NONE', #19812, 1000.000000000000000 ) ;
#23320 = VERTEX_POINT ( 'NONE', #38310 ) ;
#23321 = FACE_OUTER_BOUND ( 'NONE', #6438, .T. ) ;
#23322 = CARTESIAN_POINT ( 'NONE',  ( 86.03314645334975808, 0.1914443106846198395, -5.998834454465889365 ) ) ;
#23323 = CARTESIAN_POINT ( 'NONE',  ( 85.03548763332921112, 1.825262285978656251, -4.977705953854337118 ) ) ;
#23324 = CARTESIAN_POINT ( 'NONE',  ( 5.044480966521144971, -28.53694452721211050, 7.009310105710484073 ) ) ;
#23325 = DIRECTION ( 'NONE',  ( -0.3420201433256601087, -0.9396926207859114255, -0.000000000000000000 ) ) ;
#23326 = DIRECTION ( 'NONE',  ( -0.8888117386314211554, -0.4582725098355677762, 0.000000000000000000 ) ) ;
#23327 = EDGE_LOOP ( 'NONE', ( #36668, #8725, #12283, #3922, #12653 ) ) ;
#23328 = CARTESIAN_POINT ( 'NONE',  ( 21.83311778635127709, 5.946302252710771619, 3.143334175583627932 ) ) ;
#23329 = VECTOR ( 'NONE', #39925, 1000.000000000000000 ) ;
#23330 = CARTESIAN_POINT ( 'NONE',  ( 81.20006484400859392, 61.61449114502521240, 2.147349935851011526 ) ) ;
#23331 = CYLINDRICAL_SURFACE ( 'NONE', #37700, 0.1000000000000028644 ) ;
#23332 = VERTEX_POINT ( 'NONE', #16291 ) ;
#23333 = CARTESIAN_POINT ( 'NONE',  ( 79.89463791284350691, 61.88150425735624083, -3.258123098320698130 ) ) ;
#23335 = CARTESIAN_POINT ( 'NONE',  ( -70.92837670882107659, 13.87661300689593880, -3.784187430299790211 ) ) ;
#23334 = CARTESIAN_POINT ( 'NONE',  ( 21.78513789440741277, 0.2163316297486854445, 8.389159167568045916 ) ) ;
#23336 = CARTESIAN_POINT ( 'NONE',  ( 79.46506916755670602, 66.04886526173737593, -2.198649373785575456 ) ) ;
#23337 = CARTESIAN_POINT ( 'NONE',  ( 80.12095330986325337, 62.19218463582610212, 3.375657603866087264 ) ) ;
#23338 = VERTEX_POINT ( 'NONE', #28861 ) ;
#23339 = CARTESIAN_POINT ( 'NONE',  ( -17.69482985384421880, -42.37473357531882101, -6.000000000000000000 ) ) ;
#23340 = CARTESIAN_POINT ( 'NONE',  ( 81.01700449632699019, 66.08979032036411638, 1.386429027373558664 ) ) ;
#23341 = DIRECTION ( 'NONE',  ( -0.000000000000000000, -0.000000000000000000, 1.000000000000000000 ) ) ;
#23342 = CARTESIAN_POINT ( 'NONE',  ( 29.08816165369256268, -2.077165169587669613, 5.788842218736271583 ) ) ;
#23343 = CARTESIAN_POINT ( 'NONE',  ( 5.046365345827218185, -28.96623356337001809, 7.635761828346577573 ) ) ;
#23344 = VERTEX_POINT ( 'NONE', #668 ) ;
#23345 = CARTESIAN_POINT ( 'NONE',  ( -73.52991696981251835, -0.8431142006776708442, 10.87125227208380984 ) ) ;
#23346 = CARTESIAN_POINT ( 'NONE',  ( 21.73433939381562752, 0.2312908497712835021, -9.065555101204189725 ) ) ;
#23347 = CARTESIAN_POINT ( 'NONE',  ( -0.8688903936063803179, -27.19321022093548734, 7.013842709614101167 ) ) ;
#23348 = CIRCLE ( 'NONE', #1669, 6.000000000000002665 ) ;
#23349 = VECTOR ( 'NONE', #28364, 1000.000000000000000 ) ;
#23350 = LINE ( 'NONE', #22959, #38739 ) ;
#23351 = EDGE_CURVE ( 'NONE', #9750, #17194, #13205, .T. ) ;
#23352 = ORIENTED_EDGE ( 'NONE', *, *, #16462, .F. ) ;
#23353 = CARTESIAN_POINT ( 'NONE',  ( 21.73836974088880325, 4.234938348740031167, -2.803927442718175289 ) ) ;
#23354 =( LENGTH_UNIT ( ) NAMED_UNIT ( * ) SI_UNIT ( .MILLI., .METRE. ) );
#23355 = VECTOR ( 'NONE', #89, 1000.000000000000000 ) ;
#23356 = DIRECTION ( 'NONE',  ( 0.000000000000000000, 0.000000000000000000, -1.000000000000000000 ) ) ;
#23357 = CARTESIAN_POINT ( 'NONE',  ( 5.113695884919195578, -30.34410301451193703, 6.895394898881665569 ) ) ;
#23358 = CARTESIAN_POINT ( 'NONE',  ( -28.34874870218063947, -26.64985754041175525, 6.800000000000000711 ) ) ;
#23359 = CARTESIAN_POINT ( 'NONE',  ( 2.802452400329403126, -32.78637555231541256, 6.880147297696982633 ) ) ;
#23360 = CARTESIAN_POINT ( 'NONE',  ( -24.34874870218063592, -26.64985754041175525, 6.700000000000000178 ) ) ;
#23361 = AXIS2_PLACEMENT_3D ( 'NONE', #17784, #5245, #26667 ) ;
#23362 = CARTESIAN_POINT ( 'NONE',  ( 21.58862418887968460, 7.202556094215188054, 2.923978954502209682 ) ) ;
#23363 = ORIENTED_EDGE ( 'NONE', *, *, #40112, .F. ) ;
#23364 = CARTESIAN_POINT ( 'NONE',  ( 66.42198539279090141, 57.79096248115626366, 4.000000000000014211 ) ) ;
#23365 = CARTESIAN_POINT ( 'NONE',  ( 73.33417617461327609, 60.23131181272744072, -3.934110468510652492 ) ) ;
#23366 = CARTESIAN_POINT ( 'NONE',  ( 85.38915795161820199, 1.318023545160245558, -5.584599991349963766 ) ) ;
#23367 = CARTESIAN_POINT ( 'NONE',  ( -0.8725572984338751947, -27.34733221711291051, 6.894806418505345036 ) ) ;
#23368 = CYLINDRICAL_SURFACE ( 'NONE', #17528, 6.172764123155108251 ) ;
#23369 = EDGE_CURVE ( 'NONE', #2698, #10291, #33807, .T. ) ;
#23370 = CARTESIAN_POINT ( 'NONE',  ( -80.92837670882107659, 2.429809908902895277, 18.79999999999999716 ) ) ;
#23371 = CARTESIAN_POINT ( 'NONE',  ( 2.940588421764992688, -26.31267895086665831, 7.785344483711591934 ) ) ;
#23372 = CARTESIAN_POINT ( 'NONE',  ( 23.06594672544511582, -8.086844732617873177, 2.500000000000001332 ) ) ;
#23373 = CARTESIAN_POINT ( 'NONE',  ( 5.054699967764599400, -30.12545289942340077, 7.680992449362116226 ) ) ;
#23374 = AXIS2_PLACEMENT_3D ( 'NONE', #3494, #6761, #16807 ) ;
#23375 = AXIS2_PLACEMENT_3D ( 'NONE', #21152, #39663, #14539 ) ;
#23376 = ORIENTED_EDGE ( 'NONE', *, *, #33482, .T. ) ;
#23377 = CARTESIAN_POINT ( 'NONE',  ( 80.84620594802093763, 61.52815374075456845, -2.368006059521087447 ) ) ;
#23378 = CARTESIAN_POINT ( 'NONE',  ( 33.71578150949435582, -4.562017431774315845, 4.082147076938466235 ) ) ;
#23379 = CARTESIAN_POINT ( 'NONE',  ( 79.67348887277971414, 64.26584687736657031, 3.653685850874071939 ) ) ;
#23380 = PLANE ( 'NONE',  #7886 ) ;
#23381 = VECTOR ( 'NONE', #13727, 1000.000000000000000 ) ;
#23382 = EDGE_CURVE ( 'NONE', #8526, #11044, #3970, .T. ) ;
#23383 = PLANE ( 'NONE',  #22580 ) ;
#23384 = CARTESIAN_POINT ( 'NONE',  ( 3.922988059513587089, -26.99698279172644177, 6.894806418505345924 ) ) ;
#23385 = DIRECTION ( 'NONE',  ( 0.4690749385695426321, 0.8831583674551126695, 2.183007799372904676E-14 ) ) ;
#23386 = B_SPLINE_CURVE_WITH_KNOTS ( 'NONE', 3,
 ( #15835, #22637, #34599, #34803, #32117, #19331, #9859, #28808, #6167, #12948 ),
 .UNSPECIFIED., .F., .F.,
 ( 4, 3, 3, 4 ),
 ( 0.0005050348086185349949, 0.0005143352185143347608, 0.0005445898203825249879, 0.0005634294782181770286 ),
 .UNSPECIFIED. ) ;
#23387 = CARTESIAN_POINT ( 'NONE',  ( 21.85643539959774273, 11.87292600555486466, 1.968928953175947072 ) ) ;
#23388 = ORIENTED_EDGE ( 'NONE', *, *, #14342, .T. ) ;
#23389 = CARTESIAN_POINT ( 'NONE',  ( 5.200200943668277453, -29.53353846251400228, 7.690468881945117019 ) ) ;
#23390 = B_SPLINE_CURVE_WITH_KNOTS ( 'NONE', 3,
 ( #38076, #21629, #18943, #12754, #25332, #15234, #31509, #18313, #9052, #6600, #28406, #40342, #37654, #18728, #5979, #214, #12552, #34824 ),
 .UNSPECIFIED., .F., .F.,
 ( 4, 2, 2, 2, 2, 2, 2, 2, 4 ),
 ( 0.000000000000000000, 0.0007758045964606555527, 0.001551609192921311105, 0.003103218385842596624, 0.003879022982303238515, 0.004654827578763879106, 0.005430632175224520131, 0.005818534473454842378, 0.006206436771685162890 ),
 .UNSPECIFIED. ) ;
#23391 = ORIENTED_EDGE ( 'NONE', *, *, #20675, .T. ) ;
#23392 = CARTESIAN_POINT ( 'NONE',  ( 14.74088296503634155, -4.694786528388449121, 2.506211950836694680 ) ) ;
#23393 = CARTESIAN_POINT ( 'NONE',  ( -74.90697995311768409, -4.711520037844358022, -9.180746725924359808 ) ) ;
#23394 = ADVANCED_FACE ( 'NONE', ( #870, #13403 ), #25977, .T. ) ;
#23395 = CARTESIAN_POINT ( 'NONE',  ( 28.61591789821288145, 47.14532032487838364, -1.000000000000000000 ) ) ;
#23396 = FACE_OUTER_BOUND ( 'NONE', #32028, .T. ) ;
#23397 = CARTESIAN_POINT ( 'NONE',  ( 81.32777602152022212, 61.82240453612693187, 2.372413575842097444 ) ) ;
#23398 = LINE ( 'NONE', #1999, #21598 ) ;
#23399 = DIRECTION ( 'NONE',  ( -0.4999999999999999445, -0.8660254037844387076, 0.000000000000000000 ) ) ;
#23400 = CARTESIAN_POINT ( 'NONE',  ( -2.978675913592195190, -26.64985754041175525, 6.700000000000000178 ) ) ;
#23401 = CARTESIAN_POINT ( 'NONE',  ( -70.92837670882107659, -37.87473357531881391, -10.00000000000000888 ) ) ;
#23402 = AXIS2_PLACEMENT_3D ( 'NONE', #3243, #36968, #12464 ) ;
#23403 = AXIS2_PLACEMENT_3D ( 'NONE', #29401, #35788, #6971 ) ;
#23404 = CARTESIAN_POINT ( 'NONE',  ( -64.09292236773265472, 35.65892419719516226, 4.099996682510911761 ) ) ;
#23405 = CARTESIAN_POINT ( 'NONE',  ( 5.021324086407805254, -24.55319635012989110, 6.700000000000000178 ) ) ;
#23406 = CARTESIAN_POINT ( 'NONE',  ( 4.250519439829707480, -31.81867212404081968, 6.870716933885661959 ) ) ;
#23407 = CARTESIAN_POINT ( 'NONE',  ( -1.799609906766908685, -29.56993018339339940, 7.800000000000000711 ) ) ;
#23408 = CARTESIAN_POINT ( 'NONE',  ( 68.56660431458814742, 58.72100381882076192, 3.990501929453217134 ) ) ;
#23409 = CARTESIAN_POINT ( 'NONE',  ( 30.51572969112700306, -0.1387093445857095764, 4.969115662648612819 ) ) ;
#23410 = CIRCLE ( 'NONE', #26705, 1.000000000000000888 ) ;
#23411 = ADVANCED_FACE ( 'NONE', ( #23867 ), #36849, .F. ) ;
#23412 = ORIENTED_EDGE ( 'NONE', *, *, #29011, .F. ) ;
#23413 = CARTESIAN_POINT ( 'NONE',  ( 4.226378548430531623, -31.84575678386042341, 7.757178535559535959 ) ) ;
#23414 = CARTESIAN_POINT ( 'NONE',  ( 85.76961320806377387, 1.955528254085527662, 4.811735575706960866 ) ) ;
#23416 = CARTESIAN_POINT ( 'NONE',  ( -0.4007890326520501811, -26.77081244048443409, 6.931070083220551403 ) ) ;
#23415 = CARTESIAN_POINT ( 'NONE',  ( 78.66037426029973290, 66.03727662354840788, -1.183438861787455165 ) ) ;
#23417 = DIRECTION ( 'NONE',  ( 1.000000000000000000, 8.959828616340678715E-16, 0.000000000000000000 ) ) ;
#23418 = CARTESIAN_POINT ( 'NONE',  ( 2.308148104750579854, -26.12639665259444044, 7.767720160662275219 ) ) ;
#23419 = ORIENTED_EDGE ( 'NONE', *, *, #23159, .T. ) ;
#23420 = CARTESIAN_POINT ( 'NONE',  ( 1.713892699967800581, -32.96990337146582561, 7.635761828346577573 ) ) ;
#23421 = CARTESIAN_POINT ( 'NONE',  ( 23.71049985568843965, -7.011247657926062971, -2.558818689067067886 ) ) ;
#23422 = ORIENTED_EDGE ( 'NONE', *, *, #4826, .F. ) ;
#23423 = DIRECTION ( 'NONE',  ( -0.7660444431189726844, -0.6427876096865458022, -0.000000000000000000 ) ) ;
#23424 = CARTESIAN_POINT ( 'NONE',  ( 81.06392658325405876, 61.26538850743065012, -1.312782405654895568 ) ) ;
#23425 = EDGE_CURVE ( 'NONE', #38217, #10579, #20577, .T. ) ;
#23426 = LINE ( 'NONE', #29799, #2360 ) ;
#23427 = ADVANCED_FACE ( 'NONE', ( #11510 ), #11302, .T. ) ;
#23428 = CARTESIAN_POINT ( 'NONE',  ( 78.86912799350189118, 65.82616116372959425, 2.227525437860354174 ) ) ;
#23429 = CARTESIAN_POINT ( 'NONE',  ( 22.48842088587040777, 0.6138701667877143331, 6.557769318399328640 ) ) ;
#23431 = ORIENTED_EDGE ( 'NONE', *, *, #12369, .T. ) ;
#23430 = CARTESIAN_POINT ( 'NONE',  ( -0.7800240848564992113, -27.24451720821412337, 7.013842709614101167 ) ) ;
#23432 = EDGE_CURVE ( 'NONE', #14002, #22478, #34709, .T. ) ;
#23433 = CARTESIAN_POINT ( 'NONE',  ( 5.039926880157825195, -30.20828278875847062, 6.894806418505346812 ) ) ;
#23434 =( BOUNDED_SURFACE ( )  B_SPLINE_SURFACE ( 3, 2, ( 
 ( #35915, #1734, #13874 ),
 ( #26836, #29917, #1338 ),
 ( #23549, #32420, #39173 ),
 ( #29526, #29718, #929 ),
 ( #36114, #16948, #4219 ),
 ( #26245, #38968, #13463 ),
 ( #4811, #14265, #16740 ),
 ( #39376, #35323, #26441 ),
 ( #7891, #13675, #38777 ),
 ( #22755, #4424, #10767 ),
 ( #17339, #7091, #29324 ),
 ( #1141, #7490, #7694 ),
 ( #38571, #20243, #32825 ),
 ( #26037, #19655, #1527 ),
 ( #32227, #20443, #4616 ),
 ( #14062, #4027, #26639 ) ),
 .UNSPECIFIED., .F., .F., .T. ) 
 B_SPLINE_SURFACE_WITH_KNOTS ( ( 4, 2, 2, 2, 2, 2, 2, 4 ),
 ( 3, 3 ),
 ( 7.372574772901430151E-18, 0.0009755768803159638137, 0.001463365320473941980, 0.001951153760631920255, 0.002438942200789898530, 0.002926730640947876588, 0.003414519081105855079, 0.003902307521263833137 ),
 ( 0.000000000000000000, 1.000000000000000000 ),
 .UNSPECIFIED. ) 
 GEOMETRIC_REPRESENTATION_ITEM ( )  RATIONAL_B_SPLINE_SURFACE ( (
 ( 1.000000000000000000, 0.6029302108204159794, 1.000000000000000000),
 ( 1.000000000000000000, 0.5783298881758098808, 1.000000000000000000),
 ( 1.000000000000000000, 0.5522465926627553312, 1.000000000000000000),
 ( 1.000000000000000000, 0.5169885426014493301, 1.000000000000000000),
 ( 1.000000000000000000, 0.5061025709684141560, 1.000000000000000000),
 ( 1.000000000000000000, 0.4881721342722142309, 1.000000000000000000),
 ( 1.000000000000000000, 0.4810711757771862218, 1.000000000000000000),
 ( 1.000000000000000000, 0.4726640060677306798, 1.000000000000000000),
 ( 1.000000000000000000, 0.4715283203431685499, 1.000000000000000000),
 ( 1.000000000000000000, 0.4761415489114428357, 1.000000000000000000),
 ( 1.000000000000000000, 0.4818043763597766316, 1.000000000000000000),
 ( 1.000000000000000000, 0.4989518560459688667, 1.000000000000000000),
 ( 1.000000000000000000, 0.5102645520265423063, 1.000000000000000000),
 ( 1.000000000000000000, 0.5358562791028014249, 1.000000000000000000),
 ( 1.000000000000000000, 0.5501980292661743377, 1.000000000000000000),
 ( 1.000000000000000000, 0.5652620711642698526, 1.000000000000000000) ) ) 
 REPRESENTATION_ITEM ( '' )  SURFACE ( )  );
#23435 = CYLINDRICAL_SURFACE ( 'NONE', #11083, 0.1000000000000028644 ) ;
#23436 = CARTESIAN_POINT ( 'NONE',  ( -1.250501372580467230, -27.88106231952350100, 7.756377446753163873 ) ) ;
#23437 = AXIS2_PLACEMENT_3D ( 'NONE', #27719, #18037, #12058 ) ;
#23438 = CARTESIAN_POINT ( 'NONE',  ( 4.654912386708397243, -31.25244092439575994, 7.643333865083952183 ) ) ;
#23439 = CARTESIAN_POINT ( 'NONE',  ( 23.68965556879579992, 3.465983028975976321, -3.401521908042043130 ) ) ;
#23440 = ORIENTED_EDGE ( 'NONE', *, *, #1351, .F. ) ;
#23441 = DIRECTION ( 'NONE',  ( 0.000000000000000000, 0.000000000000000000, 1.000000000000000000 ) ) ;
#23442 = AXIS2_PLACEMENT_3D ( 'NONE', #31969, #10319, #16685 ) ;
#23443 = CARTESIAN_POINT ( 'NONE',  ( 22.81791704898701667, -6.824503531841428661, 2.299112860430994054 ) ) ;
#23444 = CARTESIAN_POINT ( 'NONE',  ( 3.147222565855531062, -32.76435434460020701, 7.501983001166816045 ) ) ;
#23445 = EDGE_CURVE ( 'NONE', #40382, #33795, #17690, .T. ) ;
#23446 = DIRECTION ( 'NONE',  ( 1.000000000000000000, 0.000000000000000000, 0.000000000000000000 ) ) ;
#23447 = CARTESIAN_POINT ( 'NONE',  ( 78.68244131272049913, 66.05295088176870877, 1.094381639753830182 ) ) ;
#23448 = CARTESIAN_POINT ( 'NONE',  ( 88.51539661956502414, -1.738042312505858389, 3.005881034771096250 ) ) ;
#23449 = CARTESIAN_POINT ( 'NONE',  ( 5.123392144880668297, -30.30003903553068767, 7.751599049952197618 ) ) ;
#23450 = EDGE_LOOP ( 'NONE', ( #32935, #8464, #9882, #856 ) ) ;
#23451 = CARTESIAN_POINT ( 'NONE',  ( -75.45330471031414277, 33.71485196875532608, 12.49999999999999645 ) ) ;
#23452 = CARTESIAN_POINT ( 'NONE',  ( 24.15140053283135657, 3.654133365256820198, -2.050164366749841260 ) ) ;
#23453 = CARTESIAN_POINT ( 'NONE',  ( 16.00230772547182667, -3.352604421649032940, -2.703945156471453171 ) ) ;
#23454 = CARTESIAN_POINT ( 'NONE',  ( 35.78589809970488034, -3.160013725310466981, -5.791652902311821727 ) ) ;
#23455 = CARTESIAN_POINT ( 'NONE',  ( -64.08758708074093136, -65.19654454972992141, 2.999999999999999112 ) ) ;
#23456 = CARTESIAN_POINT ( 'NONE',  ( 84.10558833958633329, 3.011200051076408091, -0.2484360993799872019 ) ) ;
#23457 = CARTESIAN_POINT ( 'NONE',  ( -0.5074448109832514486, -26.98430194541812099, 7.730758795053803922 ) ) ;
#23458 = ORIENTED_EDGE ( 'NONE', *, *, #33048, .F. ) ;
#23459 = CARTESIAN_POINT ( 'NONE',  ( 2.277491769660097365, -26.21926552469281191, 7.635761828346577573 ) ) ;
#23460 = EDGE_CURVE ( 'NONE', #7585, #22592, #26373, .T. ) ;
#23461 = LINE ( 'NONE', #35436, #11212 ) ;
#23462 = AXIS2_PLACEMENT_3D ( 'NONE', #28663, #6435, #469 ) ;
#23463 = ORIENTED_EDGE ( 'NONE', *, *, #23927, .F. ) ;
#23464 = VERTEX_POINT ( 'NONE', #17477 ) ;
#23465 = CARTESIAN_POINT ( 'NONE',  ( 27.81686590159541694, 1.845386698342884602, 3.904314145750329867 ) ) ;
#23466 = CARTESIAN_POINT ( 'NONE',  ( -1.642550015356792681, -30.60663237321507069, 7.013842709614101167 ) ) ;
#23467 = CIRCLE ( 'NONE', #4415, 0.1000000000000028644 ) ;
#23468 = FACE_OUTER_BOUND ( 'NONE', #30911, .T. ) ;
#23469 = CIRCLE ( 'NONE', #19537, 0.1000000000000028644 ) ;
#23470 = EDGE_CURVE ( 'NONE', #37250, #13245, #19337, .T. ) ;
#23471 = DIRECTION ( 'NONE',  ( 0.000000000000000000, 0.000000000000000000, 1.000000000000000000 ) ) ;
#23472 = AXIS2_PLACEMENT_3D ( 'NONE', #4280, #29186, #29387 ) ;
#23473 = ORIENTED_EDGE ( 'NONE', *, *, #24312, .F. ) ;
#23474 = EDGE_CURVE ( 'NONE', #5710, #23332, #955, .T. ) ;
#23475 = CARTESIAN_POINT ( 'NONE',  ( 4.911690090265110165, -28.45299136274915952, 6.894806418505345924 ) ) ;
#23476 = ORIENTED_EDGE ( 'NONE', *, *, #8628, .T. ) ;
#23477 = CARTESIAN_POINT ( 'NONE',  ( -56.31571917568489738, 30.58480147475593114, -3.912689169536864853 ) ) ;
#23478 = CARTESIAN_POINT ( 'NONE',  ( 4.787516329918978464, -27.92079356116780886, 6.865482280155368322 ) ) ;
#23479 = ORIENTED_EDGE ( 'NONE', *, *, #39734, .F. ) ;
#23480 = CARTESIAN_POINT ( 'NONE',  ( 24.40726884955499543, 2.958944204706972503, 3.690054115108988952 ) ) ;
#23481 = EDGE_CURVE ( 'NONE', #11841, #8794, #10910, .T. ) ;
#23482 = CARTESIAN_POINT ( 'NONE',  ( 80.32635178447517887, 66.28770415027543095, -1.483157530539362279 ) ) ;
#23483 = DIRECTION ( 'NONE',  ( -0.9848077530122067991, -0.1736481776669374644, -0.000000000000000000 ) ) ;
#23484 = CARTESIAN_POINT ( 'NONE',  ( -1.226003372003152458, -31.30088982666143949, 7.691066658568947112 ) ) ;
#23485 = ORIENTED_EDGE ( 'NONE', *, *, #18053, .T. ) ;
#23487 = CARTESIAN_POINT ( 'NONE',  ( -4.890026461918812295, -8.951974136083761024, 6.000000000000000000 ) ) ;
#23486 = CARTESIAN_POINT ( 'NONE',  ( -20.34874870218063947, -26.64985754041175525, 6.700000000000000178 ) ) ;
#23488 = CARTESIAN_POINT ( 'NONE',  ( 21.38476492232890180, 5.476885306300394163, -3.544007777260224312 ) ) ;
#23489 = CARTESIAN_POINT ( 'NONE',  ( 75.80265905884337485, 60.84868533121094458, 3.810661578667723148 ) ) ;
#23490 = ORIENTED_EDGE ( 'NONE', *, *, #32049, .F. ) ;
#23491 = CARTESIAN_POINT ( 'NONE',  ( 24.25544397694150689, 2.781918247062924898, -3.883429013402408536 ) ) ;
#23492 = CARTESIAN_POINT ( 'NONE',  ( -62.92837670882106238, -42.37473357531882812, 6.000000000000000000 ) ) ;
#23493 = VECTOR ( 'NONE', #174, 1000.000000000000114 ) ;
#23494 = DIRECTION ( 'NONE',  ( -0.000000000000000000, -0.000000000000000000, -1.000000000000000000 ) ) ;
#23495 = LINE ( 'NONE', #4371, #5234 ) ;
#23496 = CARTESIAN_POINT ( 'NONE',  ( -63.58520484588292732, 35.72026407271187765, 6.999999999999999112 ) ) ;
#23497 = CARTESIAN_POINT ( 'NONE',  ( -70.82888935184436718, -48.61702805680357642, 6.000000000000001776 ) ) ;
#23498 = CARTESIAN_POINT ( 'NONE',  ( 81.94117896397187906, 62.33638752673003580, 2.166533184762200026 ) ) ;
#23499 = CARTESIAN_POINT ( 'NONE',  ( 85.68874278272487288, 2.108061670072472360, -3.902156445801064244 ) ) ;
#23500 = CARTESIAN_POINT ( 'NONE',  ( 29.60215801812428182, 1.109421360397880862, -4.380391640306282142 ) ) ;
#23501 = AXIS2_PLACEMENT_3D ( 'NONE', #21100, #11394, #17367 ) ;
#23502 = FACE_OUTER_BOUND ( 'NONE', #12725, .T. ) ;
#23503 = AXIS2_PLACEMENT_3D ( 'NONE', #6452, #22310, #37710 ) ;
#23504 = CARTESIAN_POINT ( 'NONE',  ( -60.75950795826495465, 23.17721540975219341, 15.50000000000000000 ) ) ;
#23505 = VECTOR ( 'NONE', #37137, 1000.000000000000227 ) ;
#23506 = CARTESIAN_POINT ( 'NONE',  ( -74.03009556761388410, -1.796639617249599086, -10.77097688889393190 ) ) ;
#23507 = ORIENTED_EDGE ( 'NONE', *, *, #22914, .F. ) ;
#23508 = CARTESIAN_POINT ( 'NONE',  ( 11.65737507970504616, -38.28842912540938670, 6.800000000000000711 ) ) ;
#23509 = CARTESIAN_POINT ( 'NONE',  ( 0.1158819994041509066, -26.44913956231825480, 6.980586498568971621 ) ) ;
#23510 = CARTESIAN_POINT ( 'NONE',  ( 34.77080612335073795, -3.235625644562878822, -5.633223249305419067 ) ) ;
#23511 = DIRECTION ( 'NONE',  ( 0.3757233601570931225, 0.9267318687906784813, 0.000000000000000000 ) ) ;
#23512 = CARTESIAN_POINT ( 'NONE',  ( 4.977103583311326851, -28.33982894766831606, 7.710604733652631992 ) ) ;
#23513 = CARTESIAN_POINT ( 'NONE',  ( -1.594457770366995319, -28.38926191680453925, 7.750000000000000888 ) ) ;
#23514 = EDGE_CURVE ( 'NONE', #40141, #21412, #33163, .T. ) ;
#23515 = FACE_OUTER_BOUND ( 'NONE', #19278, .T. ) ;
#23516 = ORIENTED_EDGE ( 'NONE', *, *, #32881, .F. ) ;
#23517 = CARTESIAN_POINT ( 'NONE',  ( 25.58352385666275097, 2.439062859384895532, 4.005113320270204724 ) ) ;
#23518 = CARTESIAN_POINT ( 'NONE',  ( -70.59363788503038961, 0.1660198011701667642, 3.991660656778088789 ) ) ;
#23519 = CARTESIAN_POINT ( 'NONE',  ( 67.10699435067097340, 58.18157613906911507, -3.995511504169226402 ) ) ;
#23520 = CARTESIAN_POINT ( 'NONE',  ( 3.055030623276686619, -26.34271016697629619, 7.013842709614101167 ) ) ;
#23521 = CIRCLE ( 'NONE', #30799, 0.9999999999999991118 ) ;
#23522 = EDGE_LOOP ( 'NONE', ( #20821, #23058, #16968, #23171 ) ) ;
#23523 = DIRECTION ( 'NONE',  ( -1.000000000000000000, 0.000000000000000000, -0.000000000000000000 ) ) ;
#23524 = CARTESIAN_POINT ( 'NONE',  ( 3.816341850769968236, -32.23127348326596575, 7.778050822775631090 ) ) ;
#23525 = CARTESIAN_POINT ( 'NONE',  ( 5.900850858889974404, -30.34709628986367846, 7.695279973900954751 ) ) ;
#23526 = CARTESIAN_POINT ( 'NONE',  ( 5.048915835387577822, -28.55141393210982415, 6.980586498568967180 ) ) ;
#23527 = CARTESIAN_POINT ( 'NONE',  ( -70.17638756726756810, -48.41860179101485073, 9.972019997609882225 ) ) ;
#23528 = CARTESIAN_POINT ( 'NONE',  ( 3.021324086407803478, -24.55319635012989110, 6.700000000000000178 ) ) ;
#23529 = VECTOR ( 'NONE', #6587, 1000.000000000000000 ) ;
#23530 = CARTESIAN_POINT ( 'NONE',  ( 1.280274463769470294, -26.09523354690790242, 6.931070083220559397 ) ) ;
#23531 = ORIENTED_EDGE ( 'NONE', *, *, #18724, .F. ) ;
#23532 = CARTESIAN_POINT ( 'NONE',  ( 23.43077426150285092, 3.780410721560847342, 3.135869166350258919 ) ) ;
#23533 = EDGE_CURVE ( 'NONE', #10351, #22200, #31776, .T. ) ;
#23534 = DIRECTION ( 'NONE',  ( -3.491481338843133750E-15, 1.000000000000000000, -0.000000000000000000 ) ) ;
#23535 = CARTESIAN_POINT ( 'NONE',  ( 80.77858121287650306, 63.01782502344085657, 3.459421039841293233 ) ) ;
#23536 = EDGE_CURVE ( 'NONE', #26273, #29514, #18024, .T. ) ;
#23537 = DIRECTION ( 'NONE',  ( -1.000000000000000000, 0.000000000000000000, 0.000000000000000000 ) ) ;
#23538 = ORIENTED_EDGE ( 'NONE', *, *, #35756, .T. ) ;
#23539 = CARTESIAN_POINT ( 'NONE',  ( 79.36485406729210013, 60.67242113316871155, -2.285396881590245677 ) ) ;
#23541 = CARTESIAN_POINT ( 'NONE',  ( 14.76643007562886112, -4.521128121716065706, -2.511026874211885751 ) ) ;
#23540 = CARTESIAN_POINT ( 'NONE',  ( 22.60888406660597028, 0.2903629327645729230, 6.504315945443690516 ) ) ;
#23542 = CARTESIAN_POINT ( 'NONE',  ( 78.83984420990714170, 66.12288285737325566, -1.382728580142345454 ) ) ;
#23543 = CARTESIAN_POINT ( 'NONE',  ( 78.08876170118931270, 64.69829802809502439, 3.164065397988977235 ) ) ;
#23544 = VERTEX_POINT ( 'NONE', #3322 ) ;
#23545 = CARTESIAN_POINT ( 'NONE',  ( -0.8455530167579952128, -27.31644983497921331, 7.778050822775635531 ) ) ;
#23546 = CARTESIAN_POINT ( 'NONE',  ( 80.32635178447536362, 66.28770415027547358, 1.483157530538789626 ) ) ;
#23547 = CARTESIAN_POINT ( 'NONE',  ( -89.00859394718985129, 2.429809908903242555, 15.50000000000000000 ) ) ;
#23548 = CARTESIAN_POINT ( 'NONE',  ( 27.76889013493211067, -0.3210463222110187531, 6.029547961152755597 ) ) ;
#23549 = CARTESIAN_POINT ( 'NONE',  ( -62.75216693000847101, 36.25077706935577027, -4.893820751806843283 ) ) ;
#23550 = ORIENTED_EDGE ( 'NONE', *, *, #39719, .F. ) ;
#23551 = DIRECTION ( 'NONE',  ( -0.000000000000000000, -0.000000000000000000, 1.000000000000000000 ) ) ;
#23552 = CARTESIAN_POINT ( 'NONE',  ( 21.73423954385304668, 0.2273991419590928875, -9.075701020149493203 ) ) ;
#23553 = DIRECTION ( 'NONE',  ( -1.000000000000000000, 0.000000000000000000, 0.000000000000000000 ) ) ;
#23554 = VERTEX_POINT ( 'NONE', #15224 ) ;
#23555 = CARTESIAN_POINT ( 'NONE',  ( 5.169453744383599059, -29.10560552944284396, 6.875780273367533724 ) ) ;
#23556 = ORIENTED_EDGE ( 'NONE', *, *, #30019, .F. ) ;
#23557 = CARTESIAN_POINT ( 'NONE',  ( 34.63600047421554962, -0.7840873862764304869, -5.277546382571144612 ) ) ;
#23558 = PLANE ( 'NONE',  #16088 ) ;
#23559 = CARTESIAN_POINT ( 'NONE',  ( 3.281055722528557705, -32.69266877113672365, 6.961115707816233567 ) ) ;
#23560 = CARTESIAN_POINT ( 'NONE',  ( -65.04872026876938662, 34.92042435966252611, -6.752913741461258113 ) ) ;
#23561 = DIRECTION ( 'NONE',  ( 0.8820753183692410238, -0.4711084086744811161, 0.000000000000000000 ) ) ;
#23562 = PLANE ( 'NONE',  #7255 ) ;
#23563 = VECTOR ( 'NONE', #32638, 1000.000000000000227 ) ;
#23564 = CARTESIAN_POINT ( 'NONE',  ( -29.07867591359219617, -24.55319635012989110, 6.700000000000000178 ) ) ;
#23565 = ORIENTED_EDGE ( 'NONE', *, *, #26189, .T. ) ;
#23566 = CARTESIAN_POINT ( 'NONE',  ( 66.27376694608996388, 57.73522568913447373, 4.000000000000000000 ) ) ;
#23567 = CARTESIAN_POINT ( 'NONE',  ( 72.17048485476517783, 59.77360812419138369, -3.955776929930289398 ) ) ;
#23568 = EDGE_LOOP ( 'NONE', ( #5552, #23650 ) ) ;
#23569 = CARTESIAN_POINT ( 'NONE',  ( 87.73180046618776373, -1.932853647757891258, -3.545598201197500465 ) ) ;
#23570 = AXIS2_PLACEMENT_3D ( 'NONE', #24359, #18173, #30764 ) ;
#23571 = CARTESIAN_POINT ( 'NONE',  ( -14.97867591359219119, -24.55319635012989110, 6.700000000000000178 ) ) ;
#23572 = AXIS2_PLACEMENT_3D ( 'NONE', #1525, #13872, #14059 ) ;
#23573 = CARTESIAN_POINT ( 'NONE',  ( -0.9325302353475311001, -27.26388753469717940, 6.867280401193709416 ) ) ;
#23574 = DIRECTION ( 'NONE',  ( 0.000000000000000000, 0.000000000000000000, -1.000000000000000000 ) ) ;
#23575 = CARTESIAN_POINT ( 'NONE',  ( -1.796521113867400654, -29.56993018341788826, 7.767301406056523305 ) ) ;
#23576 = CARTESIAN_POINT ( 'NONE',  ( -10.44874870218064089, -26.64985754041175525, 6.700000000000000178 ) ) ;
#23577 = ADVANCED_FACE ( 'NONE', ( #21620 ), #6385, .F. ) ;
#23578 = DIRECTION ( 'NONE',  ( 0.000000000000000000, 0.000000000000000000, 1.000000000000000000 ) ) ;
#23579 = EDGE_CURVE ( 'NONE', #15644, #37970, #37448, .T. ) ;
#23580 = ORIENTED_EDGE ( 'NONE', *, *, #27271, .F. ) ;
#23581 = CARTESIAN_POINT ( 'NONE',  ( 80.62899510017081184, 61.84672251665477205, -2.918211652848216264 ) ) ;
#23582 = CARTESIAN_POINT ( 'NONE',  ( 33.75147498838597215, -4.699296933879914206, 3.805678930683413785 ) ) ;
#23583 = CARTESIAN_POINT ( 'NONE',  ( 80.32689410753103232, 62.53373119284189130, 3.467090974304449347 ) ) ;
#23585 = ORIENTED_EDGE ( 'NONE', *, *, #36035, .T. ) ;
#23584 = CARTESIAN_POINT ( 'NONE',  ( 25.01091293555841233, 3.329590545877085805, 1.936828124349011526 ) ) ;
#23586 = AXIS2_PLACEMENT_3D ( 'NONE', #549, #25645, #19864 ) ;
#23587 = CARTESIAN_POINT ( 'NONE',  ( 0.3896649785617538608, -32.81498557016907114, 7.754798119455333705 ) ) ;
#23588 = CARTESIAN_POINT ( 'NONE',  ( 3.949132033880527803, -27.01980083679679723, 6.870716933885664623 ) ) ;
#23589 = CARTESIAN_POINT ( 'NONE',  ( 17.35285164467449093, 14.28221863251290991, 2.500000000000000000 ) ) ;
#23590 = CARTESIAN_POINT ( 'NONE',  ( 21.85643539959775339, 6.533355437427212919, 10.99619876466361212 ) ) ;
#23591 = ORIENTED_EDGE ( 'NONE', *, *, #9205, .F. ) ;
#23592 = CARTESIAN_POINT ( 'NONE',  ( 76.21224277836739702, 64.31709241891930162, -2.649705962983377461 ) ) ;
#23593 = CARTESIAN_POINT ( 'NONE',  ( 14.76814867959672739, -5.160745194441147099, 2.500000607217906623 ) ) ;
#23594 = CARTESIAN_POINT ( 'NONE',  ( -76.81575550944289432, 9.394122235356590522, -9.604269881316103152 ) ) ;
#23595 = CARTESIAN_POINT ( 'NONE',  ( 1.527538316465248291, -32.96553355588380185, 6.882085323592685100 ) ) ;
#23596 = CARTESIAN_POINT ( 'NONE',  ( 2.468116271650433902, -26.25773128481726459, 6.887945620086119547 ) ) ;
#23597 = CARTESIAN_POINT ( 'NONE',  ( 81.02128870047407361, 63.12856183665077481, 3.380792992375197148 ) ) ;
#23598 = DIRECTION ( 'NONE',  ( 1.000000000000000000, 0.000000000000000000, 0.000000000000000000 ) ) ;
#23599 = CARTESIAN_POINT ( 'NONE',  ( 3.858201203583684791, -26.94241211265677194, 7.695279973900954751 ) ) ;
#23600 = DIRECTION ( 'NONE',  ( -0.000000000000000000, -0.000000000000000000, 1.000000000000000000 ) ) ;
#23601 = CARTESIAN_POINT ( 'NONE',  ( 0.5732355268899250733, -26.25637850312180177, 6.867280401193708528 ) ) ;
#23602 = EDGE_CURVE ( 'NONE', #1810, #12640, #25924, .T. ) ;
#23603 = CARTESIAN_POINT ( 'NONE',  ( 3.977009164777316919, -32.22831426950175882, 7.710604733652632881 ) ) ;
#23604 = FACE_BOUND ( 'NONE', #9329, .T. ) ;
#23605 = CARTESIAN_POINT ( 'NONE',  ( -70.92837670882107659, 26.72470171467712063, 0.000000000000000000 ) ) ;
#23606 = CARTESIAN_POINT ( 'NONE',  ( 67.77942698303134250, 58.15829091545840157, 3.995247128881094678 ) ) ;
#23607 = ADVANCED_FACE ( 'NONE', ( #34200 ), #28398, .F. ) ;
#23608 = DIRECTION ( 'NONE',  ( 0.5000000000000101030, -0.8660254037844328234, -0.000000000000000000 ) ) ;
#23609 = CARTESIAN_POINT ( 'NONE',  ( 84.99141033049929206, 2.891338577806874088, -0.4625859348280507155 ) ) ;
#23611 = CARTESIAN_POINT ( 'NONE',  ( 31.02916373834690944, -0.3132898623965780782, -5.049249463166630925 ) ) ;
#23610 = CARTESIAN_POINT ( 'NONE',  ( 79.96011558216464721, 64.80970700093439518, -3.432259906339275801 ) ) ;
#23612 = CARTESIAN_POINT ( 'NONE',  ( -21.07867591359219617, -26.64985754041175525, 6.800000000000000711 ) ) ;
#23613 = CARTESIAN_POINT ( 'NONE',  ( -58.93521193748835429, 27.64319143539499279, 6.467610917687007799 ) ) ;
#23614 = ORIENTED_EDGE ( 'NONE', *, *, #32002, .F. ) ;
#23615 = CARTESIAN_POINT ( 'NONE',  ( -78.88273507863694078, 11.42845723122414014, -6.074662874054942208 ) ) ;
#23616 = CARTESIAN_POINT ( 'NONE',  ( 1.296126803379346715, -26.19404450011727548, 6.895222827070020877 ) ) ;
#23617 = B_SPLINE_CURVE_WITH_KNOTS ( 'NONE', 3,
 ( #15296, #21279, #18576, #27848 ),
 .UNSPECIFIED., .F., .F.,
 ( 4, 4 ),
 ( 0.000000000000000000, 6.391136169994552113E-06 ),
 .UNSPECIFIED. ) ;
#23618 = ORIENTED_EDGE ( 'NONE', *, *, #7385, .F. ) ;
#23619 = ORIENTED_EDGE ( 'NONE', *, *, #16173, .F. ) ;
#23620 = ADVANCED_FACE ( 'NONE', ( #3121 ), #40136, .F. ) ;
#23621 = CARTESIAN_POINT ( 'NONE',  ( 78.86912799350172065, 65.82616116372945214, -2.227525437860510937 ) ) ;
#23622 = CARTESIAN_POINT ( 'NONE',  ( 24.90974289849040346, 3.541794099149180752, -0.3255497437964431917 ) ) ;
#23623 = CARTESIAN_POINT ( 'NONE',  ( 79.41630106684688428, 65.17102571570140412, 3.206617288017371337 ) ) ;
#23624 = CARTESIAN_POINT ( 'NONE',  ( 25.66178649468485773, 1.154831409588704227, 4.432321438749628584 ) ) ;
#23626 = ORIENTED_EDGE ( 'NONE', *, *, #38478, .T. ) ;
#23625 = DIRECTION ( 'NONE',  ( 0.000000000000000000, 0.000000000000000000, 1.000000000000000000 ) ) ;
#23627 = CARTESIAN_POINT ( 'NONE',  ( 5.039465595983135593, -30.21069599340067313, 6.892063359921932530 ) ) ;
#23628 = LINE ( 'NONE', #36192, #14027 ) ;
#23629 = CARTESIAN_POINT ( 'NONE',  ( -1.198187176124504205, -27.79278364650808442, 7.778050822775631978 ) ) ;
#23630 = FACE_OUTER_BOUND ( 'NONE', #16615, .T. ) ;
#23631 = CARTESIAN_POINT ( 'NONE',  ( 22.36345331109650658, 4.261471805455568251, -3.688296226855283688 ) ) ;
#23632 = ORIENTED_EDGE ( 'NONE', *, *, #30264, .F. ) ;
#23633 = CARTESIAN_POINT ( 'NONE',  ( 2.342808000876349439, -33.01046787075163280, 7.710604733652627552 ) ) ;
#23634 = CARTESIAN_POINT ( 'NONE',  ( 22.31758782591801094, 6.227955964823622459, -0.6941013191108784675 ) ) ;
#23635 = CARTESIAN_POINT ( 'NONE',  ( 17.55902044582588672, 11.95912233719816342, 2.500000000000000444 ) ) ;
#23636 = CARTESIAN_POINT ( 'NONE',  ( -62.92837670882106238, -23.80776546975053520, -6.000000000000000000 ) ) ;
#23637 = CARTESIAN_POINT ( 'NONE',  ( 81.49447160051045103, 61.73183938760540457, 1.953285432047543901 ) ) ;
#23638 = CARTESIAN_POINT ( 'NONE',  ( 84.57067941792149668, 3.126724152278200997, 0.3173792860121260051 ) ) ;
#23639 = ORIENTED_EDGE ( 'NONE', *, *, #5175, .F. ) ;
#23640 = CARTESIAN_POINT ( 'NONE',  ( -1.699609906766908596, -29.56993018339339940, 7.767301406074262893 ) ) ;
#23641 = EDGE_CURVE ( 'NONE', #20410, #4296, #39621, .T. ) ;
#23642 = CARTESIAN_POINT ( 'NONE',  ( 21.65999089574924596, 6.756737864946346761, -2.827852530117774599 ) ) ;
#23643 = AXIS2_PLACEMENT_3D ( 'NONE', #20178, #7823, #29652 ) ;
#23644 = CARTESIAN_POINT ( 'NONE',  ( 26.27455094472032116, -3.204942025804789818, -4.209323993755259785 ) ) ;
#23645 = CARTESIAN_POINT ( 'NONE',  ( 35.86862426242751667, -2.087724560567193244, -5.804564320744471040 ) ) ;
#23646 = CARTESIAN_POINT ( 'NONE',  ( -14.97867591359219119, -24.55319635012989110, 6.700000000000000178 ) ) ;
#23647 = CARTESIAN_POINT ( 'NONE',  ( 22.04842757576495771, 0.2902497289493954358, -7.510401919737763166 ) ) ;
#23648 = EDGE_CURVE ( 'NONE', #3677, #10008, #37251, .T. ) ;
#23649 = DIRECTION ( 'NONE',  ( 0.000000000000000000, 0.000000000000000000, 1.000000000000000000 ) ) ;
#23650 = ORIENTED_EDGE ( 'NONE', *, *, #18319, .F. ) ;
#23651 = CARTESIAN_POINT ( 'NONE',  ( 33.62635108579966925, -1.235446387465426898, 5.454603361950056239 ) ) ;
#23652 = EDGE_CURVE ( 'NONE', #12335, #20068, #37745, .T. ) ;
#23653 = CARTESIAN_POINT ( 'NONE',  ( -5.316495087772349137, -32.84709638682603838, 6.000000000000000888 ) ) ;
#23654 = EDGE_CURVE ( 'NONE', #35786, #212, #35804, .T. ) ;
#23655 = CARTESIAN_POINT ( 'NONE',  ( -1.133537450598582241, -27.69140558245994654, 6.959317978105168834 ) ) ;
#23656 = ORIENTED_EDGE ( 'NONE', *, *, #35540, .T. ) ;
#23657 = VERTEX_POINT ( 'NONE', #34608 ) ;
#23658 = CARTESIAN_POINT ( 'NONE',  ( 27.81619187117563996, 1.844502997120055054, 3.906579784159712965 ) ) ;
#23659 = CARTESIAN_POINT ( 'NONE',  ( -1.644731256756654769, -30.59959515653206097, 6.903112506833887885 ) ) ;
#23660 = CARTESIAN_POINT ( 'NONE',  ( 87.45260826627337281, -1.934911646089722659, 3.714069959888173234 ) ) ;
#23661 = ORIENTED_EDGE ( 'NONE', *, *, #36793, .F. ) ;
#23662 = DIRECTION ( 'NONE',  ( 0.000000000000000000, 0.000000000000000000, -1.000000000000000000 ) ) ;
#23663 = EDGE_CURVE ( 'NONE', #37345, #9551, #29183, .T. ) ;
#23664 = FACE_OUTER_BOUND ( 'NONE', #25351, .T. ) ;
#23665 =( NAMED_UNIT ( * ) PLANE_ANGLE_UNIT ( ) SI_UNIT ( $, .RADIAN. ) );
#23666 =( BOUNDED_CURVE ( )  B_SPLINE_CURVE ( 3, ( #4936, #14392, #10897, #36041 ),
 .UNSPECIFIED., .F., .T. ) 
 B_SPLINE_CURVE_WITH_KNOTS ( ( 4, 4 ),
 ( 1.381924640371168245, 1.574767692156076482 ),
 .UNSPECIFIED. ) 
 CURVE ( )  GEOMETRIC_REPRESENTATION_ITEM ( )  RATIONAL_B_SPLINE_CURVE ( ( 1.000000000000000000, 0.9969033633783032089, 0.9969033633783032089, 1.000000000000000000 ) ) 
 REPRESENTATION_ITEM ( '' )  );
#23667 = EDGE_LOOP ( 'NONE', ( #6230, #15129, #3668, #19451 ) ) ;
#23668 = CARTESIAN_POINT ( 'NONE',  ( -57.97698207090199674, 31.94645990616745834, -4.307980060361010999 ) ) ;
#23669 = ORIENTED_EDGE ( 'NONE', *, *, #14340, .T. ) ;
#23671 = CARTESIAN_POINT ( 'NONE',  ( 4.306781708726275859, -27.38664762112922446, 7.769368695748487319 ) ) ;
#23670 = CARTESIAN_POINT ( 'NONE',  ( 4.805696999878964704, -27.95526195095927591, 6.880828092187096345 ) ) ;
#23672 = EDGE_LOOP ( 'NONE', ( #20663, #18474, #8819, #2564 ) ) ;
#23673 = CARTESIAN_POINT ( 'NONE',  ( 24.47679419834368275, 2.965539177225203105, 3.653982106517862594 ) ) ;
#23674 = CARTESIAN_POINT ( 'NONE',  ( 82.16223423120655411, 62.72759567084518295, -2.080779877698640146 ) ) ;
#23675 = CIRCLE ( 'NONE', #24994, 0.1000000000000028644 ) ;
#23676 = LINE ( 'NONE', #7423, #10114 ) ;
#23677 = ORIENTED_EDGE ( 'NONE', *, *, #28081, .T. ) ;
#23679 = CARTESIAN_POINT ( 'NONE',  ( 16.02007836965137955, -3.385103570282511409, -2.706718695280325715 ) ) ;
#23678 = CARTESIAN_POINT ( 'NONE',  ( 0.03514138663457523626, -26.60563578670519291, 7.784838882742139532 ) ) ;
#23680 = CARTESIAN_POINT ( 'NONE',  ( -9.078675913592196167, -26.64985754041175525, 6.800000000000000711 ) ) ;
#23681 = CARTESIAN_POINT ( 'NONE',  ( 74.58877118170933329, 61.99488014651142009, 3.786335567263263702 ) ) ;
#23682 = CARTESIAN_POINT ( 'NONE',  ( 22.25539530137726274, 2.842831528157699683, -4.834828159471090459 ) ) ;
#23683 = ORIENTED_EDGE ( 'NONE', *, *, #2396, .T. ) ;
#23684 = CARTESIAN_POINT ( 'NONE',  ( -62.96463773297387689, 37.71389135159058270, 4.136849086241030982 ) ) ;
#23685 = FACE_OUTER_BOUND ( 'NONE', #29657, .T. ) ;
#23686 = DIRECTION ( 'NONE',  ( 0.6427876096865481337, -0.7660444431189707970, -0.000000000000000000 ) ) ;
#23687 = PLANE ( 'NONE',  #10428 ) ;
#23688 = PLANE ( 'NONE',  #15566 ) ;
#23689 = CARTESIAN_POINT ( 'NONE',  ( 82.00886418671287004, 63.26204695399094646, 2.636331425444717436 ) ) ;
#23690 = CARTESIAN_POINT ( 'NONE',  ( 85.45255010372768822, 2.373364497502822967, 3.195069691434311743 ) ) ;
#23691 = CARTESIAN_POINT ( 'NONE',  ( 28.57954844588206811, 0.5947805351201630453, 5.396286122280502084 ) ) ;
#23692 = CARTESIAN_POINT ( 'NONE',  ( 4.336009428051142756, -27.42202173051807890, 6.894806418505345924 ) ) ;
#23693 = CARTESIAN_POINT ( 'NONE',  ( 4.654215647715354010, -31.25365064525384540, 7.748216051605115950 ) ) ;
#23694 = CARTESIAN_POINT ( 'NONE',  ( -80.93982711156188259, -5.651589301102212026, -4.572683551290904980 ) ) ;
#23695 = CYLINDRICAL_SURFACE ( 'NONE', #31019, 0.09010775117052960415 ) ;
#23696 = DIRECTION ( 'NONE',  ( 0.000000000000000000, 0.000000000000000000, -1.000000000000000000 ) ) ;
#23697 = EDGE_CURVE ( 'NONE', #22592, #9154, #33992, .T. ) ;
#23698 = CARTESIAN_POINT ( 'NONE',  ( 37.07725246739935443, -2.790096878235085676, -5.993199982913866464 ) ) ;
#23699 = SURFACE_SIDE_STYLE ('',( #8652 ) ) ;
#23700 = CARTESIAN_POINT ( 'NONE',  ( 4.977925439032924615, -28.34201439931610977, 7.720710062488894465 ) ) ;
#23701 = EDGE_CURVE ( 'NONE', #21833, #8080, #39102, .T. ) ;
#23702 = DIRECTION ( 'NONE',  ( 1.000000000000000000, 0.000000000000000000, 0.000000000000000000 ) ) ;
#23703 = EDGE_CURVE ( 'NONE', #14078, #3561, #8620, .T. ) ;
#23704 = DIRECTION ( 'NONE',  ( -0.7660444431189725734, -0.6427876096865456912, -0.000000000000000000 ) ) ;
#23705 = AXIS2_PLACEMENT_3D ( 'NONE', #17109, #32791, #13425 ) ;
#23706 = ORIENTED_EDGE ( 'NONE', *, *, #19159, .F. ) ;
#23707 = CARTESIAN_POINT ( 'NONE',  ( 34.13106453884969227, -3.728238084256084495, 5.351387154442956096 ) ) ;
#23708 = CARTESIAN_POINT ( 'NONE',  ( -70.39213229241123315, 0.06107131307206801335, 3.975988782274378686 ) ) ;
#23709 = CARTESIAN_POINT ( 'NONE',  ( 67.05715689120697220, 57.86208461462646113, -3.995640437668404932 ) ) ;
#23710 = LINE ( 'NONE', #11337, #28642 ) ;
#23711 = ORIENTED_EDGE ( 'NONE', *, *, #38016, .T. ) ;
#23712 = CARTESIAN_POINT ( 'NONE',  ( -0.4625701342256395288, -32.19321274608519445, 7.730758795053800370 ) ) ;
#23713 = LINE ( 'NONE', #4987, #4863 ) ;
#23714 = CARTESIAN_POINT ( 'NONE',  ( 77.97569881417399529, 65.55229714878629466, 1.909807370998233722 ) ) ;
#23715 = DIRECTION ( 'NONE',  ( 0.000000000000000000, -1.000000000000000000, 0.000000000000000000 ) ) ;
#23716 = CARTESIAN_POINT ( 'NONE',  ( 3.604513180742714429, -26.63320592762521244, 6.998987538705435441 ) ) ;
#23717 = LINE ( 'NONE', #24118, #37628 ) ;
#23718 = VERTEX_POINT ( 'NONE', #4116 ) ;
#23719 = CARTESIAN_POINT ( 'NONE',  ( 22.18707434479883744, 5.266624075232406277, 3.077484895491516159 ) ) ;
#23720 = DIRECTION ( 'NONE',  ( 0.000000000000000000, 0.000000000000000000, 1.000000000000000000 ) ) ;
#23721 = CARTESIAN_POINT ( 'NONE',  ( 17.92617638325606677, -3.172788574053346355, 2.962287333578757398 ) ) ;
#23722 = CARTESIAN_POINT ( 'NONE',  ( 81.13619541807486257, 61.97540048441254612, 2.718470589328604081 ) ) ;
#23723 = CARTESIAN_POINT ( 'NONE',  ( -0.01940968312617183042, -32.61825661283325672, 7.678495282201406980 ) ) ;
#23724 = ORIENTED_EDGE ( 'NONE', *, *, #23654, .F. ) ;
#23725 = CARTESIAN_POINT ( 'NONE',  ( 77.86640729734752142, 62.36914183036531512, -3.839379600940508119 ) ) ;
#23726 = AXIS2_PLACEMENT_3D ( 'NONE', #23289, #35859, #4563 ) ;
#23728 = CARTESIAN_POINT ( 'NONE',  ( 14.76731606441705402, -5.163872065058405347, -2.500000000054358740 ) ) ;
#23727 = CARTESIAN_POINT ( 'NONE',  ( 26.06497513181486880, 0.7653527817883817308, 4.421512231569668216 ) ) ;
#23729 = CARTESIAN_POINT ( 'NONE',  ( 81.64588081867499625, 62.19174680642493058, -2.443770662193221810 ) ) ;
#23730 = CARTESIAN_POINT ( 'NONE',  ( 78.90238306073098329, 63.15141027621823611, 3.791687334209852267 ) ) ;
#23731 = FACE_OUTER_BOUND ( 'NONE', #19229, .T. ) ;
#23732 = CIRCLE ( 'NONE', #34301, 0.1000000000000028644 ) ;
#23733 = CARTESIAN_POINT ( 'NONE',  ( 82.52706534919268222, 63.19378067493421014, 1.386429027373558664 ) ) ;
#23735 = ORIENTED_EDGE ( 'NONE', *, *, #8639, .F. ) ;
#23734 = CARTESIAN_POINT ( 'NONE',  ( 39.57450465021913999, -13.08403409140692553, 6.000000000000001776 ) ) ;
#23736 = CARTESIAN_POINT ( 'NONE',  ( 29.64656804624054942, -2.931097914703496787, 5.165983120431130615 ) ) ;
#23737 = DIRECTION ( 'NONE',  ( 0.000000000000000000, 0.000000000000000000, 1.000000000000000000 ) ) ;
#23738 = VERTEX_POINT ( 'NONE', #6590 ) ;
#23739 = FACE_OUTER_BOUND ( 'NONE', #31146, .T. ) ;
#23740 = CARTESIAN_POINT ( 'NONE',  ( 22.60882170720540429, 0.2902834165949863543, -6.504415997128977445 ) ) ;
#23741 = EDGE_CURVE ( 'NONE', #37831, #10017, #20964, .T. ) ;
#23742 = DIRECTION ( 'NONE',  ( 0.6662082868431817850, 0.000000000000000000, -0.7457657263118712132 ) ) ;
#23743 = CYLINDRICAL_SURFACE ( 'NONE', #37418, 0.1000000000000028644 ) ;
#23744 = EDGE_CURVE ( 'NONE', #39470, #9255, #4282, .T. ) ;
#23745 = CARTESIAN_POINT ( 'NONE',  ( -71.91962744173181932, -48.24704961926887847, 9.950992054193424252 ) ) ;
#23746 = CARTESIAN_POINT ( 'NONE',  ( 20.91845615398282376, 4.580162226973405915, -2.658158748952031747 ) ) ;
#23747 = CARTESIAN_POINT ( 'NONE',  ( 3.384522735995777243, -32.62220248850111659, 7.784725160561910329 ) ) ;
#23748 = CARTESIAN_POINT ( 'NONE',  ( -34.24874870218063450, -26.64985754041175525, 6.700000000000000178 ) ) ;
#23749 = CARTESIAN_POINT ( 'NONE',  ( -1.034128943104400067, -31.75451381418163166, 6.865554069792296765 ) ) ;
#23750 = DIRECTION ( 'NONE',  ( 0.000000000000000000, 0.000000000000000000, -1.000000000000000000 ) ) ;
#23751 = CARTESIAN_POINT ( 'NONE',  ( 0.9904113513190105911, -32.89497607571279758, 7.754798119455333705 ) ) ;
#23752 = CARTESIAN_POINT ( 'NONE',  ( 5.094860814950578742, -29.76375618630001796, 6.903372536218460809 ) ) ;
#23753 = ADVANCED_FACE ( 'NONE', ( #39465 ), #36304, .T. ) ;
#23754 = CARTESIAN_POINT ( 'NONE',  ( -10.24874870218063450, -26.64985754041175525, 6.700000000000000178 ) ) ;
#23755 = ADVANCED_FACE ( 'NONE', ( #1425 ), #14667, .T. ) ;
#23756 = VERTEX_POINT ( 'NONE', #4893 ) ;
#23757 = LINE ( 'NONE', #8097, #39631 ) ;
#23758 = CARTESIAN_POINT ( 'NONE',  ( 72.75889805100318597, 61.54370698478811619, -3.677837812371882897 ) ) ;
#23759 = ORIENTED_EDGE ( 'NONE', *, *, #20661, .F. ) ;
#23760 = CARTESIAN_POINT ( 'NONE',  ( 86.27652758060003180, -0.2533697966053802819, -5.917929974479952726 ) ) ;
#23761 = AXIS2_PLACEMENT_3D ( 'NONE', #8661, #24317, #36880 ) ;
#23762 = CARTESIAN_POINT ( 'NONE',  ( 0.1848886247971567864, -26.52637048718725765, 6.969307238440507035 ) ) ;
#23763 = CARTESIAN_POINT ( 'NONE',  ( 2.932249383186227742, -26.40092124923403460, 6.874555630061442102 ) ) ;
#23764 = LINE ( 'NONE', #11599, #19535 ) ;
#23765 = DIRECTION ( 'NONE',  ( -0.9396926207859057634, -0.3420201433256757073, -0.000000000000000000 ) ) ;
#23766 = CARTESIAN_POINT ( 'NONE',  ( -66.99872204295122913, 28.48507918597134037, 9.800414904976365804 ) ) ;
#23767 = ORIENTED_EDGE ( 'NONE', *, *, #37500, .F. ) ;
#23768 = CARTESIAN_POINT ( 'NONE',  ( 79.28407881342867825, 64.35615987108394620, -3.584461231902843714 ) ) ;
#23769 = CARTESIAN_POINT ( 'NONE',  ( 79.69769351933607027, 63.91149418591603393, 3.725738571856552994 ) ) ;
#23770 = DIRECTION ( 'NONE',  ( 0.000000000000000000, 0.7126435865141299564, -0.7015262779114391778 ) ) ;
#23771 = DIRECTION ( 'NONE',  ( 1.000000000000000000, 0.000000000000000000, -0.000000000000000000 ) ) ;
#23772 = SHAPE_REPRESENTATION ( 'Ruler Clamping Screw', ( #30744 ), #18883 ) ;
#23773 = CARTESIAN_POINT ( 'NONE',  ( 4.009398355169389028, -27.07422402788343518, 6.876076431790005827 ) ) ;
#23774 = DIRECTION ( 'NONE',  ( -0.3420201433256601642, -0.9396926207859115365, -0.000000000000000000 ) ) ;
#23775 = CARTESIAN_POINT ( 'NONE',  ( 21.85643539959775694, 2.564233178479530917, 15.28924334870111146 ) ) ;
#23776 = VERTEX_POINT ( 'NONE', #11455 ) ;
#23777 = FACE_OUTER_BOUND ( 'NONE', #13062, .T. ) ;
#23778 = CARTESIAN_POINT ( 'NONE',  ( 14.77571469133521198, -5.163876921041897106, 2.500000000713546555 ) ) ;
#23779 = CIRCLE ( 'NONE', #6714, 7.538952224936807056 ) ;
#23780 = CARTESIAN_POINT ( 'NONE',  ( -80.18326513131566458, 10.47830472520926826, -6.103113075884769145 ) ) ;
#23781 = CYLINDRICAL_SURFACE ( 'NONE', #17522, 0.1000000000000028644 ) ;
#23782 = DIRECTION ( 'NONE',  ( 1.000000000000000000, 0.000000000000000000, 0.000000000000000000 ) ) ;
#23783 = CARTESIAN_POINT ( 'NONE',  ( 79.05590852586873041, 65.97304283769160804, 2.079311677127754887 ) ) ;
#23784 = CARTESIAN_POINT ( 'NONE',  ( -1.490154220801371387, -30.74486085573374083, 7.756377446753165650 ) ) ;
#23785 = B_SPLINE_CURVE_WITH_KNOTS ( 'NONE', 3,
 ( #6417, #30728, #25146, #37679, #18757, #14844, #9482, #15057, #2946, #24739, #37288, #18543, #2533, #34030, #9280, #2322, #8872, #40569, #40172, #2737, #34433, #22072, #34643, #36885, #28023, #27811, #40364, #27410, #39973, #18971, #12167, #8665, #11743, #24322, #9081, #6008, #12380, #21244, #33816, #21858, #31128, #31332, #3156, #37893, #35045, #11038, #9701, #26513, #38852, #25354, #12991, #32898, #4498, #23615, #23223, #20314, #36181, #39247, #10645, #35787, #7564, #451, #7765, #31947, #20119, #39043 ),
 .UNSPECIFIED., .F., .F.,
 ( 4, 2, 2, 2, 2, 2, 2, 2, 2, 2, 2, 2, 2, 2, 2, 2, 2, 2, 2, 2, 2, 2, 2, 2, 2, 2, 2, 2, 2, 2, 2, 2, 4 ),
 ( 0.04111556421994554816, 0.04237963096789508499, 0.04364369771584461488, 0.04490776446379415171, 0.04617183121174368160, 0.04869996470764277607, 0.04996403145559230596, 0.05122809820354183585, 0.05249216495149136574, 0.05375623169944089563, 0.05502029844739042552, 0.05628436519533996235, 0.05881249869123900131, 0.06007656543918852426, 0.06134063218713804722, 0.06260469893508756323, 0.06386876568303709312, 0.06513283243098660913, 0.06639689917893612514, 0.06766096592688564115, 0.06829299930086041304, 0.06892503267483519880, 0.07018909942278475644, 0.07082113279675951445, 0.07145316617073427246, 0.07271723291868376071, 0.07398129966663326285, 0.07524536641458275110, 0.07650943316253225324, 0.07777349991048174149, 0.07903756665843122975, 0.08030163340638071801, 0.08156570015433022014 ),
 .UNSPECIFIED. ) ;
#23786 = DIRECTION ( 'NONE',  ( 0.1736481776669404897, -0.9848077530122062440, -0.000000000000000000 ) ) ;
#23787 = CARTESIAN_POINT ( 'NONE',  ( -1.390358791352311885, -31.21210439690994320, 7.753200566781599967 ) ) ;
#23788 = CARTESIAN_POINT ( 'NONE',  ( 0.6707251200944375213, -26.22480883340364954, 6.903112506833889661 ) ) ;
#23789 = EDGE_CURVE ( 'NONE', #7409, #31349, #40562, .T. ) ;
#23790 = EDGE_CURVE ( 'NONE', #31323, #22687, #36596, .T. ) ;
#23791 = DIRECTION ( 'NONE',  ( 0.000000000000000000, 0.000000000000000000, 1.000000000000000000 ) ) ;
#23792 = CARTESIAN_POINT ( 'NONE',  ( 87.77108079546424335, -0.2309192195606523390, 3.753057804081372684 ) ) ;
#23793 = EDGE_CURVE ( 'NONE', #1128, #12118, #6173, .T. ) ;
#23794 = CARTESIAN_POINT ( 'NONE',  ( -24.34874870218063592, -25.49307895267003587, 6.700000000000000178 ) ) ;
#23795 = CARTESIAN_POINT ( 'NONE',  ( 67.81915466200213416, 58.05084569011909679, 3.988165415173097195 ) ) ;
#23796 = CARTESIAN_POINT ( 'NONE',  ( 35.47949778313863334, -1.848513373575088714, 5.743831722591982825 ) ) ;
#23797 = CARTESIAN_POINT ( 'NONE',  ( -32.44874870218063734, -26.64985754041175525, 6.800000000000000711 ) ) ;
#23798 = CARTESIAN_POINT ( 'NONE',  ( 85.12050554930138446, 2.746332700819607453, -1.966258668667607123 ) ) ;
#23800 = CARTESIAN_POINT ( 'NONE',  ( 4.869399027392470103, -30.80178947334650275, 6.874555630061443878 ) ) ;
#23799 = CARTESIAN_POINT ( 'NONE',  ( 81.21856020378540109, 61.45841878490982424, -1.842213953838253815 ) ) ;
#23801 = CARTESIAN_POINT ( 'NONE',  ( -1.611808805343041051, -28.80220400497604416, 6.887945620086120435 ) ) ;
#23802 = CARTESIAN_POINT ( 'NONE',  ( -57.68674048389794962, 29.08812126441108603, 4.503248736989442058 ) ) ;
#23803 = CARTESIAN_POINT ( 'NONE',  ( -0.6586047051253564044, -32.15549463652887852, 6.875780273367531059 ) ) ;
#23804 = ORIENTED_EDGE ( 'NONE', *, *, #23663, .F. ) ;
#23805 = CARTESIAN_POINT ( 'NONE',  ( -1.722317759908783996, -28.83844474126830804, 7.750000000000000888 ) ) ;
#23806 = PRODUCT_DEFINITION_CONTEXT ( 'detailed design', #1357, 'design' ) ;
#23807 = CARTESIAN_POINT ( 'NONE',  ( 81.03586710326727882, 61.41218721227320287, -1.994058748902159950 ) ) ;
#23808 = CARTESIAN_POINT ( 'NONE',  ( -1.521248034093554136, -28.20206769887411724, 6.916197352289367828 ) ) ;
#23809 = CARTESIAN_POINT ( 'NONE',  ( 78.72772338417267690, 65.90741647005506820, 1.973779052375973064 ) ) ;
#23810 = CARTESIAN_POINT ( 'NONE',  ( 26.22005767131799914, 1.338533239893550109, 4.347865427178345676 ) ) ;
#23813 = ORIENTED_EDGE ( 'NONE', *, *, #31306, .T. ) ;
#23812 = CARTESIAN_POINT ( 'NONE',  ( -0.7638942222524777170, -27.22743084971469330, 6.949473656533219135 ) ) ;
#23811 = AXIS2_PLACEMENT_3D ( 'NONE', #27415, #20619, #33206 ) ;
#23814 = CARTESIAN_POINT ( 'NONE',  ( 75.58356882164667923, 59.79721036961944236, -3.404024988867352164 ) ) ;
#23815 = CARTESIAN_POINT ( 'NONE',  ( -69.92837670882107659, -20.78299143688747819, 5.916079783099621459 ) ) ;
#23817 = DIRECTION ( 'NONE',  ( -0.000000000000000000, -0.000000000000000000, 1.000000000000000000 ) ) ;
#23816 = CARTESIAN_POINT ( 'NONE',  ( 82.38753728249152175, 5.816132372599501110, 5.999999999999998224 ) ) ;
#23818 = CARTESIAN_POINT ( 'NONE',  ( -1.182416063321688693, -27.76731179479478229, 7.757178535559532406 ) ) ;
#23819 = DIRECTION ( 'NONE',  ( 0.000000000000000000, 0.000000000000000000, 1.000000000000000000 ) ) ;
#23820 =( BOUNDED_SURFACE ( )  B_SPLINE_SURFACE ( 3, 2, ( 
 ( #12270, #24843, #37785 ),
 ( #9593, #37389, #19070 ),
 ( #9183, #21756, #34744 ),
 ( #3256, #15778, #34338 ) ),
 .UNSPECIFIED., .F., .F., .T. ) 
 B_SPLINE_SURFACE_WITH_KNOTS ( ( 4, 4 ),
 ( 3, 3 ),
 ( 0.005269474087521970260, 0.007542904871472735570 ),
 ( 0.000000000000000000, 1.000000000000000000 ),
 .UNSPECIFIED. ) 
 GEOMETRIC_REPRESENTATION_ITEM ( )  RATIONAL_B_SPLINE_SURFACE ( (
 ( 1.000000000000000000, 0.8929779998654624462, 1.000000000000000000),
 ( 1.000000000000000000, 0.8751601137609862358, 1.000000000000000000),
 ( 1.000000000000000000, 0.8609322455899910409, 1.000000000000000000),
 ( 1.000000000000000000, 0.8503447817689703259, 1.000000000000000000) ) ) 
 REPRESENTATION_ITEM ( '' )  SURFACE ( )  );
#23821 = CARTESIAN_POINT ( 'NONE',  ( 21.82801474315459345, 4.845872665800435186, -3.845916247992467785 ) ) ;
#23822 = VERTEX_POINT ( 'NONE', #1829 ) ;
#23823 = CARTESIAN_POINT ( 'NONE',  ( -1.797258899342013549, -29.44812577374269580, 7.754798119455333705 ) ) ;
#23824 = ORIENTED_EDGE ( 'NONE', *, *, #17451, .F. ) ;
#23825 = CARTESIAN_POINT ( 'NONE',  ( 22.71016324673079012, -4.497379315063210647, 7.328459856909534054 ) ) ;
#23826 = CARTESIAN_POINT ( 'NONE',  ( 3.021324086407803478, -24.55319635012989110, 6.700000000000000178 ) ) ;
#23827 = DIRECTION ( 'NONE',  ( 0.000000000000000000, -0.000000000000000000, -1.000000000000000000 ) ) ;
#23828 = CARTESIAN_POINT ( 'NONE',  ( 79.18807306865346618, 66.05665914930217752, 1.983726836936665183 ) ) ;
#23829 = CARTESIAN_POINT ( 'NONE',  ( 85.98118993947397826, 1.447477879098551856, 5.565446759936045318 ) ) ;
#23830 = CARTESIAN_POINT ( 'NONE',  ( 4.296241352401964697, -27.37412594797728715, 7.635761828346577573 ) ) ;
#23831 = ORIENTED_EDGE ( 'NONE', *, *, #33873, .T. ) ;
#23832 = DIRECTION ( 'NONE',  ( 1.000000000000000000, -0.000000000000000000, 0.000000000000000000 ) ) ;
#23833 = AXIS2_PLACEMENT_3D ( 'NONE', #36955, #1985, #23771 ) ;
#23834 = CARTESIAN_POINT ( 'NONE',  ( 5.063683507119011828, -29.07157929038318755, 6.866852738645444099 ) ) ;
#23835 = CARTESIAN_POINT ( 'NONE',  ( 18.24666052293414253, -3.095731080093750087, -3.016724835387484482 ) ) ;
#23836 = EDGE_CURVE ( 'NONE', #38454, #26819, #23628, .T. ) ;
#23837 = CARTESIAN_POINT ( 'NONE',  ( 36.99184966288904519, -2.719776486114577008, -5.979870809795490239 ) ) ;
#23838 = CARTESIAN_POINT ( 'NONE',  ( -70.92837670882107659, -56.35932253828835314, 0.000000000000000000 ) ) ;
#23839 = CARTESIAN_POINT ( 'NONE',  ( 24.67432665942473236, 0.7056974025990818689, -4.794247048528192501 ) ) ;
#23840 = FACE_OUTER_BOUND ( 'NONE', #16171, .T. ) ;
#23841 = VERTEX_POINT ( 'NONE', #20526 ) ;
#23842 = DIRECTION ( 'NONE',  ( 0.9396926207859080948, 0.3420201433256694901, -0.000000000000000000 ) ) ;
#23843 = VECTOR ( 'NONE', #36396, 1000.000000000000000 ) ;
#23844 = CARTESIAN_POINT ( 'NONE',  ( -1.137290665474521401, -27.69707997270900179, 6.988553391373223178 ) ) ;
#23845 = ORIENTED_EDGE ( 'NONE', *, *, #30942, .F. ) ;
#23846 = ORIENTED_EDGE ( 'NONE', *, *, #24370, .F. ) ;
#23847 = CARTESIAN_POINT ( 'NONE',  ( 33.94687777511632021, -0.4864967322304499797, 5.119561820975840227 ) ) ;
#23848 = CARTESIAN_POINT ( 'NONE',  ( -1.649386784634844894, -30.58432408495164623, 6.961115707816236231 ) ) ;
#23849 = CARTESIAN_POINT ( 'NONE',  ( 17.88642430224130209, -3.177481357815599594, -2.956548120854927575 ) ) ;
#23850 = CARTESIAN_POINT ( 'NONE',  ( -18.44874870218064089, -26.64985754041175525, 6.700000000000000178 ) ) ;
#23851 = ORIENTED_EDGE ( 'NONE', *, *, #15119, .T. ) ;
#23852 = DIRECTION ( 'NONE',  ( 1.000000000000000000, 0.000000000000000000, 0.000000000000000000 ) ) ;
#23853 = ORIENTED_EDGE ( 'NONE', *, *, #28785, .F. ) ;
#23854 = ORIENTED_EDGE ( 'NONE', *, *, #4806, .T. ) ;
#23855 = DIRECTION ( 'NONE',  ( 1.000000000000000000, 0.000000000000000000, 0.000000000000000000 ) ) ;
#23856 = VERTEX_POINT ( 'NONE', #11251 ) ;
#23857 = CARTESIAN_POINT ( 'NONE',  ( -58.12241481891157946, 28.59128022406728675, -4.921134609696957263 ) ) ;
#23858 = ORIENTED_EDGE ( 'NONE', *, *, #17743, .T. ) ;
#23859 = EDGE_CURVE ( 'NONE', #37103, #4455, #17423, .T. ) ;
#23861 = CARTESIAN_POINT ( 'NONE',  ( -14.44874870218064089, -26.64985754041175525, 6.700000000000000178 ) ) ;
#23860 = CARTESIAN_POINT ( 'NONE',  ( 4.818431413503324379, -27.98001418187951472, 6.912143950357346078 ) ) ;
#23862 = CARTESIAN_POINT ( 'NONE',  ( 23.41947422422738967, 3.389483684519994711, 3.647767087863493796 ) ) ;
#23863 = CARTESIAN_POINT ( 'NONE',  ( 78.94658775073214940, 66.18447242754096749, -1.227604746834844107 ) ) ;
#23864 = CARTESIAN_POINT ( 'NONE',  ( 0.3299799762144463022, -25.47407434293985418, 6.894806418505347700 ) ) ;
#23865 = CYLINDRICAL_SURFACE ( 'NONE', #293, 3.399999999999999911 ) ;
#23866 = ORIENTED_EDGE ( 'NONE', *, *, #30982, .F. ) ;
#23868 = CARTESIAN_POINT ( 'NONE',  ( 18.13303797671674644, -2.853770859205107868, -3.036497144084084443 ) ) ;
#23867 = FACE_OUTER_BOUND ( 'NONE', #3759, .T. ) ;
#23869 = CARTESIAN_POINT ( 'NONE',  ( -1.799174846253356552, -29.51474654163957112, 6.875671892026061549 ) ) ;
#23870 = CARTESIAN_POINT ( 'NONE',  ( 74.45643886899652841, 62.27924959144220196, 3.661998389317300706 ) ) ;
#23871 = AXIS2_PLACEMENT_3D ( 'NONE', #40019, #5856, #34287 ) ;
#23872 = CARTESIAN_POINT ( 'NONE',  ( 21.85601462913819049, 3.177268030137100130, -4.957676561649461355 ) ) ;
#23873 = VERTEX_POINT ( 'NONE', #7973 ) ;
#23874 = CARTESIAN_POINT ( 'NONE',  ( -62.99925096543677938, 37.98736139490962671, 4.069933184287122252 ) ) ;
#23875 = ADVANCED_FACE ( 'NONE', ( #33111 ), #30010, .F. ) ;
#23876 = CARTESIAN_POINT ( 'NONE',  ( 9.703489126596464232, 56.50623631086179444, 1.000000000000000000 ) ) ;
#23877 = DIRECTION ( 'NONE',  ( -0.000000000000000000, -0.000000000000000000, 1.000000000000000000 ) ) ;
#23878 = CARTESIAN_POINT ( 'NONE',  ( -1.261910041069868260, -27.90116479715461750, 7.695279973900954751 ) ) ;
#23879 = CARTESIAN_POINT ( 'NONE',  ( -67.57960606288301619, 36.15173574121458699, 8.626892781888731321 ) ) ;
#23880 = CARTESIAN_POINT ( 'NONE',  ( 78.68815740766761735, 66.05701152551952759, 1.050153991572632561 ) ) ;
#23881 = CARTESIAN_POINT ( 'NONE',  ( 87.00024757794628272, 0.6349172363070331171, 4.931108601852515427 ) ) ;
#23882 = B_SPLINE_CURVE_WITH_KNOTS ( 'NONE', 3,
 ( #12873, #2820, #8748, #21333, #34119, #15761, #28316, #37771, #40445, #12254, #15344, #24826, #18626, #3036, #21741, #6093, #12665, #25240, #16963, #13478, #28730, #19258 ),
 .UNSPECIFIED., .F., .F.,
 ( 4, 1, 1, 1, 1, 1, 1, 2, 2, 2, 1, 1, 2, 2, 4 ),
 ( 0.000000000000000000, 0.2500000000000843214, 0.3750000000001239009, 0.4375000000001435518, 0.4687500000001555422, 0.4843750000001613154, 0.4921875000001640355, 0.4960937500001632583, 0.5000000000001625367, 0.6250000000001404432, 0.6875000000001272316, 0.7187500000001187939, 0.7343750000001144640, 0.7500000000001101341, 1.000000000000000000 ),
 .UNSPECIFIED. ) ;
#23883 = CARTESIAN_POINT ( 'NONE',  ( 30.36459403182758265, -1.672762201151555939, 6.017704416797944766 ) ) ;
#23884 = CARTESIAN_POINT ( 'NONE',  ( -1.799609906766908685, -29.56993018339339940, 7.202408869016148074 ) ) ;
#23885 = DIRECTION ( 'NONE',  ( -0.1736481776669340227, 0.9848077530122073542, -0.000000000000000000 ) ) ;
#23886 = CYLINDRICAL_SURFACE ( 'NONE', #27064, 0.1000000000000028644 ) ;
#23887 = AXIS2_PLACEMENT_3D ( 'NONE', #29930, #1747, #14278 ) ;
#23888 = CARTESIAN_POINT ( 'NONE',  ( -8.448748702180639114, -26.64985754041175525, 6.700000000000000178 ) ) ;
#23889 = EDGE_CURVE ( 'NONE', #40280, #35786, #21575, .T. ) ;
#23890 = CARTESIAN_POINT ( 'NONE',  ( 37.01039123596240898, -2.703883751567390359, -5.982764670703224041 ) ) ;
#23891 = CARTESIAN_POINT ( 'NONE',  ( -0.3385372945680173995, -26.84912605459717838, 7.013842709614101167 ) ) ;
#23892 = CARTESIAN_POINT ( 'NONE',  ( -70.92837670882012446, 0.2170085631207802901, 6.000000000001379341 ) ) ;
#23893 = DIRECTION ( 'NONE',  ( 0.000000000000000000, -1.000000000000000000, -0.000000000000000000 ) ) ;
#23894 = CARTESIAN_POINT ( 'NONE',  ( 0.05705130999228511662, -26.47997509747052192, 7.754798119455333705 ) ) ;
#23895 = VECTOR ( 'NONE', #26726, 1000.000000000000000 ) ;
#23896 = CARTESIAN_POINT ( 'NONE',  ( -2.448748702180640446, -25.49307895267003587, 6.800000000000000711 ) ) ;
#23897 = ORIENTED_EDGE ( 'NONE', *, *, #27186, .F. ) ;
#23898 = CARTESIAN_POINT ( 'NONE',  ( 33.45095132737965571, -3.771342036780488627, 5.158305224127381017 ) ) ;
#23899 =( BOUNDED_CURVE ( )  B_SPLINE_CURVE ( 3, ( #8411, #25704, #34386, #401 ),
 .UNSPECIFIED., .F., .T. ) 
 B_SPLINE_CURVE_WITH_KNOTS ( ( 4, 4 ),
 ( 1.347909859412855127, 1.534781240595300078 ),
 .UNSPECIFIED. ) 
 CURVE ( )  GEOMETRIC_REPRESENTATION_ITEM ( )  RATIONAL_B_SPLINE_CURVE ( ( 1.000000000000000000, 0.9970920404276226723, 0.9970920404276226723, 1.000000000000000000 ) ) 
 REPRESENTATION_ITEM ( '' )  );
#23900 = DIRECTION ( 'NONE',  ( -0.000000000000000000, -0.000000000000000000, -1.000000000000000000 ) ) ;
#23901 = CARTESIAN_POINT ( 'NONE',  ( 66.85741207324237223, 57.95599960577073517, -3.999594749380519954 ) ) ;
#23902 = ADVANCED_FACE ( 'NONE', ( #8991 ), #24650, .T. ) ;
#23903 = CARTESIAN_POINT ( 'NONE',  ( -2.628262761802994785, -27.02926189858848360, 7.695279973900954751 ) ) ;
#23904 = VERTEX_POINT ( 'NONE', #18048 ) ;
#23905 = DIRECTION ( 'NONE',  ( -0.000000000000000000, -0.000000000000000000, -1.000000000000000000 ) ) ;
#23906 = FACE_OUTER_BOUND ( 'NONE', #14591, .T. ) ;
#23907 = LINE ( 'NONE', #8253, #23981 ) ;
#23908 = CARTESIAN_POINT ( 'NONE',  ( -80.69880588614331884, 11.48364438412461119, 2.288095856349301016 ) ) ;
#23909 = CARTESIAN_POINT ( 'NONE',  ( 0.3268026257083770925, -32.78913155470570473, 6.974994249511788702 ) ) ;
#23910 = DIRECTION ( 'NONE',  ( -0.000000000000000000, -0.000000000000000000, 1.000000000000000000 ) ) ;
#23911 = ORIENTED_EDGE ( 'NONE', *, *, #35633, .T. ) ;
#23912 = CARTESIAN_POINT ( 'NONE',  ( 23.43164679671629003, 3.783403669430692062, 3.128883362209908814 ) ) ;
#23913 = CARTESIAN_POINT ( 'NONE',  ( 80.03496335128151884, 66.36160760684386162, -1.085061034363233201 ) ) ;
#23915 = AXIS2_PLACEMENT_3D ( 'NONE', #21144, #5490, #11643 ) ;
#23914 = CARTESIAN_POINT ( 'NONE',  ( 80.68504733838216225, 63.31860838049915685, 3.572022490087450652 ) ) ;
#23916 = VECTOR ( 'NONE', #30268, 999.9999999999998863 ) ;
#23917 = CARTESIAN_POINT ( 'NONE',  ( -0.07973430863924736711, -32.46669619298256748, 6.866852738645443210 ) ) ;
#23918 = VERTEX_POINT ( 'NONE', #8780 ) ;
#23919 = CARTESIAN_POINT ( 'NONE',  ( 77.45101235711661047, 65.18271368322074011, -2.178915381671167939 ) ) ;
#23921 = CARTESIAN_POINT ( 'NONE',  ( 14.75560021692665202, -5.144521063667438554, -2.500000000017701840 ) ) ;
#23920 = CARTESIAN_POINT ( 'NONE',  ( 23.58768437045748101, 0.4155699572297044120, 5.528158402111618130 ) ) ;
#23922 = ADVANCED_FACE ( 'NONE', ( #27534 ), #40283, .F. ) ;
#23923 = EDGE_CURVE ( 'NONE', #16534, #17047, #16511, .T. ) ;
#23924 = CARTESIAN_POINT ( 'NONE',  ( 79.33055955479225929, 65.97011375961784552, -2.296576099416863581 ) ) ;
#23925 = CARTESIAN_POINT ( 'NONE',  ( 78.85022303194003257, 62.54057813906807439, 3.766285651913947596 ) ) ;
#23926 = ORIENTED_EDGE ( 'NONE', *, *, #35718, .T. ) ;
#23927 = EDGE_CURVE ( 'NONE', #14639, #9920, #24862, .T. ) ;
#23928 = AXIS2_PLACEMENT_3D ( 'NONE', #13848, #7869, #11340 ) ;
#23929 = CARTESIAN_POINT ( 'NONE',  ( 36.60794128011109905, -3.504051565419862069, -5.830873203126740734 ) ) ;
#23930 = CARTESIAN_POINT ( 'NONE',  ( 79.66449323073867106, 66.32230831612973532, 1.250177805244208296 ) ) ;
#23932 = CARTESIAN_POINT ( 'NONE',  ( 36.10284116201629701, 0.9159659085930716982, 5.999999999999999112 ) ) ;
#23931 = CARTESIAN_POINT ( 'NONE',  ( 3.434919991761703262, -26.64563530151581361, 7.784838882742140420 ) ) ;
#23933 = CARTESIAN_POINT ( 'NONE',  ( 23.98959816390508593, 3.209834647534565377, 4.521976212143768770 ) ) ;
#23934 = DIRECTION ( 'NONE',  ( 0.000000000000000000, 0.000000000000000000, 1.000000000000000000 ) ) ;
#23935 = CARTESIAN_POINT ( 'NONE',  ( -10.97867591359219475, -24.55319635012989110, 6.700000000000000178 ) ) ;
#23936 = ORIENTED_EDGE ( 'NONE', *, *, #3719, .T. ) ;
#23937 = CARTESIAN_POINT ( 'NONE',  ( -80.91065676098011750, -6.597313057213483489, -0.5950503846463429669 ) ) ;
#23938 = CARTESIAN_POINT ( 'NONE',  ( 22.28822635994833945, 0.2533368339982051132, -7.122398813026761033 ) ) ;
#23939 = CARTESIAN_POINT ( 'NONE',  ( 0.3635682928745467835, -32.69609516209911959, 7.013842709614101167 ) ) ;
#23940 = CARTESIAN_POINT ( 'NONE',  ( 5.001438667734867671, -30.73314912614656436, 7.695279973900954751 ) ) ;
#23941 = DIRECTION ( 'NONE',  ( -1.000000000000000000, -1.734723475976808672E-15, 0.000000000000000000 ) ) ;
#23942 = DIRECTION ( 'NONE',  ( -0.000000000000000000, -1.000000000000000000, -0.000000000000000000 ) ) ;
#23943 = CARTESIAN_POINT ( 'NONE',  ( 33.45628508796660583, -3.829382271890817258, -5.093793554038391846 ) ) ;
#23944 = CARTESIAN_POINT ( 'NONE',  ( 30.80878225244670077, -3.348914835482470043, -4.960346515808566892 ) ) ;
#23945 = DIRECTION ( 'NONE',  ( -0.000000000000000000, -0.000000000000000000, 1.000000000000000000 ) ) ;
#23946 = CARTESIAN_POINT ( 'NONE',  ( -71.92070561156705821, -48.24608967860918085, 5.917785064630586511 ) ) ;
#23947 = CARTESIAN_POINT ( 'NONE',  ( 2.674062101369763855, -32.82753328145249583, 6.997764925645181933 ) ) ;
#23948 = CARTESIAN_POINT ( 'NONE',  ( -73.08797875314412806, 4.425365387401466677, 10.93635685748529873 ) ) ;
#23949 = VECTOR ( 'NONE', #35890, 1000.000000000000000 ) ;
#23950 = FACE_OUTER_BOUND ( 'NONE', #16936, .T. ) ;
#23951 = CARTESIAN_POINT ( 'NONE',  ( 66.58353442343859285, 57.79581178809598896, 3.999616584010542208 ) ) ;
#23952 = CARTESIAN_POINT ( 'NONE',  ( 71.26393988290669768, 58.68354208002635630, -3.837797619696095008 ) ) ;
#23953 = EDGE_CURVE ( 'NONE', #8120, #34664, #2421, .T. ) ;
#23954 = ORIENTED_EDGE ( 'NONE', *, *, #33061, .T. ) ;
#23955 = CARTESIAN_POINT ( 'NONE',  ( 1.700390093233090871, -29.56993018339339940, 7.800000000000000711 ) ) ;
#23956 = CARTESIAN_POINT ( 'NONE',  ( 0.1799856441161017395, -26.52881562477996980, 6.920489980334477487 ) ) ;
#23957 = FACE_OUTER_BOUND ( 'NONE', #13983, .T. ) ;
#23958 = CARTESIAN_POINT ( 'NONE',  ( 21.71185578408363881, 6.328645931448866335, 3.192210964217056191 ) ) ;
#23959 = CARTESIAN_POINT ( 'NONE',  ( -71.92837670882107659, 28.72470171467712063, 3.916079783099620126 ) ) ;
#23960 = CONTEXT_DEPENDENT_SHAPE_REPRESENTATION ( #2684, #14733 ) ;
#23961 = ADVANCED_FACE ( 'NONE', ( #26663 ), #24378, .F. ) ;
#23962 = DIRECTION ( 'NONE',  ( -0.000000000000000000, -0.000000000000000000, -1.000000000000000000 ) ) ;
#23963 = VERTEX_POINT ( 'NONE', #7916 ) ;
#23964 = CARTESIAN_POINT ( 'NONE',  ( 4.638101942922436827, -27.85824998890764448, 7.635761828346577573 ) ) ;
#23965 = PRESENTATION_STYLE_ASSIGNMENT (( #8727 ) ) ;
#23966 = EDGE_CURVE ( 'NONE', #13498, #5492, #14901, .T. ) ;
#23967 = ORIENTED_EDGE ( 'NONE', *, *, #33061, .F. ) ;
#23968 = CARTESIAN_POINT ( 'NONE',  ( 78.69113869042872977, 65.45098002628645872, -2.699019001080980473 ) ) ;
#23969 = CARTESIAN_POINT ( 'NONE',  ( 17.36540201846515075, 9.558839302759881917, -2.500000000000007105 ) ) ;
#23970 = CARTESIAN_POINT ( 'NONE',  ( 80.24949846641645479, 62.81397012663808255, 3.564905221331804430 ) ) ;
#23971 = EDGE_CURVE ( 'NONE', #30400, #39064, #27469, .T. ) ;
#23972 = AXIS2_PLACEMENT_3D ( 'NONE', #20541, #14366, #26934 ) ;
#23973 = LINE ( 'NONE', #33062, #15304 ) ;
#23974 = AXIS2_PLACEMENT_3D ( 'NONE', #2777, #15303, #40406 ) ;
#23975 = CARTESIAN_POINT ( 'NONE',  ( 4.015454011556017555, -27.07985406927975447, 6.882085323592685988 ) ) ;
#23977 = ORIENTED_EDGE ( 'NONE', *, *, #5038, .T. ) ;
#23976 = CARTESIAN_POINT ( 'NONE',  ( -6.448748702180637338, -25.49307895267003587, 6.700000000000000178 ) ) ;
#23978 = CARTESIAN_POINT ( 'NONE',  ( 21.85643539959779957, 3.623429283794106670, 13.13803316603621241 ) ) ;
#23979 = VERTEX_POINT ( 'NONE', #36532 ) ;
#23980 = CARTESIAN_POINT ( 'NONE',  ( -78.36455021024127632, 10.14388467517119707, 6.697453011245038113 ) ) ;
#23981 = VECTOR ( 'NONE', #5191, 1000.000000000000000 ) ;
#23982 = CARTESIAN_POINT ( 'NONE',  ( 14.73442315498073540, -4.754054855475527752, 2.504681350756293945 ) ) ;
#23983 = CARTESIAN_POINT ( 'NONE',  ( -78.60820997296055168, 10.22189545475253070, -6.417293082551506878 ) ) ;
#23984 = EDGE_CURVE ( 'NONE', #33558, #26758, #17777, .T. ) ;
#23985 = FACE_OUTER_BOUND ( 'NONE', #15932, .T. ) ;
#23986 = FACE_OUTER_BOUND ( 'NONE', #40290, .T. ) ;
#23987 = DIRECTION ( 'NONE',  ( 0.000000000000000000, 0.000000000000000000, 1.000000000000000000 ) ) ;
#23988 = CARTESIAN_POINT ( 'NONE',  ( 14.61588355500315828, 13.14117221797890345, 2.487560133874544999 ) ) ;
#23989 = CARTESIAN_POINT ( 'NONE',  ( -3.078675913592197944, -24.55319635012989110, 6.700000000000000178 ) ) ;
#23990 = CARTESIAN_POINT ( 'NONE',  ( 0.5638177912361027611, -26.25960026125660818, 6.870737987065013819 ) ) ;
#23991 = CARTESIAN_POINT ( 'NONE',  ( 4.478136214281437155, -27.44056150411416795, 6.880828092187099010 ) ) ;
#23992 = CARTESIAN_POINT ( 'NONE',  ( -12.24874870218063627, -26.64985754041175525, 6.700000000000000178 ) ) ;
#23993 = CARTESIAN_POINT ( 'NONE',  ( 4.184975392578208719, -31.89090000634120514, 6.887945620086122211 ) ) ;
#23994 = EDGE_LOOP ( 'NONE', ( #10791, #24968, #25466, #31033 ) ) ;
#23995 = CARTESIAN_POINT ( 'NONE',  ( 0.3012221886605330745, -26.46337503191243457, 7.505001789837628223 ) ) ;
#23996 = CARTESIAN_POINT ( 'NONE',  ( 67.43935760634008147, 58.17964655298460741, 3.998402061830689025 ) ) ;
#23997 = CARTESIAN_POINT ( 'NONE',  ( 36.99148392659544271, -2.973123077218505106, 5.979813727801484013 ) ) ;
#23998 = FACE_OUTER_BOUND ( 'NONE', #40319, .T. ) ;
#23999 = AXIS2_PLACEMENT_3D ( 'NONE', #26124, #32709, #26518 ) ;
#24000 = CARTESIAN_POINT ( 'NONE',  ( 88.02721697999687933, -0.6980542412123691420, -4.669518943469966210 ) ) ;
#24002 = DIRECTION ( 'NONE',  ( -0.3757233601570978965, -0.9267318687906764829, 0.000000000000000000 ) ) ;
#24001 = CARTESIAN_POINT ( 'NONE',  ( 30.30396332325029718, -0.06004591992995000210, 5.542382567169830132 ) ) ;
#24003 = CARTESIAN_POINT ( 'NONE',  ( -1.615458968787878868, -28.81812344876338017, 6.876076431790006716 ) ) ;
#24004 = CARTESIAN_POINT ( 'NONE',  ( -58.69259491913187787, 29.82092612118092489, 5.479210374447095688 ) ) ;
#24005 = VECTOR ( 'NONE', #4076, 1000.000000000000000 ) ;
#24006 = CARTESIAN_POINT ( 'NONE',  ( -61.24591834330252027, -42.37473357531882812, 2.500000000000000000 ) ) ;
#24007 = ORIENTED_EDGE ( 'NONE', *, *, #13901, .T. ) ;
#24008 = CARTESIAN_POINT ( 'NONE',  ( -69.93073207689441517, -20.86216845902604078, 5.928523475362944772 ) ) ;
#24009 = ORIENTED_EDGE ( 'NONE', *, *, #39824, .T. ) ;
#24010 = ORIENTED_EDGE ( 'NONE', *, *, #27522, .F. ) ;
#24011 = CARTESIAN_POINT ( 'NONE',  ( 80.06960825067233145, 63.75365790317245995, -3.697630003121159969 ) ) ;
#24012 = SHAPE_REPRESENTATION ( 'MAS-318', ( #11650, #1818, #1184, #16926, #39950, #15617, #22224, #24168, #544, #17562, #40587, #6433 ), #4468 ) ;
#24013 = CARTESIAN_POINT ( 'NONE',  ( -1.564531365849052946, -28.30882517984442615, 6.869132338375688818 ) ) ;
#24014 = CARTESIAN_POINT ( 'NONE',  ( 81.04529349509155622, 61.25860024526325276, 1.340350474428757099 ) ) ;
#24015 = CARTESIAN_POINT ( 'NONE',  ( 21.74703536819586347, 0.5577694647882641688, 8.300425383226157194 ) ) ;
#24017 = ORIENTED_EDGE ( 'NONE', *, *, #22531, .F. ) ;
#24016 = CARTESIAN_POINT ( 'NONE',  ( 3.137425909638337895, -33.65403811543650647, 6.954324564059724878 ) ) ;
#24018 = ADVANCED_FACE ( 'NONE', ( #29739 ), #10991, .F. ) ;
#24019 = ADVANCED_FACE ( 'NONE', ( #1554 ), #17171, .F. ) ;
#24020 = CARTESIAN_POINT ( 'NONE',  ( 73.39456880541679595, 61.63402075718063600, -3.749455561531862546 ) ) ;
#24022 = EDGE_CURVE ( 'NONE', #16945, #7860, #17960, .T. ) ;
#24021 = CARTESIAN_POINT ( 'NONE',  ( 3.272872476393454910, -32.58444492952590110, 6.868387053540521592 ) ) ;
#24024 = CARTESIAN_POINT ( 'NONE',  ( -68.98442902999595105, 21.93515443114010210, -9.800414904976365804 ) ) ;
#24023 = DIRECTION ( 'NONE',  ( 0.9961946980917455452, 0.000000000000000000, -0.08715574274765851281 ) ) ;
#24025 = DIRECTION ( 'NONE',  ( 0.000000000000000000, 0.000000000000000000, 1.000000000000000000 ) ) ;
#24026 = CARTESIAN_POINT ( 'NONE',  ( -59.87552183813137674, 24.84364830758654108, -46.17089178453873188 ) ) ;
#24027 = CARTESIAN_POINT ( 'NONE',  ( 21.72652366223498177, 6.198145607837613369, -3.240109526687368291 ) ) ;
#24028 = VERTEX_POINT ( 'NONE', #1758 ) ;
#24029 = CARTESIAN_POINT ( 'NONE',  ( 5.026281758278582146, -30.27593629695115496, 6.864216812889196717 ) ) ;
#24030 = AXIS2_PLACEMENT_3D ( 'NONE', #27096, #5076, #33293 ) ;
#24031 = CARTESIAN_POINT ( 'NONE',  ( 22.81652408475101979, -6.765098194116612618, -2.522738730058198264 ) ) ;
#24032 = CIRCLE ( 'NONE', #22750, 0.1000000000000028644 ) ;
#24033 = DIRECTION ( 'NONE',  ( -0.000000000000000000, -0.000000000000000000, -1.000000000000000000 ) ) ;
#24034 = VERTEX_POINT ( 'NONE', #14085 ) ;
#24035 = CARTESIAN_POINT ( 'NONE',  ( 1.067097196290011318, -33.00081685525598374, 7.781480525794718162 ) ) ;
#24036 = CARTESIAN_POINT ( 'NONE',  ( 80.45827632841071875, 65.09029793562214650, 3.202775791561846663 ) ) ;
#24037 = CARTESIAN_POINT ( 'NONE',  ( 84.45327006356104960, 2.923007647743876447, -2.091752339247905823 ) ) ;
#24038 = FACE_OUTER_BOUND ( 'NONE', #27887, .T. ) ;
#24039 = EDGE_LOOP ( 'NONE', ( #24892, #19749, #19280, #12941 ) ) ;
#24040 = CYLINDRICAL_SURFACE ( 'NONE', #10865, 0.09010775117052811922 ) ;
#24041 = VECTOR ( 'NONE', #10719, 1000.000000000000000 ) ;
#24042 = DIRECTION ( 'NONE',  ( 0.000000000000000000, 0.6662082868431845606, 0.7457657263118687707 ) ) ;
#24043 = CARTESIAN_POINT ( 'NONE',  ( 31.36819916996323698, -3.287745066446770892, -5.091721761760051201 ) ) ;
#24044 = CARTESIAN_POINT ( 'NONE',  ( -75.45330471031414277, 33.71485196875532608, 12.50000000000000000 ) ) ;
#24045 = DIRECTION ( 'NONE',  ( 0.000000000000000000, 0.000000000000000000, -1.000000000000000000 ) ) ;
#24046 = CARTESIAN_POINT ( 'NONE',  ( 25.30174877026170321, 0.8083424722246850269, -4.611467558984948312 ) ) ;
#24047 = DIRECTION ( 'NONE',  ( -0.000000000000000000, -0.000000000000000000, 1.000000000000000000 ) ) ;
#24048 = ORIENTED_EDGE ( 'NONE', *, *, #27405, .T. ) ;
#24049 = DIRECTION ( 'NONE',  ( -0.3420201433256706003, 0.9396926207859077618, 0.000000000000000000 ) ) ;
#24050 = CARTESIAN_POINT ( 'NONE',  ( 31.83263240781453973, -2.965535539804599718, -5.174650181000254534 ) ) ;
#24051 = ORIENTED_EDGE ( 'NONE', *, *, #34749, .T. ) ;
#24052 = VERTEX_POINT ( 'NONE', #7716 ) ;
#24054 = CARTESIAN_POINT ( 'NONE',  ( 34.14254696827997293, -3.849676149305037320, 5.233320676800256699 ) ) ;
#24053 = CARTESIAN_POINT ( 'NONE',  ( 81.05462132553121535, 63.14435662960352147, -3.368075118064902007 ) ) ;
#24055 = CARTESIAN_POINT ( 'NONE',  ( -1.330295241805246498, -31.30949717850352343, 7.773839561854631874 ) ) ;
#24056 = CARTESIAN_POINT ( 'NONE',  ( -69.42837670882107659, -47.11702805680359063, 9.886859966642603581 ) ) ;
#24057 = CARTESIAN_POINT ( 'NONE',  ( 18.44527402623563361, -3.111956244387396264, -3.036883180503353596 ) ) ;
#24058 = CARTESIAN_POINT ( 'NONE',  ( 4.546924931960046656, -31.42929550842064756, 7.013842709614101167 ) ) ;
#24059 = VERTEX_POINT ( 'NONE', #20267 ) ;
#24060 = DIRECTION ( 'NONE',  ( 1.000000000000000000, 0.000000000000000000, 0.000000000000000000 ) ) ;
#24061 = ORIENTED_EDGE ( 'NONE', *, *, #25439, .F. ) ;
#24062 = ORIENTED_EDGE ( 'NONE', *, *, #28605, .T. ) ;
#24063 = DIRECTION ( 'NONE',  ( 0.1736481776669361321, -0.9848077530122070211, 0.000000000000000000 ) ) ;
#24064 = CARTESIAN_POINT ( 'NONE',  ( 79.38068533922456993, 65.45287079212489800, -2.940771700540094624 ) ) ;
#24065 = CARTESIAN_POINT ( 'NONE',  ( 14.77500745536057813, -5.175466302041957789, 2.500000552286355759 ) ) ;
#24066 = VERTEX_POINT ( 'NONE', #11191 ) ;
#24067 = DIRECTION ( 'NONE',  ( -0.000000000000000000, -0.000000000000000000, 1.000000000000000000 ) ) ;
#24068 = ORIENTED_EDGE ( 'NONE', *, *, #5170, .T. ) ;
#24069 = CARTESIAN_POINT ( 'NONE',  ( 22.37319937022849814, 4.167743866275963605, 3.748729264894208324 ) ) ;
#24070 = CIRCLE ( 'NONE', #39865, 3.499999999999999556 ) ;
#24071 = CARTESIAN_POINT ( 'NONE',  ( 79.82775505260887883, 66.24998868310140665, -1.780213741554920626 ) ) ;
#24072 = EDGE_CURVE ( 'NONE', #16830, #5157, #26331, .T. ) ;
#24074 = EDGE_CURVE ( 'NONE', #30107, #5805, #24391, .T. ) ;
#24073 = CARTESIAN_POINT ( 'NONE',  ( 4.736942281967229995, -28.04042185224137995, 7.006423389747790331 ) ) ;
#24075 = EDGE_LOOP ( 'NONE', ( #37134, #19691, #17113, #19686 ) ) ;
#24076 = AXIS2_PLACEMENT_3D ( 'NONE', #11309, #10915, #26579 ) ;
#24078 = CARTESIAN_POINT ( 'NONE',  ( 1.090137774077392319, -26.22513774092466221, 7.643333865083958401 ) ) ;
#24077 = CARTESIAN_POINT ( 'NONE',  ( 1.121324086407811338, -26.64985754041175525, 6.800000000000000711 ) ) ;
#24079 = DIRECTION ( 'NONE',  ( 0.000000000000000000, 0.000000000000000000, 1.000000000000000000 ) ) ;
#24080 = CARTESIAN_POINT ( 'NONE',  ( 75.42787669100914627, 61.66269772210893763, 3.901127667181031100 ) ) ;
#24081 = CARTESIAN_POINT ( 'NONE',  ( 23.88986409409178790, 2.649682191105962037, -4.076355408754036347 ) ) ;
#24082 = ORIENTED_EDGE ( 'NONE', *, *, #34393, .F. ) ;
#24083 = DIRECTION ( 'NONE',  ( -0.000000000000000000, -0.000000000000000000, 1.000000000000000000 ) ) ;
#24084 = DIRECTION ( 'NONE',  ( 0.000000000000000000, 0.000000000000000000, 1.000000000000000000 ) ) ;
#24085 = DIRECTION ( 'NONE',  ( 1.000000000000000000, 0.000000000000000000, -0.000000000000000000 ) ) ;
#24086 = CARTESIAN_POINT ( 'NONE',  ( -63.41438759659862257, 35.63967351046427012, 6.822170959111637956 ) ) ;
#24087 = CARTESIAN_POINT ( 'NONE',  ( -1.653919781298413660, -29.01440746736336962, 7.680992449362115337 ) ) ;
#24088 = CARTESIAN_POINT ( 'NONE',  ( 81.95280109346369102, 63.95510859576443607, 2.731810022747816813 ) ) ;
#24089 = CARTESIAN_POINT ( 'NONE',  ( 85.32384696181071604, 2.517929975123688990, -2.669340390032339361 ) ) ;
#24090 = CARTESIAN_POINT ( 'NONE',  ( 29.67925625648019405, 0.9272574953382407559, 4.669903954941619695 ) ) ;
#24091 = CARTESIAN_POINT ( 'NONE',  ( -34.87867591359218977, -26.64985754041175525, 6.800000000000000711 ) ) ;
#24092 = CARTESIAN_POINT ( 'NONE',  ( -0.9170814437486904946, -27.39993314898963206, 7.643333865083951295 ) ) ;
#24093 = CARTESIAN_POINT ( 'NONE',  ( -18.34874870218063947, -25.49307895267003587, 6.700000000000000178 ) ) ;
#24094 = CARTESIAN_POINT ( 'NONE',  ( -64.08758708074093136, 36.14363715547680300, 3.800414904976363140 ) ) ;
#24095 = CARTESIAN_POINT ( 'NONE',  ( 34.98303455028736408, -1.566528556295725849, -5.666346628096917470 ) ) ;
#24096 = FILL_AREA_STYLE ('',( #11529 ) ) ;
#24097 = FACE_OUTER_BOUND ( 'NONE', #14288, .T. ) ;
#24098 = CIRCLE ( 'NONE', #2451, 0.1000000000000028644 ) ;
#24099 = DIRECTION ( 'NONE',  ( -0.000000000000000000, -1.000000000000000000, -0.000000000000000000 ) ) ;
#24100 = EDGE_CURVE ( 'NONE', #20712, #27773, #30783, .T. ) ;
#24101 = AXIS2_PLACEMENT_3D ( 'NONE', #30701, #18892, #2508 ) ;
#24102 = CONICAL_SURFACE ( 'NONE', #18858, 6.138794830819693793, 0.03429555972217021576 ) ;
#24103 = CARTESIAN_POINT ( 'NONE',  ( 4.392721987511531978, -31.80629977964779442, 7.749999999999998224 ) ) ;
#24104 = CARTESIAN_POINT ( 'NONE',  ( -69.92837670882107659, -0.7829914368874778541, 5.916079783099621459 ) ) ;
#24105 = ORIENTED_EDGE ( 'NONE', *, *, #1532, .T. ) ;
#24106 = CARTESIAN_POINT ( 'NONE',  ( 32.03504567309566653, 0.1963253013062704611, 4.819203286259713614 ) ) ;
#24107 = CARTESIAN_POINT ( 'NONE',  ( -70.02024225408199243, -0.3498828673826461233, 5.943034864274133078 ) ) ;
#24108 = CARTESIAN_POINT ( 'NONE',  ( 66.71461092208421917, 57.89240490252945648, -3.999756211082519552 ) ) ;
#24109 = CARTESIAN_POINT ( 'NONE',  ( -0.5587660686011224342, -26.89668496448380353, 7.756742906098588186 ) ) ;
#24110 = EDGE_CURVE ( 'NONE', #27683, #6019, #21710, .T. ) ;
#24111 = ORIENTED_EDGE ( 'NONE', *, *, #38575, .F. ) ;
#24112 = CYLINDRICAL_SURFACE ( 'NONE', #9464, 0.09010775117052736982 ) ;
#24113 = CARTESIAN_POINT ( 'NONE',  ( 3.913290293412393872, -32.15122301917286762, 7.695279973900954751 ) ) ;
#24114 = CARTESIAN_POINT ( 'NONE',  ( 68.46975562008563543, 59.13163800552559479, 3.939088990506558030 ) ) ;
#24115 = CARTESIAN_POINT ( 'NONE',  ( 86.46043323462474461, 1.241262327860113590, 4.894917242394325463 ) ) ;
#24116 = VERTEX_POINT ( 'NONE', #15109 ) ;
#24117 = DIRECTION ( 'NONE',  ( 0.000000000000000000, 1.000000000000000000, 0.000000000000000000 ) ) ;
#24118 = CARTESIAN_POINT ( 'NONE',  ( -7.890026461918812295, -6.626103207857777159E-16, 6.000000000000000000 ) ) ;
#24119 = ORIENTED_EDGE ( 'NONE', *, *, #38344, .T. ) ;
#24120 = CARTESIAN_POINT ( 'NONE',  ( 22.18852649867165283, 5.259174019323452853, 3.082925981170793861 ) ) ;
#24121 = CARTESIAN_POINT ( 'NONE',  ( 82.26973386304365476, 64.90130211351629441, -1.000000000000000000 ) ) ;
#24122 = DIRECTION ( 'NONE',  ( -0.000000000000000000, -0.000000000000000000, -1.000000000000000000 ) ) ;
#24123 = CARTESIAN_POINT ( 'NONE',  ( 81.21317738564106037, 61.78038839029203189, 2.432199249741022307 ) ) ;
#24124 = AXIS2_PLACEMENT_3D ( 'NONE', #18973, #6626, #38099 ) ;
#24126 = EDGE_CURVE ( 'NONE', #6217, #8770, #15356, .T. ) ;
#24125 = CARTESIAN_POINT ( 'NONE',  ( -4.220127061295482087E-17, 0.7293679304675931840, -6.000000000000000000 ) ) ;
#24127 = EDGE_LOOP ( 'NONE', ( #32078, #26960, #34656, #30437 ) ) ;
#24128 = CARTESIAN_POINT ( 'NONE',  ( 77.55533639035672877, 62.99992453720924601, -3.808649511194682979 ) ) ;
#24130 = CARTESIAN_POINT ( 'NONE',  ( 14.62203240282402206, -4.616478718678312276, -2.500000000000228706 ) ) ;
#24129 = CARTESIAN_POINT ( 'NONE',  ( 27.43541126664922558, 0.9752269244486642119, 4.488355539249689663 ) ) ;
#24131 = AXIS2_PLACEMENT_3D ( 'NONE', #30830, #2639, #40072 ) ;
#24132 = CARTESIAN_POINT ( 'NONE',  ( 78.99802787997164444, 66.11506539533232285, -1.704083397383983289 ) ) ;
#24133 = CARTESIAN_POINT ( 'NONE',  ( 79.68931684371919744, 62.31783030446536742, 3.554489553981594607 ) ) ;
#24134 = CIRCLE ( 'NONE', #3145, 0.1000000000000028644 ) ;
#24135 = ORIENTED_EDGE ( 'NONE', *, *, #29843, .F. ) ;
#24136 = VECTOR ( 'NONE', #10596, 1000.000000000000000 ) ;
#24137 = CARTESIAN_POINT ( 'NONE',  ( -0.8241947473075555974, -27.29254761058917822, 7.754798119455333705 ) ) ;
#24138 = ORIENTED_EDGE ( 'NONE', *, *, #2167, .T. ) ;
#24139 = CARTESIAN_POINT ( 'NONE',  ( 81.16949749213439702, 61.30395080096879212, 1.008685033153497557 ) ) ;
#24141 = LINE ( 'NONE', #23547, #34127 ) ;
#24140 = CARTESIAN_POINT ( 'NONE',  ( 3.452406831854927471, -26.65609467884121031, 7.785172627573961890 ) ) ;
#24142 = CARTESIAN_POINT ( 'NONE',  ( 26.56634348862415251, 2.991955253353971500, -0.5426703667890996341 ) ) ;
#24143 = FACE_OUTER_BOUND ( 'NONE', #20441, .T. ) ;
#24144 = FACE_OUTER_BOUND ( 'NONE', #19022, .T. ) ;
#24145 = ORIENTED_EDGE ( 'NONE', *, *, #8628, .F. ) ;
#24146 = CARTESIAN_POINT ( 'NONE',  ( -80.91031161377242142, -5.699894439238892829, -0.6008404087775668367 ) ) ;
#24147 = EDGE_CURVE ( 'NONE', #32868, #31820, #27667, .T. ) ;
#24148 = CARTESIAN_POINT ( 'NONE',  ( 4.938390203311415748E-15, -42.37473357531882101, 6.000000000000000000 ) ) ;
#24149 = ORIENTED_EDGE ( 'NONE', *, *, #13729, .T. ) ;
#24150 = CYLINDRICAL_SURFACE ( 'NONE', #29013, 0.09010775117052882699 ) ;
#24151 = CARTESIAN_POINT ( 'NONE',  ( -9.078675913592196167, -26.64985754041175525, 6.700000000000000178 ) ) ;
#24152 = CARTESIAN_POINT ( 'NONE',  ( -0.06129048428309483154, -26.54561512989744188, 7.635761828346575797 ) ) ;
#24153 = CARTESIAN_POINT ( 'NONE',  ( -1.799563906791552315, -29.54920986262704119, 6.906385212079471536 ) ) ;
#24154 = CARTESIAN_POINT ( 'NONE',  ( 33.94509347138731670, -0.4898356627277217767, -5.123723072070831996 ) ) ;
#24155 = LINE ( 'NONE', #5428, #21352 ) ;
#24156 = DIRECTION ( 'NONE',  ( -0.000000000000000000, -0.000000000000000000, 1.000000000000000000 ) ) ;
#24157 = CARTESIAN_POINT ( 'NONE',  ( 5.042410289116912026, -28.94470923627980952, 7.680992449362118002 ) ) ;
#24158 =( BOUNDED_CURVE ( )  B_SPLINE_CURVE ( 3, ( #20281, #33684, #14705, #27277 ),
 .UNSPECIFIED., .F., .T. ) 
 B_SPLINE_CURVE_WITH_KNOTS ( ( 4, 4 ),
 ( 1.381924640371169355, 1.574767692156078036 ),
 .UNSPECIFIED. ) 
 CURVE ( )  GEOMETRIC_REPRESENTATION_ITEM ( )  RATIONAL_B_SPLINE_CURVE ( ( 1.000000000000000000, 0.9969033633783032089, 0.9969033633783032089, 1.000000000000000000 ) ) 
 REPRESENTATION_ITEM ( '' )  );
#24159 = DIRECTION ( 'NONE',  ( 0.000000000000000000, 0.000000000000000000, 1.000000000000000000 ) ) ;
#24160 = LINE ( 'NONE', #20455, #10176 ) ;
#24161 = CARTESIAN_POINT ( 'NONE',  ( 2.338742698598150316, -26.23039339646865287, 6.894806418505346812 ) ) ;
#24162 = CARTESIAN_POINT ( 'NONE',  ( 4.885209878933623351, -28.37958095652696144, 7.730758795053806587 ) ) ;
#24163 = AXIS2_PLACEMENT_3D ( 'NONE', #31665, #19096, #6551 ) ;
#24164 = DIRECTION ( 'NONE',  ( 0.000000000000000000, 1.000000000000000000, 0.000000000000000000 ) ) ;
#24165 = CARTESIAN_POINT ( 'NONE',  ( 22.52490398424734863, 1.961233960008371024, -5.344660709420910649 ) ) ;
#24166 = ORIENTED_EDGE ( 'NONE', *, *, #34503, .T. ) ;
#24167 = EDGE_CURVE ( 'NONE', #17561, #29464, #33874, .T. ) ;
#24169 = VERTEX_POINT ( 'NONE', #34487 ) ;
#24168 = AXIS2_PLACEMENT_3D ( 'NONE', #28128, #40681, #12487 ) ;
#24170 = CARTESIAN_POINT ( 'NONE',  ( 66.27376694608996388, 57.73522568913447373, 4.000000000000000000 ) ) ;
#24171 = AXIS2_PLACEMENT_3D ( 'NONE', #11277, #29633, #29829 ) ;
#24172 = CARTESIAN_POINT ( 'NONE',  ( 69.35860043680946774, 58.39594701590269921, -3.954017255840812872 ) ) ;
#24173 = VECTOR ( 'NONE', #14738, 1000.000000000000000 ) ;
#24174 = EDGE_CURVE ( 'NONE', #1835, #37531, #25252, .T. ) ;
#24175 = VERTEX_POINT ( 'NONE', #37537 ) ;
#24176 = CARTESIAN_POINT ( 'NONE',  ( -0.9886485709270328437, -27.32959591667594523, 7.756742906098588186 ) ) ;
#24177 = CARTESIAN_POINT ( 'NONE',  ( -0.8494288436016770305, -27.16237997642270585, 7.387053503561888057 ) ) ;
#24178 = CARTESIAN_POINT ( 'NONE',  ( 3.055224846074477529, -26.45152950476128595, 6.929923840112066635 ) ) ;
#24179 = DIRECTION ( 'NONE',  ( -1.000000000000000000, 0.000000000000000000, -0.000000000000000000 ) ) ;
#24180 = FACE_OUTER_BOUND ( 'NONE', #39971, .T. ) ;
#24181 = ORIENTED_EDGE ( 'NONE', *, *, #27944, .F. ) ;
#24182 = CARTESIAN_POINT ( 'NONE',  ( 24.42597585396890025, 3.174433883044760929, 3.223073399387599736 ) ) ;
#24183 =( NAMED_UNIT ( * ) PLANE_ANGLE_UNIT ( ) SI_UNIT ( $, .RADIAN. ) );
#24184 = EDGE_CURVE ( 'NONE', #615, #37655, #15049, .T. ) ;
#24185 = ORIENTED_EDGE ( 'NONE', *, *, #39129, .T. ) ;
#24186 = CARTESIAN_POINT ( 'NONE',  ( 80.75587274821523920, 61.22306450394816579, -1.910479420724443989 ) ) ;
#24187 = CARTESIAN_POINT ( 'NONE',  ( 17.20447544827797515, 12.11625409491893812, -2.500000000000000444 ) ) ;
#24188 = CARTESIAN_POINT ( 'NONE',  ( 79.66325760479739415, 66.16013226748967213, -2.011780557866151398 ) ) ;
#24189 = CARTESIAN_POINT ( 'NONE',  ( 79.08605325858584933, 64.90301710537215740, 3.311815948186460634 ) ) ;
#24190 = CARTESIAN_POINT ( 'NONE',  ( 8.290806648384990041, 0.000000000000000000, 6.000000000000000000 ) ) ;
#24191 = CARTESIAN_POINT ( 'NONE',  ( -0.9786759135921931918, -24.55319635012989110, 6.800000000000000711 ) ) ;
#24192 = CARTESIAN_POINT ( 'NONE',  ( 21.85643539959776760, -1.092963988217814375, -14.35370713741404458 ) ) ;
#24193 = AXIS2_PLACEMENT_3D ( 'NONE', #7884, #17737, #33835 ) ;
#24194 = ORIENTED_EDGE ( 'NONE', *, *, #8530, .F. ) ;
#24195 = CARTESIAN_POINT ( 'NONE',  ( -79.25269282065100640, 11.47373787457623884, 5.555836242586228657 ) ) ;
#24196 = CARTESIAN_POINT ( 'NONE',  ( 14.69276469947978647, -4.522233606460802413, 2.500000000000264233 ) ) ;
#24197 = CARTESIAN_POINT ( 'NONE',  ( -75.90835578683964968, 8.772181813903891623, -10.10645397056114803 ) ) ;
#24198 = DIRECTION ( 'NONE',  ( 0.000000000000000000, 0.000000000000000000, -1.000000000000000000 ) ) ;
#24199 = CARTESIAN_POINT ( 'NONE',  ( 2.413333108735914223, -26.24550221827435337, 6.863904403958575706 ) ) ;
#24200 = CARTESIAN_POINT ( 'NONE',  ( -1.750118104476454439, -30.09189987372638342, 7.780491323090171996 ) ) ;
#24201 = CARTESIAN_POINT ( 'NONE',  ( 2.850561110411099275, -26.37038230420113649, 7.635761828346577573 ) ) ;
#24202 = PLANE ( 'NONE',  #7617 ) ;
#24203 = CARTESIAN_POINT ( 'NONE',  ( -70.12815439591902589, -0.1689404852770337306, 9.968370014334123397 ) ) ;
#24204 = DIRECTION ( 'NONE',  ( -1.000000000000000000, 0.000000000000000000, 0.000000000000000000 ) ) ;
#24205 = CARTESIAN_POINT ( 'NONE',  ( 3.977572546501451978, -32.22783162523180778, 7.697032948437509070 ) ) ;
#24206 = ADVANCED_FACE ( 'NONE', ( #18596 ), #37136, .F. ) ;
#24207 = CARTESIAN_POINT ( 'NONE',  ( 86.80189613381685376, 0.8577149926806704183, 5.030330955187197972 ) ) ;
#24208 = DIRECTION ( 'NONE',  ( 0.000000000000000000, 0.000000000000000000, 1.000000000000000000 ) ) ;
#24209 = ORIENTED_EDGE ( 'NONE', *, *, #16666, .T. ) ;
#24210 = AXIS2_PLACEMENT_3D ( 'NONE', #20745, #21169, #27131 ) ;
#24211 = CARTESIAN_POINT ( 'NONE',  ( 67.67991563464998706, 58.42724437289452055, 3.992148460412343614 ) ) ;
#24212 = CARTESIAN_POINT ( 'NONE',  ( 35.78817461119013643, -3.222426957731786334, 5.792008206986667851 ) ) ;
#24213 = B_SPLINE_CURVE_WITH_KNOTS ( 'NONE', 3,
 ( #37087, #2536, #8877, #21662 ),
 .UNSPECIFIED., .F., .F.,
 ( 4, 4 ),
 ( 0.000000000000000000, 6.391136169899793690E-06 ),
 .UNSPECIFIED. ) ;
#24214 = EDGE_CURVE ( 'NONE', #36832, #4935, #2587, .T. ) ;
#24215 = DIRECTION ( 'NONE',  ( 1.000000000000000000, -0.000000000000000000, -0.000000000000000000 ) ) ;
#24216 = CARTESIAN_POINT ( 'NONE',  ( 84.97295377430323526, 2.662001904288300302, 3.416982328422734305 ) ) ;
#24218 = DIRECTION ( 'NONE',  ( 0.1736481776669273613, 0.9848077530122086864, -0.000000000000000000 ) ) ;
#24217 = CARTESIAN_POINT ( 'NONE',  ( -25.07867591359219617, -24.55319635012989110, 6.700000000000000178 ) ) ;
#24219 = DIRECTION ( 'NONE',  ( 1.385724075720358314E-16, -1.000000000000000000, 0.000000000000000000 ) ) ;
#24220 = CARTESIAN_POINT ( 'NONE',  ( 33.45855146796573365, -3.830112298179899177, 5.093503661137224192 ) ) ;
#24221 = CARTESIAN_POINT ( 'NONE',  ( -19.07867591359219972, -26.64985754041175525, 6.700000000000000178 ) ) ;
#24222 = AXIS2_PLACEMENT_3D ( 'NONE', #30349, #2155, #14675 ) ;
#24223 = EDGE_LOOP ( 'NONE', ( #26368, #21856, #21782, #32104, #22260, #10469, #33157 ) ) ;
#24224 = CARTESIAN_POINT ( 'NONE',  ( -70.22814611767556414, -21.49690818219047017, 3.958999674376895150 ) ) ;
#24225 = UNCERTAINTY_MEASURE_WITH_UNIT (LENGTH_MEASURE( 1.000000000000000082E-05 ), #4937, 'distance_accuracy_value', 'NONE');
#24226 = CARTESIAN_POINT ( 'NONE',  ( 81.04520860822712791, 61.30615853997439046, -1.682919622592479625 ) ) ;
#24227 = CARTESIAN_POINT ( 'NONE',  ( 3.099557997805675313, -32.67648533487435714, 7.505001789837626447 ) ) ;
#24228 = CARTESIAN_POINT ( 'NONE',  ( 78.64443580140854806, 65.97314938607597412, 1.660510093083201744 ) ) ;
#24229 = CARTESIAN_POINT ( 'NONE',  ( 23.60520478173619807, 0.4415638201438380483, 5.510117418379326892 ) ) ;
#24231 = ORIENTED_EDGE ( 'NONE', *, *, #36221, .T. ) ;
#24230 = CARTESIAN_POINT ( 'NONE',  ( 4.740470269852407270, -27.86479572999185450, 7.785096263473211486 ) ) ;
#24232 = CARTESIAN_POINT ( 'NONE',  ( 74.55930941259208566, 60.55296354997373953, -3.883841728571185481 ) ) ;
#24233 = CARTESIAN_POINT ( 'NONE',  ( 3.224716257031337019, -32.60908495567738896, 6.911401339314956260 ) ) ;
#24234 = CLOSED_SHELL ( 'NONE', ( #32471, #20617, #28192, #15670, #15636, #34100, #20210, #13056, #37278, #21909, #26152, #22276, #26184 ) ) ;
#24236 = LINE ( 'NONE', #36797, #36128 ) ;
#24235 = CARTESIAN_POINT ( 'NONE',  ( 4.955822899483663946, -30.85533363526925754, 6.863805608295730387 ) ) ;
#24237 = CARTESIAN_POINT ( 'NONE',  ( -1.228840775939959551, -27.84377650683858718, 7.782167645815904145 ) ) ;
#24238 = PLANE ( 'NONE',  #3809 ) ;
#24239 = DIRECTION ( 'NONE',  ( 0.9396926207859082059, 0.3420201433256695456, -0.000000000000000000 ) ) ;
#24240 = ORIENTED_EDGE ( 'NONE', *, *, #38755, .F. ) ;
#24241 = DIRECTION ( 'NONE',  ( 0.8660254037844449249, -0.4999999999999888423, -0.000000000000000000 ) ) ;
#24242 = CARTESIAN_POINT ( 'NONE',  ( 24.08269697565317813, 2.216436711090640888, -5.807619368686713024 ) ) ;
#24243 = LINE ( 'NONE', #5515, #8418 ) ;
#24244 = DIRECTION ( 'NONE',  ( -0.000000000000000000, -0.000000000000000000, 1.000000000000000000 ) ) ;
#24245 = CARTESIAN_POINT ( 'NONE',  ( 81.36706168520311167, 62.61468991663328154, 3.015642068896308370 ) ) ;
#24246 = CARTESIAN_POINT ( 'NONE',  ( 86.54029261786013194, -0.3196574014320466284, 5.877194713501632251 ) ) ;
#24247 = DIRECTION ( 'NONE',  ( -0.000000000000000000, -0.000000000000000000, 1.000000000000000000 ) ) ;
#24248 = ORIENTED_EDGE ( 'NONE', *, *, #4157, .T. ) ;
#24249 = CARTESIAN_POINT ( 'NONE',  ( 4.546924931960046656, -31.42929550842064756, 7.013842709614101167 ) ) ;
#24250 = EDGE_CURVE ( 'NONE', #20163, #32142, #12631, .T. ) ;
#24251 = AXIS2_PLACEMENT_3D ( 'NONE', #35341, #37989, #19470 ) ;
#24252 = CARTESIAN_POINT ( 'NONE',  ( 5.059341540990399011, -29.04314055594101163, 6.880147297696982633 ) ) ;
#24253 = EDGE_CURVE ( 'NONE', #33136, #32235, #38390, .T. ) ;
#24254 = CARTESIAN_POINT ( 'NONE',  ( 33.13127733337127978, -3.703616631181526397, -5.170032777214017550 ) ) ;
#24255 = CARTESIAN_POINT ( 'NONE',  ( -65.87013514634764988, 36.66000420377759639, -7.725785790320288449 ) ) ;
#24256 = PLANE ( 'NONE',  #20055 ) ;
#24257 = DIRECTION ( 'NONE',  ( -1.000000000000000000, 0.000000000000000000, 0.000000000000000000 ) ) ;
#24258 = VERTEX_POINT ( 'NONE', #12434 ) ;
#24259 = CARTESIAN_POINT ( 'NONE',  ( 32.77846936337113704, -0.9351094977892036031, 5.322270913068036791 ) ) ;
#24260 = ADVANCED_FACE ( 'NONE', ( #6474 ), #21298, .T. ) ;
#24261 = ADVANCED_FACE ( 'NONE', ( #12005 ), #24585, .F. ) ;
#24262 = CARTESIAN_POINT ( 'NONE',  ( -1.215384403943503555, -27.82114229413565099, 6.887041543973311697 ) ) ;
#24263 = VECTOR ( 'NONE', #15022, 1000.000000000000000 ) ;
#24264 = VERTEX_POINT ( 'NONE', #18397 ) ;
#24265 = ORIENTED_EDGE ( 'NONE', *, *, #14569, .F. ) ;
#24267 = CARTESIAN_POINT ( 'NONE',  ( 33.11406552165681916, -0.1504008805997818499, 4.940950335661676185 ) ) ;
#24266 = CARTESIAN_POINT ( 'NONE',  ( 81.33630325801044592, 62.05105258569628290, -2.628317182735725677 ) ) ;
#24268 = DIRECTION ( 'NONE',  ( 0.000000000000000000, 0.000000000000000000, 1.000000000000000000 ) ) ;
#24269 =( BOUNDED_CURVE ( )  B_SPLINE_CURVE ( 3, ( #13189, #38293, #16474, #19373 ),
 .UNSPECIFIED., .F., .T. ) 
 B_SPLINE_CURVE_WITH_KNOTS ( ( 4, 4 ),
 ( 1.381924640371167579, 1.574767692156075594 ),
 .UNSPECIFIED. ) 
 CURVE ( )  GEOMETRIC_REPRESENTATION_ITEM ( )  RATIONAL_B_SPLINE_CURVE ( ( 1.000000000000000000, 0.9969033633783032089, 0.9969033633783032089, 1.000000000000000000 ) ) 
 REPRESENTATION_ITEM ( '' )  );
#24270 = CARTESIAN_POINT ( 'NONE',  ( 25.55635707441696880, -2.736503067813388590, 4.195085622931020275 ) ) ;
#24271 = CARTESIAN_POINT ( 'NONE',  ( 1.751596854648554302, -26.17031492517298474, 6.892063359921933419 ) ) ;
#24272 = DIRECTION ( 'NONE',  ( -0.000000000000000000, -0.000000000000000000, 1.000000000000000000 ) ) ;
#24273 = LINE ( 'NONE', #17877, #37574 ) ;
#24274 = ORIENTED_EDGE ( 'NONE', *, *, #26030, .T. ) ;
#24275 = CARTESIAN_POINT ( 'NONE',  ( -2.348748702180637693, -25.49307895267003587, 6.700000000000000178 ) ) ;
#24276 = ORIENTED_EDGE ( 'NONE', *, *, #11545, .F. ) ;
#24277 = ORIENTED_EDGE ( 'NONE', *, *, #24022, .F. ) ;
#24278 = DIRECTION ( 'NONE',  ( -0.000000000000000000, -1.000000000000000000, -0.000000000000000000 ) ) ;
#24279 = CARTESIAN_POINT ( 'NONE',  ( 80.30796587587548174, 63.87804906342756084, -3.654032574946329603 ) ) ;
#24280 = CARTESIAN_POINT ( 'NONE',  ( -10.44874870218064089, -25.49307895267003587, 6.700000000000000178 ) ) ;
#24281 = ORIENTED_EDGE ( 'NONE', *, *, #35080, .T. ) ;
#24283 = CARTESIAN_POINT ( 'NONE',  ( 4.349665778881001366, -27.43886483293057665, 7.784476445165072533 ) ) ;
#24282 = CARTESIAN_POINT ( 'NONE',  ( 22.24827523181307143, 3.072553326788747707, 4.656571929184647907 ) ) ;
#24284 = VERTEX_POINT ( 'NONE', #30985 ) ;
#24285 = CARTESIAN_POINT ( 'NONE',  ( 82.09393942629647256, 63.66644892668119127, -2.541832380859317286 ) ) ;
#24286 = CARTESIAN_POINT ( 'NONE',  ( -70.92837670224925262, -21.78291075600659354, 3.999987187540717137 ) ) ;
#24288 = CARTESIAN_POINT ( 'NONE',  ( 15.73410864315090762, -3.515507921127240643, -2.662086203255957351 ) ) ;
#24287 = CARTESIAN_POINT ( 'NONE',  ( 0.06174230887167742737, -26.59084733370359999, 7.784476445165073422 ) ) ;
#24289 = CARTESIAN_POINT ( 'NONE',  ( -1.794332605514025181, -29.37780194793158373, 6.951256099901591767 ) ) ;
#24290 = CARTESIAN_POINT ( 'NONE',  ( 73.39456880541679595, 61.63402075718063600, 3.749455561531862546 ) ) ;
#24291 = CARTESIAN_POINT ( 'NONE',  ( 22.83256966555022771, 3.311254434957428217, -4.047795553463541474 ) ) ;
#24292 = LINE ( 'NONE', #2912, #11221 ) ;
#24293 = CARTESIAN_POINT ( 'NONE',  ( 21.85643539959776760, 9.535790418011023561, -9.299971273199719946 ) ) ;
#24294 = AXIS2_PLACEMENT_3D ( 'NONE', #32576, #19605, #32970 ) ;
#24295 = PLANE ( 'NONE',  #6567 ) ;
#24296 = ORIENTED_EDGE ( 'NONE', *, *, #20216, .F. ) ;
#24297 = CARTESIAN_POINT ( 'NONE',  ( -65.15514661499976512, 34.97220226750604866, 6.888442104241534913 ) ) ;
#24298 = CARTESIAN_POINT ( 'NONE',  ( 81.73829655978381936, 61.84901640042588866, 1.708467252431126626 ) ) ;
#24299 = CARTESIAN_POINT ( 'NONE',  ( 86.12362567153361681, 1.619580568575353485, 4.895344567657775592 ) ) ;
#24300 = CARTESIAN_POINT ( 'NONE',  ( 13.52694889643372278, 17.29870644234688370, 2.500000000000000000 ) ) ;
#24301 = DIRECTION ( 'NONE',  ( -0.000000000000000000, -1.000000000000000000, -0.000000000000000000 ) ) ;
#24302 = CARTESIAN_POINT ( 'NONE',  ( 1.551251297819356001, -25.49307895267003587, 6.800000000000000711 ) ) ;
#24303 = CARTESIAN_POINT ( 'NONE',  ( 17.15375077719031438, -3.245341706395144410, 2.857006424881785911 ) ) ;
#24304 = DIRECTION ( 'NONE',  ( -0.000000000000000000, -1.000000000000000000, -0.000000000000000000 ) ) ;
#24305 = CARTESIAN_POINT ( 'NONE',  ( 36.64653950724111553, -2.460867072496613517, -5.925976808648774075 ) ) ;
#24306 = CARTESIAN_POINT ( 'NONE',  ( 5.197144683283896782, -29.57049166273291263, 7.767720160662275219 ) ) ;
#24307 = DIRECTION ( 'NONE',  ( -0.5000000000000039968, 0.8660254037844362651, -0.000000000000000000 ) ) ;
#24309 = CIRCLE ( 'NONE', #5900, 0.1000000000000028644 ) ;
#24308 = CARTESIAN_POINT ( 'NONE',  ( 1.578585683582428345, -33.06757917596850405, 7.754798119455333705 ) ) ;
#24310 = ADVANCED_FACE ( 'NONE', ( #2790 ), #25805, .T. ) ;
#24311 = CARTESIAN_POINT ( 'NONE',  ( -69.42837670882107659, -47.11702805680359063, 5.809475019311128641 ) ) ;
#24312 = EDGE_CURVE ( 'NONE', #24578, #7785, #39019, .T. ) ;
#24313 = ORIENTED_EDGE ( 'NONE', *, *, #20671, .F. ) ;
#24314 = CARTESIAN_POINT ( 'NONE',  ( 37.09095381799627944, -3.108752521506979338, 5.978566616837214909 ) ) ;
#24315 = CARTESIAN_POINT ( 'NONE',  ( -71.92837670882107659, -0.7829914368874768549, 3.916079783099621014 ) ) ;
#24316 = CARTESIAN_POINT ( 'NONE',  ( 66.84168730393145097, 57.99964773888063974, -3.999029912551660182 ) ) ;
#24317 = DIRECTION ( 'NONE',  ( -0.000000000000000000, -0.000000000000000000, 1.000000000000000000 ) ) ;
#24318 = DIRECTION ( 'NONE',  ( 1.000000000000000000, 0.000000000000000000, 0.000000000000000000 ) ) ;
#24319 = ORIENTED_EDGE ( 'NONE', *, *, #33873, .F. ) ;
#24320 = FACE_OUTER_BOUND ( 'NONE', #35618, .T. ) ;
#24321 = AXIS2_PLACEMENT_3D ( 'NONE', #34711, #19238, #22137 ) ;
#24322 = CARTESIAN_POINT ( 'NONE',  ( -72.37659067963534198, 5.886899662738341199, -9.895437931856170266 ) ) ;
#24323 = CARTESIAN_POINT ( 'NONE',  ( 2.921324086407800280, -26.64985754041175525, 6.800000000000000711 ) ) ;
#24324 = CARTESIAN_POINT ( 'NONE',  ( -10.87867591359219155, -26.64985754041175525, 6.800000000000000711 ) ) ;
#24325 = EDGE_LOOP ( 'NONE', ( #11037, #16048, #20892, #21305, #7335, #21502, #1264 ) ) ;
#24326 = LINE ( 'NONE', #15465, #13530 ) ;
#24327 = CARTESIAN_POINT ( 'NONE',  ( 1.272790698195233938, -26.09614646471635524, 6.912143950357348743 ) ) ;
#24328 = VERTEX_POINT ( 'NONE', #19632 ) ;
#24329 = CARTESIAN_POINT ( 'NONE',  ( 23.72357854948797140, 3.529942696455977025, 3.269053811182030866 ) ) ;
#24330 = CARTESIAN_POINT ( 'NONE',  ( 82.59411735159429213, 63.56171878218356852, -1.000000000000000000 ) ) ;
#24331 = CARTESIAN_POINT ( 'NONE',  ( -72.84815947045233031, 2.429809908903243443, 12.50000000000000000 ) ) ;
#24332 = CARTESIAN_POINT ( 'NONE',  ( 78.93014367432635936, 65.87924701951081374, 2.174925636353740366 ) ) ;
#24333 = VERTEX_POINT ( 'NONE', #22925 ) ;
#24334 = CARTESIAN_POINT ( 'NONE',  ( -36.34874870218064302, -26.64985754041175525, 6.700000000000000178 ) ) ;
#24335 = ORIENTED_EDGE ( 'NONE', *, *, #23701, .T. ) ;
#24336 = CARTESIAN_POINT ( 'NONE',  ( 79.35831483666115105, 61.48221340643407729, -3.218236826935543249 ) ) ;
#24338 = LINE ( 'NONE', #36902, #3967 ) ;
#24337 = CARTESIAN_POINT ( 'NONE',  ( 25.40538314162099809, 0.6392986327759521137, 4.601631931458681990 ) ) ;
#24339 = CARTESIAN_POINT ( 'NONE',  ( 80.70340038347460165, 64.47061299330862028, -3.456914256419914455 ) ) ;
#24340 = CARTESIAN_POINT ( 'NONE',  ( 78.41725481636187567, 64.09006905928654874, 3.590127757398426933 ) ) ;
#24341 = ORIENTED_EDGE ( 'NONE', *, *, #21156, .T. ) ;
#24342 = ORIENTED_EDGE ( 'NONE', *, *, #38525, .F. ) ;
#24343 = CIRCLE ( 'NONE', #27633, 0.1000000000000028644 ) ;
#24344 = CARTESIAN_POINT ( 'NONE',  ( -0.8969834501566193996, -27.37591117031255195, 7.775108481317158926 ) ) ;
#24345 = CARTESIAN_POINT ( 'NONE',  ( 81.16944410057618597, 61.30393124705405938, 1.011532654301222856 ) ) ;
#24347 = DIRECTION ( 'NONE',  ( -0.4999999999999962808, 0.8660254037844408170, 0.000000000000000000 ) ) ;
#24346 = CARTESIAN_POINT ( 'NONE',  ( 3.503008481831729082, -26.68712402683863161, 7.757178535559534183 ) ) ;
#24348 = CARTESIAN_POINT ( 'NONE',  ( 31.72291873093343284, -3.714249907566092634, 4.801291842747894556 ) ) ;
#24349 = CARTESIAN_POINT ( 'NONE',  ( 14.62597543585568793, -4.708289007715579899, -2.500000000000003997 ) ) ;
#24350 = PLANE ( 'NONE',  #3603 ) ;
#24351 = CARTESIAN_POINT ( 'NONE',  ( 1.574665456181726375, -33.06768670341953253, 6.867199677474203234 ) ) ;
#24352 = CARTESIAN_POINT ( 'NONE',  ( 21.79667146064388206, 0.2347865111010814521, -8.327566971649902783 ) ) ;
#24353 = LINE ( 'NONE', #37516, #10357 ) ;
#24354 = ORIENTED_EDGE ( 'NONE', *, *, #5402, .F. ) ;
#24355 = DIRECTION ( 'NONE',  ( -0.000000000000000000, -0.000000000000000000, 1.000000000000000000 ) ) ;
#24356 = CARTESIAN_POINT ( 'NONE',  ( -0.5909859742846951258, -26.91526153312021563, 7.255881584735162093 ) ) ;
#24357 = CARTESIAN_POINT ( 'NONE',  ( 5.172564876073734830, -29.12947328719863194, 7.013842709614101167 ) ) ;
#24358 = VECTOR ( 'NONE', #35481, 1000.000000000000000 ) ;
#24359 = CARTESIAN_POINT ( 'NONE',  ( -66.99872204295122913, 28.48507918597134037, -46.17089178453873188 ) ) ;
#24360 = CARTESIAN_POINT ( 'NONE',  ( 36.47577210302739559, -3.472112016856729877, -5.836390310795054326 ) ) ;
#24361 = CARTESIAN_POINT ( 'NONE',  ( 3.369155479471896530, -26.60763004909045293, 7.695279973900954751 ) ) ;
#24362 = CARTESIAN_POINT ( 'NONE',  ( 27.06148380711046642, 1.345426480462052821, -4.421175649609593528 ) ) ;
#24363 = CARTESIAN_POINT ( 'NONE',  ( -0.07465813067054014041, -26.55344152887859011, 7.730015791551945625 ) ) ;
#24364 = CARTESIAN_POINT ( 'NONE',  ( 6.019945922396399141, -27.01350538757900210, 7.695279973900954751 ) ) ;
#24365 = CARTESIAN_POINT ( 'NONE',  ( -68.98442902999595105, 21.93515443114010210, -12.49999999999999645 ) ) ;
#24366 = CARTESIAN_POINT ( 'NONE',  ( -74.47588865074813214, 7.309999117102635502, 10.65416010709459194 ) ) ;
#24367 = CARTESIAN_POINT ( 'NONE',  ( 4.882868366733327470, -28.37333834040810032, 7.695279973900954751 ) ) ;
#24368 = CARTESIAN_POINT ( 'NONE',  ( 14.73396276735570787, -4.758955132908557317, -2.504555023738491037 ) ) ;
#24369 = CARTESIAN_POINT ( 'NONE',  ( 24.83719285264605148, 2.308780662792858429, -4.092877271418466023 ) ) ;
#24370 = EDGE_CURVE ( 'NONE', #11160, #13546, #22373, .T. ) ;
#24371 = ORIENTED_EDGE ( 'NONE', *, *, #37726, .T. ) ;
#24372 = PRESENTATION_STYLE_ASSIGNMENT (( #37532 ) ) ;
#24373 = CARTESIAN_POINT ( 'NONE',  ( 69.65195751129601831, 59.35873293165669651, -3.965028736237012907 ) ) ;
#24374 = VECTOR ( 'NONE', #24164, 1000.000000000000000 ) ;
#24375 = CARTESIAN_POINT ( 'NONE',  ( 2.270779804372443422, -33.02314641928401784, 6.887161170156907097 ) ) ;
#24376 = ORIENTED_EDGE ( 'NONE', *, *, #9115, .F. ) ;
#24377 = DIRECTION ( 'NONE',  ( -1.000000000000000000, 0.000000000000000000, 0.000000000000000000 ) ) ;
#24378 = CYLINDRICAL_SURFACE ( 'NONE', #7455, 0.09010775117052870209 ) ;
#24379 = CARTESIAN_POINT ( 'NONE',  ( 3.043504320637459681, -26.44646349201601865, 6.903372536218459032 ) ) ;
#24380 = B_SPLINE_SURFACE_WITH_KNOTS ( 'NONE', 3, 1, ( 
 ( #1607, #14536 ),
 ( #36382, #39250 ),
 ( #32701, #4501 ),
 ( #29599, #35987 ),
 ( #17623, #5088 ),
 ( #1414, #7769 ),
 ( #30199, #32901 ),
 ( #4688, #14141 ),
 ( #27110, #11042 ),
 ( #1814, #39660 ),
 ( #11442, #35597 ),
 ( #7367, #3059 ),
 ( #2844, #15161 ),
 ( #30409, #11647 ),
 ( #33714, #11856 ),
 ( #6116, #37394 ),
 ( #8568, #24432 ),
 ( #9188, #14957 ),
 ( #31038, #21762 ),
 ( #17828, #40272 ),
 ( #2436, #15365 ),
 ( #21565, #24224 ),
 ( #27921, #8978 ),
 ( #18243, #21147 ),
 ( #5493, #40684 ),
 ( #24635, #36784 ),
 ( #40077, #36986 ),
 ( #18651, #8768 ),
 ( #24008, #36583 ),
 ( #5703, #27525 ),
 ( #2218, #21351 ) ),
 .UNSPECIFIED., .F., .F., .F.,
 ( 4, 3, 3, 3, 3, 3, 3, 3, 3, 3, 4 ),
 ( 2, 2 ),
 ( 0.000000000000000000, 0.1064040534484947120, 0.2127447817800686702, 0.3200334471358569077, 0.4279895727010785689, 0.5349334657245098379, 0.6407861787064418335, 0.7471238984184976895, 0.8547834834472671783, 0.9625789755878066956, 1.000000000000000000 ),
 ( 0.000000000000000000, 1.000000000000000000 ),
 .UNSPECIFIED. ) ;
#24382 = CARTESIAN_POINT ( 'NONE',  ( 4.903710960591165069, -30.70956631902851086, 7.740055089680402567 ) ) ;
#24381 = CARTESIAN_POINT ( 'NONE',  ( -0.8732574325522374226, -27.19792959302312596, 6.887547729233686411 ) ) ;
#24383 = APPLICATION_PROTOCOL_DEFINITION ( 'draft international standard', 'automotive_design', 1998, #6089 ) ;
#24384 = CARTESIAN_POINT ( 'NONE',  ( -38.44874870218063734, -26.64985754041175525, 6.800000000000000711 ) ) ;
#24385 = ORIENTED_EDGE ( 'NONE', *, *, #18840, .F. ) ;
#24386 = CARTESIAN_POINT ( 'NONE',  ( 23.43766775396862911, 3.794989907829951825, 3.097544954452251087 ) ) ;
#24387 = SURFACE_STYLE_FILL_AREA ( #14913 ) ;
#24388 = CIRCLE ( 'NONE', #11874, 15.73502530973474478 ) ;
#24389 = VERTEX_POINT ( 'NONE', #4401 ) ;
#24390 = CARTESIAN_POINT ( 'NONE',  ( 80.65804582012491153, 61.64568945823260293, -2.699019001080977365 ) ) ;
#24391 = B_SPLINE_CURVE_WITH_KNOTS ( 'NONE', 3,
 ( #2171, #32849, #5445, #20466, #36137, #23762, #14691, #21097, #39401, #4639, #23956, #20669, #33254, #27258, #17987, #5037, #17569, #11594, #33668, #2380, #36937, #15316, #18809, #28487, #34697, #12223, #28076, #19024, #37341, #34292, #9331 ),
 .UNSPECIFIED., .F., .F.,
 ( 4, 3, 3, 3, 3, 3, 3, 3, 3, 3, 4 ),
 ( 1.117570019170468176E-18, 2.999644130997731624E-05, 6.002588995694847643E-05, 8.960886084588059531E-05, 0.0001190604700446496486, 0.0001489538463052702297, 0.0001796139255493970418, 0.0002109707048517063196, 0.0002426195318110334050, 0.0002740640997890030940, 0.0002849778069099824138 ),
 .UNSPECIFIED. ) ;
#24392 = CARTESIAN_POINT ( 'NONE',  ( 17.42606438386317791, 12.01804243839431585, -2.500000000000000444 ) ) ;
#24393 = CARTESIAN_POINT ( 'NONE',  ( 79.38089166731849389, 66.16750285958211464, -1.809109834152295093 ) ) ;
#24394 = EDGE_CURVE ( 'NONE', #28666, #22380, #272, .T. ) ;
#24395 = CARTESIAN_POINT ( 'NONE',  ( 80.58270521159307975, 62.07868998654234360, 3.101774481621348833 ) ) ;
#24396 = ORIENTED_EDGE ( 'NONE', *, *, #25541, .T. ) ;
#24397 = PLANE ( 'NONE',  #1529 ) ;
#24398 = CARTESIAN_POINT ( 'NONE',  ( 18.51830382657068341, 13.21772817956447277, 2.500000000000000444 ) ) ;
#24399 = CARTESIAN_POINT ( 'NONE',  ( 21.85643539959773207, -2.370478073490382531, -12.58538558043069600 ) ) ;
#24400 = ORIENTED_EDGE ( 'NONE', *, *, #15605, .T. ) ;
#24401 = DIRECTION ( 'NONE',  ( 1.000000000000000000, 0.000000000000000000, 0.000000000000000000 ) ) ;
#24402 = CARTESIAN_POINT ( 'NONE',  ( 37.03382163445419906, -3.210012919756318528, 5.955199199487100969 ) ) ;
#24403 = AXIS2_PLACEMENT_3D ( 'NONE', #33222, #39995, #13513 ) ;
#24404 = EDGE_CURVE ( 'NONE', #21412, #31670, #902, .T. ) ;
#24405 = LINE ( 'NONE', #9158, #26101 ) ;
#24406 = CARTESIAN_POINT ( 'NONE',  ( -75.50324732371151981, 10.04197788123400414, -8.898607310640866075 ) ) ;
#24407 = LINE ( 'NONE', #20909, #30708 ) ;
#24408 = CARTESIAN_POINT ( 'NONE',  ( 2.338742698598150316, -26.23039339646865287, 6.894806418505346812 ) ) ;
#24409 = CYLINDRICAL_SURFACE ( 'NONE', #26850, 0.1000000000000028644 ) ;
#24410 = CARTESIAN_POINT ( 'NONE',  ( 14.63934257578662290, 12.89545353563754304, 2.491221481426366680 ) ) ;
#24411 = CARTESIAN_POINT ( 'NONE',  ( 3.288727556110957462, -26.44342115354165301, 7.139344958878409031 ) ) ;
#24412 = CARTESIAN_POINT ( 'NONE',  ( -1.411741797515851271, -31.17137799540083876, 7.013842709614101167 ) ) ;
#24413 = CARTESIAN_POINT ( 'NONE',  ( 5.052258071467315759, -28.99977615411923537, 7.779495906702013741 ) ) ;
#24414 = CARTESIAN_POINT ( 'NONE',  ( -70.12865035339947894, -0.1685304919200742435, 3.947195235540182701 ) ) ;
#24415 = AXIS2_PLACEMENT_3D ( 'NONE', #26576, #8835, #30479 ) ;
#24416 = CARTESIAN_POINT ( 'NONE',  ( -0.4475183596422435683, -26.93431084857535751, 6.894806418505348589 ) ) ;
#24417 = CARTESIAN_POINT ( 'NONE',  ( 24.42049692777757741, 2.955061417206801710, -3.687805831412614310 ) ) ;
#24418 = EDGE_CURVE ( 'NONE', #7860, #6802, #11018, .T. ) ;
#24419 = EDGE_LOOP ( 'NONE', ( #23954, #12188, #3544 ) ) ;
#24420 = CARTESIAN_POINT ( 'NONE',  ( 67.18992292689074475, 57.95373832061253694, 3.997022163556062324 ) ) ;
#24421 = CARTESIAN_POINT ( 'NONE',  ( 36.43211955938636493, -3.203076905710052102, 5.892511390020157336 ) ) ;
#24422 = CARTESIAN_POINT ( 'NONE',  ( 4.952473364809343082, -30.82556682577061835, 7.784725160561909441 ) ) ;
#24423 = DIRECTION ( 'NONE',  ( -0.000000000000000000, -0.000000000000000000, 1.000000000000000000 ) ) ;
#24424 = CARTESIAN_POINT ( 'NONE',  ( 87.14327233159831110, 0.3315334873356338141, 5.689878492676547772 ) ) ;
#24426 = DIRECTION ( 'NONE',  ( 1.000000000000000000, 0.000000000000000000, -0.000000000000000000 ) ) ;
#24425 = CARTESIAN_POINT ( 'NONE',  ( -18.97867591359219475, -24.55319635012989110, 6.800000000000000711 ) ) ;
#24427 = VERTEX_POINT ( 'NONE', #19827 ) ;
#24428 = CARTESIAN_POINT ( 'NONE',  ( -1.605899657953074211, -28.77718300982459709, 6.929923840112066635 ) ) ;
#24429 = DIRECTION ( 'NONE',  ( 0.000000000000000000, 0.000000000000000000, 1.000000000000000000 ) ) ;
#24430 = ADVANCED_FACE ( 'NONE', ( #1313 ), #25405, .F. ) ;
#24431 = ORIENTED_EDGE ( 'NONE', *, *, #10732, .F. ) ;
#24432 = CARTESIAN_POINT ( 'NONE',  ( -70.70940173728274658, -21.76495738335424690, 3.997008894667204881 ) ) ;
#24433 = CARTESIAN_POINT ( 'NONE',  ( 80.89855423268610934, 61.90964448260509556, -2.818206040476792129 ) ) ;
#24434 = CARTESIAN_POINT ( 'NONE',  ( -1.699609906766908596, -29.35555682840059433, 7.376738162537630039 ) ) ;
#24435 = CARTESIAN_POINT ( 'NONE',  ( 79.61178798950636804, 64.58589821993884073, 3.525318766974264051 ) ) ;
#24437 = ORIENTED_EDGE ( 'NONE', *, *, #33342, .F. ) ;
#24436 = CARTESIAN_POINT ( 'NONE',  ( -1.799609906766908685, -29.56993018339339940, 7.620413589471895399 ) ) ;
#24438 = CARTESIAN_POINT ( 'NONE',  ( 74.04982613775094080, 61.68561850464361385, -3.815996826674513009 ) ) ;
#24439 = CARTESIAN_POINT ( 'NONE',  ( 4.298799322723926508, -31.91476908534313850, 7.750000000000000888 ) ) ;
#24441 = CARTESIAN_POINT ( 'NONE',  ( -63.06903391669472825, 38.60168910470162018, -4.000000000000000000 ) ) ;
#24440 = CARTESIAN_POINT ( 'NONE',  ( 4.918781769468254517, -30.94541378637557827, 6.941203072598468360 ) ) ;
#24442 = FACE_OUTER_BOUND ( 'NONE', #14411, .T. ) ;
#24443 = EDGE_CURVE ( 'NONE', #18492, #28666, #9752, .T. ) ;
#24444 = EDGE_CURVE ( 'NONE', #38572, #10250, #22731, .T. ) ;
#24445 = CARTESIAN_POINT ( 'NONE',  ( 23.15428476648550671, 3.937122355327012269, -3.239522367696926253 ) ) ;
#24446 = ORIENTED_EDGE ( 'NONE', *, *, #23648, .T. ) ;
#24447 = CARTESIAN_POINT ( 'NONE',  ( -7.078675913592194391, -26.64985754041175525, 6.700000000000000178 ) ) ;
#24448 = ADVANCED_FACE ( 'NONE', ( #33616 ), #20823, .F. ) ;
#24449 = CARTESIAN_POINT ( 'NONE',  ( 23.92064240948634790, 4.179079982057642972, -0.5982227118658990372 ) ) ;
#24450 = CARTESIAN_POINT ( 'NONE',  ( 2.875937710231030398, -32.76024173560432473, 7.635761828346577573 ) ) ;
#24451 = LINE ( 'NONE', #36404, #20872 ) ;
#24452 = CARTESIAN_POINT ( 'NONE',  ( 80.45887431248506516, 64.72775385883048216, 3.425340496581062322 ) ) ;
#24453 = CARTESIAN_POINT ( 'NONE',  ( 85.50109956362166486, 1.391598633704343113, -5.555888502831813902 ) ) ;
#24454 = CARTESIAN_POINT ( 'NONE',  ( -9.439742135462632078, 51.66544268451064426, 4.000000000000000000 ) ) ;
#24455 = VERTEX_POINT ( 'NONE', #14038 ) ;
#24456 = DIRECTION ( 'NONE',  ( 1.000000000000000000, 0.000000000000000000, 0.000000000000000000 ) ) ;
#24457 = DIRECTION ( 'NONE',  ( 0.000000000000000000, 1.000000000000000000, 0.000000000000000000 ) ) ;
#24458 = CARTESIAN_POINT ( 'NONE',  ( 4.006432741929322638, -26.93700985481278920, 6.867280401193709416 ) ) ;
#24459 = CARTESIAN_POINT ( 'NONE',  ( 17.03662858313420259, -3.187941445456853096, -2.857527714150005504 ) ) ;
#24460 = CARTESIAN_POINT ( 'NONE',  ( -0.1589752317941719728, -32.41646502212034875, 7.013842709614101167 ) ) ;
#24461 = CARTESIAN_POINT ( 'NONE',  ( 85.87360894986291271, 0.4889004943431661254, 5.985809846730117734 ) ) ;
#24462 = FACE_OUTER_BOUND ( 'NONE', #24075, .T. ) ;
#24463 = ORIENTED_EDGE ( 'NONE', *, *, #23663, .T. ) ;
#24464 = DIRECTION ( 'NONE',  ( 1.000000000000000000, 0.000000000000000000, 0.000000000000000000 ) ) ;
#24465 = CARTESIAN_POINT ( 'NONE',  ( -1.219418532703906877, -27.82788610016705988, 6.894806418505346812 ) ) ;
#24466 = VERTEX_POINT ( 'NONE', #11542 ) ;
#24467 = ORIENTED_EDGE ( 'NONE', *, *, #25583, .T. ) ;
#24469 = CARTESIAN_POINT ( 'NONE',  ( 36.88857704436834695, -3.352795655385050200, 5.910168394248842993 ) ) ;
#24468 = CARTESIAN_POINT ( 'NONE',  ( 79.20700709577712928, 65.89182355360532028, -2.372413575842141853 ) ) ;
#24470 = CARTESIAN_POINT ( 'NONE',  ( 14.72021916802428443, 13.05558383789484900, -2.500000000000000000 ) ) ;
#24471 = VECTOR ( 'NONE', #29247, 1000.000000000000114 ) ;
#24472 = FACE_OUTER_BOUND ( 'NONE', #1020, .T. ) ;
#24473 = VERTEX_POINT ( 'NONE', #5392 ) ;
#24474 = CARTESIAN_POINT ( 'NONE',  ( -1.740649852066194381, -30.20965207207213155, 7.670465701733752972 ) ) ;
#24475 = ADVANCED_FACE ( 'NONE', ( #23906 ), #14441, .F. ) ;
#24476 = ORIENTED_EDGE ( 'NONE', *, *, #30499, .T. ) ;
#24477 = B_SPLINE_CURVE_WITH_KNOTS ( 'NONE', 3,
 ( #33271, #5053, #31400, #22699, #25015, #31197, #18827, #8942, #9349, #3773, #673, #29068, #35266, #18610, #10316, #37554, #22894, #21929, #31002, #21527, #10111, #7236, #2607, #34504, #25778, #32176, #21725, #34307, #16493, #38515, #12448 ),
 .UNSPECIFIED., .F., .F.,
 ( 4, 3, 3, 3, 3, 3, 3, 3, 3, 3, 4 ),
 ( 8.673617379884035472E-19, 2.999644130997694354E-05, 6.002588995694842222E-05, 8.960886084587984992E-05, 0.0001190604700446502720, 0.0001489538463052734552, 0.0001796139255494000775, 0.0002109707048517115509, 0.0002426195318110373352, 0.0002740640997890081898, 0.0002849778069099824680 ),
 .UNSPECIFIED. ) ;
#24479 = EDGE_LOOP ( 'NONE', ( #38654, #32330, #36398, #25963 ) ) ;
#24478 = ORIENTED_EDGE ( 'NONE', *, *, #2459, .T. ) ;
#24480 = CARTESIAN_POINT ( 'NONE',  ( 0.02919540433882696420, -32.53086290775901546, 7.670860738520328681 ) ) ;
#24481 = CARTESIAN_POINT ( 'NONE',  ( 80.27036958223403929, 63.85842528439429344, -3.661914029440275442 ) ) ;
#24482 = DIRECTION ( 'NONE',  ( -0.000000000000000000, -0.000000000000000000, 1.000000000000000000 ) ) ;
#24483 = ORIENTED_EDGE ( 'NONE', *, *, #12306, .F. ) ;
#24485 = CARTESIAN_POINT ( 'NONE',  ( 14.75988012747214206, 13.12337194104200577, 2.499999999999984901 ) ) ;
#24484 = CARTESIAN_POINT ( 'NONE',  ( 22.44694882813763570, 3.194566178373594134, 4.411186854447311845 ) ) ;
#24486 = ORIENTED_EDGE ( 'NONE', *, *, #19642, .F. ) ;
#24487 = EDGE_CURVE ( 'NONE', #15795, #5705, #8252, .T. ) ;
#24488 = CARTESIAN_POINT ( 'NONE',  ( 78.68995612299299580, 66.05828935306207939, -1.022614849746414922 ) ) ;
#24489 = EDGE_CURVE ( 'NONE', #9007, #32259, #40477, .T. ) ;
#24490 = CARTESIAN_POINT ( 'NONE',  ( -0.8241947473075555974, -27.29254761058917822, 7.754798119455333705 ) ) ;
#24491 = ORIENTED_EDGE ( 'NONE', *, *, #18644, .F. ) ;
#24493 = DIRECTION ( 'NONE',  ( 0.000000000000000000, 0.000000000000000000, 1.000000000000000000 ) ) ;
#24492 = CARTESIAN_POINT ( 'NONE',  ( 4.885173765863568107, -28.37948784604718000, 7.661510568013096822 ) ) ;
#24494 = CARTESIAN_POINT ( 'NONE',  ( -1.795519090086910019, -29.40075872605237706, 7.013842709614101167 ) ) ;
#24495 = CARTESIAN_POINT ( 'NONE',  ( 74.30211141138923381, 59.57442121254392475, 3.624554307378899054 ) ) ;
#24496 = EDGE_LOOP ( 'NONE', ( #5555, #2714, #5913, #15145 ) ) ;
#24497 = CARTESIAN_POINT ( 'NONE',  ( 24.14002715383752573, 2.925673756400894110, -3.791870614624193170 ) ) ;
#24498 = ORIENTED_EDGE ( 'NONE', *, *, #8536, .F. ) ;
#24499 = CARTESIAN_POINT ( 'NONE',  ( 0.5185917657260591396, -26.38192185697194603, 7.643333865083957512 ) ) ;
#24500 = EDGE_CURVE ( 'NONE', #29219, #40258, #6688, .T. ) ;
#24501 = CARTESIAN_POINT ( 'NONE',  ( 21.85643539959777115, -1.425092139247138734, 16.06258187428232986 ) ) ;
#24502 = CARTESIAN_POINT ( 'NONE',  ( 1.300000000000000044, 0.5999999999999995337, 4.030609108440248889 ) ) ;
#24503 = EDGE_LOOP ( 'NONE', ( #5437, #20333, #25631, #4458 ) ) ;
#24504 = FACE_OUTER_BOUND ( 'NONE', #4817, .T. ) ;
#24505 = CARTESIAN_POINT ( 'NONE',  ( 81.63129934975499680, 61.79668339569253988, 1.832274617051023569 ) ) ;
#24506 = CARTESIAN_POINT ( 'NONE',  ( 85.21894181876761820, 2.635764410888131959, 2.550537924818469637 ) ) ;
#24507 = DIRECTION ( 'NONE',  ( 0.000000000000000000, 0.000000000000000000, 1.000000000000000000 ) ) ;
#24508 = CIRCLE ( 'NONE', #8059, 0.1000000000000028644 ) ;
#24509 = CARTESIAN_POINT ( 'NONE',  ( 2.715114166433969078, -32.91960704172863927, 6.951256099901589103 ) ) ;
#24510 = ORIENTED_EDGE ( 'NONE', *, *, #35578, .T. ) ;
#24511 = CARTESIAN_POINT ( 'NONE',  ( 28.90011140548632440, -3.472380137462792948, 4.526229835286804892 ) ) ;
#24512 = CARTESIAN_POINT ( 'NONE',  ( -26.87867591359219333, -24.55319635012989110, 6.800000000000000711 ) ) ;
#24513 = CARTESIAN_POINT ( 'NONE',  ( 34.13594578679055758, -3.137541451073295740, -5.534137939634120151 ) ) ;
#24514 = SURFACE_STYLE_USAGE ( .BOTH. , #23699 ) ;
#24515 = B_SPLINE_CURVE_WITH_KNOTS ( 'NONE', 3,
 ( #19274, #31034, #6111, #21562, #19072, #18446, #15973, #18648, #9595, #28747, #27917, #37998, #6725, #28538, #37185, #9798, #37391, #25259, #6315, #18863, #22177, #31639, #22381, #3652, #2841, #150, #40463, #3053, #3460, #24632, #31231, #34748, #24847, #12272, #348, #557, #8975, #31841, #34137, #12891, #34341, #5907, #15361, #31436, #9185, #25455, #16180, #21758, #15573, #28334, #6525, #34945, #28127, #3258, #12485, #25054, #37586, #9383, #21969, #34541, #15782, #12681, #19874, #6918, #35347, #13898, #9997, #4244, #29548, #38198, #22579, #10402 ),
 .UNSPECIFIED., .F., .F.,
 ( 4, 2, 2, 1, 2, 2, 2, 1, 2, 2, 2, 1, 1, 2, 2, 2, 2, 2, 1, 2, 2, 1, 1, 1, 1, 1, 2, 2, 2, 2, 1, 1, 1, 1, 2, 2, 2, 1, 1, 1, 1, 1, 1, 2, 2, 4 ),
 ( 0.000000000000000000, 0.03125000000000544009, 0.04687500000000813932, 0.05468750000000939526, 0.05859375000001094957, 0.06250000000001250389, 0.07812500000001883216, 0.08593750000002287059, 0.08984375000002582656, 0.09375000000002878253, 0.1093750000000364153, 0.1171875000000392741, 0.1210937500000393574, 0.1230468750000377753, 0.1250000000000361655, 0.1562499999999986955, 0.1640624999999889810, 0.1718749999999792666, 0.1874999999999598377, 0.1953124999999492351, 0.2031249999999386324, 0.2187499999999198419, 0.2343749999999010514, 0.2421874999998926692, 0.2460937499998885336, 0.2480468749998864797, 0.2490234374998846478, 0.2499999999998828160, 0.3749999999999580336, 0.4374999999999957256, 0.4687500000000153211, 0.4843750000000243694, 0.4921875000000288658, 0.4960937500000311418, 0.4980468750000315858, 0.5000000000000319744, 0.6249999999999867883, 0.6874999999999652500, 0.7187499999999533706, 0.7343749999999473754, 0.7421874999999458211, 0.7460937499999450440, 0.7480468749999459321, 0.7490234374999463762, 0.7499999999999469313, 1.000000000000000000 ),
 .UNSPECIFIED. ) ;
#24516 = CARTESIAN_POINT ( 'NONE',  ( 5.198039085808181525, -29.69173459304409946, 7.754798119455333705 ) ) ;
#24517 =( BOUNDED_CURVE ( )  B_SPLINE_CURVE ( 3, ( #38839, #4486, #1399, #14124 ),
 .UNSPECIFIED., .F., .T. ) 
 B_SPLINE_CURVE_WITH_KNOTS ( ( 4, 4 ),
 ( 4.708531083176467291, 4.895802057644188743 ),
 .UNSPECIFIED. ) 
 CURVE ( )  GEOMETRIC_REPRESENTATION_ITEM ( )  RATIONAL_B_SPLINE_CURVE ( ( 1.000000000000000000, 0.9970795998553221295, 0.9970795998553221295, 1.000000000000000000 ) ) 
 REPRESENTATION_ITEM ( '' )  );
#24518 = DIRECTION ( 'NONE',  ( 1.000000000000000000, 0.000000000000000000, 0.000000000000000000 ) ) ;
#24519 = CARTESIAN_POINT ( 'NONE',  ( 4.331577083009899631, -31.85530975974228696, 7.785593909369612931 ) ) ;
#24520 = CARTESIAN_POINT ( 'NONE',  ( -70.92837670882107659, 13.87661300689593880, 0.000000000000000000 ) ) ;
#24521 = ORIENTED_EDGE ( 'NONE', *, *, #6142, .T. ) ;
#24522 = CARTESIAN_POINT ( 'NONE',  ( 35.19021350240149104, -1.105041489952045985, 5.467004813264366270 ) ) ;
#24523 = DIRECTION ( 'NONE',  ( 1.000000000000000000, 0.000000000000000000, 0.000000000000000000 ) ) ;
#24524 = CARTESIAN_POINT ( 'NONE',  ( 67.04239844378345481, 57.90286417203066094, -3.997553359131193584 ) ) ;
#24525 = CARTESIAN_POINT ( 'NONE',  ( -71.92837670882107659, -0.7829914368874778541, 9.949874371066204759 ) ) ;
#24526 = DIRECTION ( 'NONE',  ( -0.7660444431189726844, -0.6427876096865458022, -0.000000000000000000 ) ) ;
#24527 = ORIENTED_EDGE ( 'NONE', *, *, #22931, .F. ) ;
#24528 = CARTESIAN_POINT ( 'NONE',  ( -0.4574210171174863948, -32.19744825413003753, 7.703977250142846067 ) ) ;
#24529 = LINE ( 'NONE', #28220, #23274 ) ;
#24530 = CARTESIAN_POINT ( 'NONE',  ( 66.27376694608931018, 57.73522568913554665, 4.000000000000000000 ) ) ;
#24531 = EDGE_LOOP ( 'NONE', ( #39249, #14197, #7491, #39298 ) ) ;
#24532 = FACE_OUTER_BOUND ( 'NONE', #21041, .T. ) ;
#24533 = FACE_OUTER_BOUND ( 'NONE', #10332, .T. ) ;
#24534 = EDGE_LOOP ( 'NONE', ( #26636, #36342, #4546, #35122 ) ) ;
#24535 = CARTESIAN_POINT ( 'NONE',  ( 22.21849618742577093, 5.138564923484444158, 3.154761569516522979 ) ) ;
#24536 = CARTESIAN_POINT ( 'NONE',  ( 78.69038500580381879, 66.05859403932473128, -1.000000000000000000 ) ) ;
#24537 = CARTESIAN_POINT ( 'NONE',  ( 79.46693819636865896, 65.20858797830474884, 3.188730975143406088 ) ) ;
#24538 = CARTESIAN_POINT ( 'NONE',  ( -0.1538752734239677844, -32.41980122938345232, 6.887945620086118659 ) ) ;
#24539 = ORIENTED_EDGE ( 'NONE', *, *, #17053, .T. ) ;
#24540 = CARTESIAN_POINT ( 'NONE',  ( 77.25343114543989032, 63.60010822905027794, -3.597602401604580002 ) ) ;
#24542 = CARTESIAN_POINT ( 'NONE',  ( 14.68628669673910458, -4.762509258086469188, -2.500000000000608402 ) ) ;
#24541 = CARTESIAN_POINT ( 'NONE',  ( 3.872357652763316782, -32.30533874404253680, 7.776484688137383472 ) ) ;
#24543 = CARTESIAN_POINT ( 'NONE',  ( 0.5100408663666432529, -26.38511039769286981, 7.730758795053808363 ) ) ;
#24544 = CARTESIAN_POINT ( 'NONE',  ( 80.41462361967069228, 65.06645272473211605, -3.228380831070266410 ) ) ;
#24545 = CARTESIAN_POINT ( 'NONE',  ( 76.25248298134042102, 64.19605381821563128, 2.844364419910045516 ) ) ;
#24546 = EDGE_LOOP ( 'NONE', ( #16091, #30221, #28892, #19779 ) ) ;
#24547 = EDGE_CURVE ( 'NONE', #35491, #4130, #6201, .T. ) ;
#24548 = EDGE_CURVE ( 'NONE', #27683, #14186, #6616, .T. ) ;
#24549 = AXIS2_PLACEMENT_3D ( 'NONE', #1540, #11179, #10778 ) ;
#24550 = DIRECTION ( 'NONE',  ( -0.000000000000000000, -0.000000000000000000, -1.000000000000000000 ) ) ;
#24551 = EDGE_CURVE ( 'NONE', #39450, #408, #23713, .T. ) ;
#24552 = CARTESIAN_POINT ( 'NONE',  ( 81.49402754981294095, 65.64225023272291537, 1.838010297257003822 ) ) ;
#24555 = ORIENTED_EDGE ( 'NONE', *, *, #13992, .T. ) ;
#24554 = CARTESIAN_POINT ( 'NONE',  ( -1.693090760297530029, -29.35948301055791632, 6.949473656533217358 ) ) ;
#24553 = CARTESIAN_POINT ( 'NONE',  ( 4.261851404573053337, -31.95508217798681017, 6.998987538705435441 ) ) ;
#24556 = CARTESIAN_POINT ( 'NONE',  ( 29.58677136987063960, -0.8116067495284342570, -6.002319972564883699 ) ) ;
#24557 = DIRECTION ( 'NONE',  ( 0.000000000000000000, 1.000000000000000000, 0.000000000000000000 ) ) ;
#24558 = DIRECTION ( 'NONE',  ( -0.000000000000000000, 0.000000000000000000, -1.000000000000000000 ) ) ;
#24559 = CARTESIAN_POINT ( 'NONE',  ( -64.14095127866887935, 35.19432717188715287, 4.537732464557205248 ) ) ;
#24560 = CARTESIAN_POINT ( 'NONE',  ( 26.03637107960420849, 0.8233936766560462361, -4.423249474891364663 ) ) ;
#24561 = VECTOR ( 'NONE', #30895, 1000.000000000000114 ) ;
#24562 = DIRECTION ( 'NONE',  ( 1.000000000000000000, 0.000000000000000000, 0.000000000000000000 ) ) ;
#24563 = CARTESIAN_POINT ( 'NONE',  ( 27.60344192425479193, 81.15229837709949834, 4.000000000000000000 ) ) ;
#24564 = B_SPLINE_CURVE_WITH_KNOTS ( 'NONE', 3,
 ( #32564, #10703, #10908, #4361 ),
 .UNSPECIFIED., .F., .F.,
 ( 4, 4 ),
 ( 9.697399036122160616E-19, 6.391136169898363898E-06 ),
 .UNSPECIFIED. ) ;
#24565 = FACE_OUTER_BOUND ( 'NONE', #2484, .T. ) ;
#24566 = CARTESIAN_POINT ( 'NONE',  ( -1.799471907747695942, -29.53885005966835919, 6.894806418505347700 ) ) ;
#24567 = CARTESIAN_POINT ( 'NONE',  ( 2.124883528784431430, -33.04409396078893479, 6.989977667959444751 ) ) ;
#24568 = CARTESIAN_POINT ( 'NONE',  ( 33.08021759589966848, -0.2095332219197587609, -5.024918305154424836 ) ) ;
#24569 = DIRECTION ( 'NONE',  ( 1.000000000000000000, 0.000000000000000000, 0.000000000000000000 ) ) ;
#24570 = CARTESIAN_POINT ( 'NONE',  ( 70.22075738143423962, -4.730509630324903902, -5.999999999999999112 ) ) ;
#24571 = CARTESIAN_POINT ( 'NONE',  ( 5.042819392577695403, -28.94688871985320588, 7.670860738520327793 ) ) ;
#24572 = CARTESIAN_POINT ( 'NONE',  ( 0.4271750062121888458, -32.81914278374281935, 7.780491323090173772 ) ) ;
#24573 = CARTESIAN_POINT ( 'NONE',  ( -6.248748702180631831, -25.49307895267003587, 6.800000000000000711 ) ) ;
#24574 = B_SPLINE_CURVE_WITH_KNOTS ( 'NONE', 3,
 ( #40400, #37927, #33852, #12205, #5632, #31163, #24776, #30763, #2566, #37320, #21693, #9118, #26401, #19408, #6655, #32585, #4381, #28678, #13419, #31771, #23107, #7247, #9933, #13022, #1095, #35475, #3786, #3986 ),
 .UNSPECIFIED., .F., .F.,
 ( 4, 2, 2, 2, 2, 2, 2, 2, 2, 2, 2, 2, 2, 4 ),
 ( 1.301042606982605321E-18, 0.0002572729306080222961, 0.0005145458612160432911, 0.001029091722432085281, 0.002058183444864175766, 0.003087275167296266686, 0.004116366889728356737, 0.006174550334592495207, 0.008232733779456637146, 0.01234910066918491062, 0.01440728411404905082, 0.01543637583648112092, 0.01595092169769715337, 0.01646546755891318756 ),
 .UNSPECIFIED. ) ;
#24575 = CARTESIAN_POINT ( 'NONE',  ( -64.08758708074093136, 37.77454521956886424, -3.093244392760367667 ) ) ;
#24576 = FACE_OUTER_BOUND ( 'NONE', #5663, .T. ) ;
#24577 = CARTESIAN_POINT ( 'NONE',  ( 24.51166757111680994, 1.776401893265235676, -4.441653616560364171 ) ) ;
#24578 = VERTEX_POINT ( 'NONE', #15261 ) ;
#24579 = ORIENTED_EDGE ( 'NONE', *, *, #8866, .F. ) ;
#24580 = B_SPLINE_CURVE_WITH_KNOTS ( 'NONE', 3,
 ( #34717, #31609, #25021, #37558 ),
 .UNSPECIFIED., .F., .F.,
 ( 4, 4 ),
 ( 0.6850855086804076288, 1.000000000000000000 ),
 .UNSPECIFIED. ) ;
#24581 = CARTESIAN_POINT ( 'NONE',  ( 69.60281991352538000, 59.48300438377392396, -3.944663542062654571 ) ) ;
#24582 = CIRCLE ( 'NONE', #39698, 0.1000000000000028644 ) ;
#24583 = EDGE_LOOP ( 'NONE', ( #30532, #25410, #19292, #33896 ) ) ;
#24584 = CARTESIAN_POINT ( 'NONE',  ( -11.81496944966682960, -21.25669541281728669, 1.000000000000000000 ) ) ;
#24585 = CYLINDRICAL_SURFACE ( 'NONE', #16693, 0.09010775117052735594 ) ;
#24586 = CARTESIAN_POINT ( 'NONE',  ( 2.908949165453299734, -26.39197723079101010, 6.894806418505348589 ) ) ;
#24587 = DIRECTION ( 'NONE',  ( -0.000000000000000000, -0.000000000000000000, 1.000000000000000000 ) ) ;
#24588 = CARTESIAN_POINT ( 'NONE',  ( -36.87867591359218977, -24.55319635012989110, 6.800000000000000711 ) ) ;
#24589 = ORIENTED_EDGE ( 'NONE', *, *, #10907, .F. ) ;
#24590 = CARTESIAN_POINT ( 'NONE',  ( 24.07141319651289280, 3.351886934043508681, 3.193749788468272843 ) ) ;
#24591 = PLANE ( 'NONE',  #31421 ) ;
#24592 = CIRCLE ( 'NONE', #6851, 4.500000000000003553 ) ;
#24593 = ORIENTED_EDGE ( 'NONE', *, *, #20624, .F. ) ;
#24594 = CARTESIAN_POINT ( 'NONE',  ( 80.53617040090057344, 61.82406284986341660, -2.948506306558747347 ) ) ;
#24595 = CARTESIAN_POINT ( 'NONE',  ( 15.67275388389877833, 8.062146399472998937, -3.484635956154243264 ) ) ;
#24596 = CARTESIAN_POINT ( 'NONE',  ( 81.68772813446383907, 64.20773789716569979, -2.952528780688971288 ) ) ;
#24597 = CARTESIAN_POINT ( 'NONE',  ( 78.97528327045988306, 64.81351720955758822, 3.340572457511927773 ) ) ;
#24598 = ORIENTED_EDGE ( 'NONE', *, *, #21424, .F. ) ;
#24599 = DIRECTION ( 'NONE',  ( -0.000000000000000000, -0.000000000000000000, 1.000000000000000000 ) ) ;
#24600 = EDGE_CURVE ( 'NONE', #6472, #5741, #21659, .T. ) ;
#24602 = ORIENTED_EDGE ( 'NONE', *, *, #22966, .F. ) ;
#24601 = CARTESIAN_POINT ( 'NONE',  ( 1.021324086407808585, -26.64985754041175525, 6.700000000000000178 ) ) ;
#24603 = CARTESIAN_POINT ( 'NONE',  ( 21.85643539959775694, 0.06084538214464753347, 12.63034898425695296 ) ) ;
#24604 = ORIENTED_EDGE ( 'NONE', *, *, #17137, .F. ) ;
#24605 = CARTESIAN_POINT ( 'NONE',  ( -79.19778882647081275, 10.32772801069598678, 7.503737277772331460 ) ) ;
#24606 = CARTESIAN_POINT ( 'NONE',  ( -1.799464741694478898, -29.60207515963518077, 7.667456792664608223 ) ) ;
#24607 = CARTESIAN_POINT ( 'NONE',  ( -94.24726447194083789, -65.19654454972992141, 8.800414904976364028 ) ) ;
#24608 = AXIS2_PLACEMENT_3D ( 'NONE', #21886, #37314, #25382 ) ;
#24609 = CARTESIAN_POINT ( 'NONE',  ( 1.719158177631397333, -32.96987838285291872, 7.748216051605118615 ) ) ;
#24610 = CARTESIAN_POINT ( 'NONE',  ( 33.43921609458320177, -3.587388448609353020, -5.336552248008303856 ) ) ;
#24611 = CARTESIAN_POINT ( 'NONE',  ( 36.88807738535138014, -3.351649916613822278, -5.910501343806321195 ) ) ;
#24612 = DIRECTION ( 'NONE',  ( -0.000000000000000000, -0.000000000000000000, 1.000000000000000000 ) ) ;
#24613 = CARTESIAN_POINT ( 'NONE',  ( -64.08758708074093136, 43.61223004741322740, 1.000000000000000000 ) ) ;
#24614 = DIRECTION ( 'NONE',  ( 1.000000000000000000, 0.000000000000000000, 0.000000000000000000 ) ) ;
#24615 = DIRECTION ( 'NONE',  ( 0.000000000000000000, 0.000000000000000000, -1.000000000000000000 ) ) ;
#24616 = CARTESIAN_POINT ( 'NONE',  ( 5.064524549198025305, -29.07729924941551047, 7.774064877406527962 ) ) ;
#24617 = AXIS2_PLACEMENT_3D ( 'NONE', #9068, #34223, #15861 ) ;
#24618 = CARTESIAN_POINT ( 'NONE',  ( 3.908300141282813556, -32.15549264052357614, 7.661510568013099487 ) ) ;
#24619 = CARTESIAN_POINT ( 'NONE',  ( 29.11756219249926758, -3.932895944232090546, -4.208584474947498322 ) ) ;
#24620 = CARTESIAN_POINT ( 'NONE',  ( 26.82849101641929579, 1.498248074508184091, -4.376000038070654519 ) ) ;
#24621 = ORIENTED_EDGE ( 'NONE', *, *, #18405, .F. ) ;
#24622 = ORIENTED_EDGE ( 'NONE', *, *, #15578, .F. ) ;
#24623 = CARTESIAN_POINT ( 'NONE',  ( 67.08924564209870312, 58.23032185317626386, 3.992323350375290403 ) ) ;
#24624 = CARTESIAN_POINT ( 'NONE',  ( 35.79596573831845063, -3.408953143014849196, 5.784744517605735936 ) ) ;
#24625 = EDGE_CURVE ( 'NONE', #9053, #38495, #27614, .T. ) ;
#24626 = CARTESIAN_POINT ( 'NONE',  ( 4.954542941690649016, -30.81756555562317601, 7.785593909369613819 ) ) ;
#24627 = DIRECTION ( 'NONE',  ( -0.000000000000000000, -0.000000000000000000, -1.000000000000000000 ) ) ;
#24628 = CARTESIAN_POINT ( 'NONE',  ( 84.57490107788032674, 3.121871263001978924, -0.4841835102440271710 ) ) ;
#24630 = CARTESIAN_POINT ( 'NONE',  ( 33.46397865298071395, -3.088978469517898340, -5.429261216816389179 ) ) ;
#24629 = DIRECTION ( 'NONE',  ( -0.000000000000000000, -0.000000000000000000, 1.000000000000000000 ) ) ;
#24631 = ORIENTED_EDGE ( 'NONE', *, *, #37720, .F. ) ;
#24632 = CARTESIAN_POINT ( 'NONE',  ( 24.41800086858311758, 2.826335870316004861, 3.825790758725832408 ) ) ;
#24633 = CARTESIAN_POINT ( 'NONE',  ( -0.6763298692248193023, -32.13921067023287037, 7.013842709614101167 ) ) ;
#24634 = ORIENTED_EDGE ( 'NONE', *, *, #27478, .F. ) ;
#24635 = CARTESIAN_POINT ( 'NONE',  ( -69.98161893566610559, -21.12393755324485412, 5.937089484129746353 ) ) ;
#24636 = EDGE_CURVE ( 'NONE', #3709, #37354, #18341, .T. ) ;
#24637 = MECHANICAL_DESIGN_GEOMETRIC_PRESENTATION_REPRESENTATION (  '', ( #30561 ), #37127 ) ;
#24638 = AXIS2_PLACEMENT_3D ( 'NONE', #17202, #10823, #5066 ) ;
#24639 = ORIENTED_EDGE ( 'NONE', *, *, #35999, .T. ) ;
#24640 = ORIENTED_EDGE ( 'NONE', *, *, #36484, .T. ) ;
#24641 = CARTESIAN_POINT ( 'NONE',  ( 80.61389980387333765, 62.62535450461751907, -3.411701596789205926 ) ) ;
#24642 = CARTESIAN_POINT ( 'NONE',  ( -1.560938997313471965, -28.29960244491221033, 6.866770815808350470 ) ) ;
#24643 = CARTESIAN_POINT ( 'NONE',  ( 81.06165217645977350, 61.41816154915743908, 1.973779052375980392 ) ) ;
#24645 = EDGE_LOOP ( 'NONE', ( #23851, #31801, #15543, #27296, #13199 ) ) ;
#24644 = CARTESIAN_POINT ( 'NONE',  ( -1.740904132959085304, -28.93157757802832819, 6.894806418505347700 ) ) ;
#24646 = VECTOR ( 'NONE', #1459, 1000.000000000000114 ) ;
#24647 = CARTESIAN_POINT ( 'NONE',  ( 74.62207946275562165, 60.41194043352551546, -3.856662941142526169 ) ) ;
#24648 = CARTESIAN_POINT ( 'NONE',  ( -0.01240450716718164911, -26.53256281584198817, 7.783750581861600182 ) ) ;
#24649 = EDGE_CURVE ( 'NONE', #20712, #21166, #24529, .T. ) ;
#24651 = CARTESIAN_POINT ( 'NONE',  ( 26.40632256607097972, -4.828918925250113681, 3.355911752401763426 ) ) ;
#24650 = PLANE ( 'NONE',  #8760 ) ;
#24652 = LINE ( 'NONE', #15378, #13027 ) ;
#24653 = CARTESIAN_POINT ( 'NONE',  ( 33.89851005511244608, -5.475126146365266955, 0.2339871931363489144 ) ) ;
#24654 = CARTESIAN_POINT ( 'NONE',  ( 23.14945514779503100, 3.965360163098824664, -3.203264653297140274 ) ) ;
#24655 = EDGE_LOOP ( 'NONE', ( #4302, #29620, #26732, #17364 ) ) ;
#24656 = LINE ( 'NONE', #5312, #3200 ) ;
#24657 = CARTESIAN_POINT ( 'NONE',  ( 24.87384391889476021, -2.282154821806516409, -6.307558310060713325 ) ) ;
#24658 = CARTESIAN_POINT ( 'NONE',  ( -0.04165398999324298329, -32.48973880933039737, 6.894806418505347700 ) ) ;
#24659 = CARTESIAN_POINT ( 'NONE',  ( 81.49799543786487277, 62.67690593247113640, 2.943961322784972356 ) ) ;
#24660 = CARTESIAN_POINT ( 'NONE',  ( 87.94553049950697243, -1.849565313017166535, -3.579236442506480653 ) ) ;
#24661 = CARTESIAN_POINT ( 'NONE',  ( -1.479147532598991122, -25.61012871437631944, 7.013842709614101167 ) ) ;
#24662 = ORIENTED_EDGE ( 'NONE', *, *, #33278, .F. ) ;
#24663 = CARTESIAN_POINT ( 'NONE',  ( 2.879233941065469260, -26.27442913159145021, 7.643192810543819604 ) ) ;
#24664 = CARTESIAN_POINT ( 'NONE',  ( 4.619408797998243443, -31.31332657468931302, 7.785868773668302545 ) ) ;
#24665 = ADVANCED_FACE ( 'NONE', ( #11952 ), #30932, .F. ) ;
#24666 = VECTOR ( 'NONE', #30287, 1000.000000000000000 ) ;
#24667 = VECTOR ( 'NONE', #35796, 1000.000000000000000 ) ;
#24668 = CARTESIAN_POINT ( 'NONE',  ( -5.078675913592192614, -26.64985754041175525, 6.700000000000000178 ) ) ;
#24669 = DIRECTION ( 'NONE',  ( -0.000000000000000000, -0.000000000000000000, 1.000000000000000000 ) ) ;
#24670 = DIRECTION ( 'NONE',  ( -1.000000000000000000, 0.000000000000000000, 0.000000000000000000 ) ) ;
#24671 = DIRECTION ( 'NONE',  ( 0.000000000000000000, 0.000000000000000000, 1.000000000000000000 ) ) ;
#24672 = CARTESIAN_POINT ( 'NONE',  ( 1.855597646007116186, -26.17346053900190839, 6.871394612369935651 ) ) ;
#24673 = ORIENTED_EDGE ( 'NONE', *, *, #30697, .T. ) ;
#24674 = CARTESIAN_POINT ( 'NONE',  ( 36.44665502137046786, -2.355026295696516669, 5.894780000404371556 ) ) ;
#24675 = CARTESIAN_POINT ( 'NONE',  ( -38.97867591359219119, -26.64985754041175525, 6.700000000000000178 ) ) ;
#24676 = EDGE_CURVE ( 'NONE', #29224, #32959, #23785, .T. ) ;
#24677 = CARTESIAN_POINT ( 'NONE',  ( 86.66388813748453401, 1.012732124415782531, -5.000054679117940104 ) ) ;
#24678 = ORIENTED_EDGE ( 'NONE', *, *, #76, .T. ) ;
#24680 = CARTESIAN_POINT ( 'NONE',  ( 25.73464818478049665, 2.638161164068132170, 3.516476401580347133 ) ) ;
#24679 = CARTESIAN_POINT ( 'NONE',  ( 79.95152939680100701, 65.17166210280107919, -3.248659383495581920 ) ) ;
#24681 = CARTESIAN_POINT ( 'NONE',  ( 28.29734904859521194, -2.858939882045380632, 4.622883711642937321 ) ) ;
#24682 = ADVANCED_FACE ( 'NONE', ( #4297 ), #25556, .T. ) ;
#24683 = EDGE_CURVE ( 'NONE', #11306, #29197, #35838, .T. ) ;
#24684 = CARTESIAN_POINT ( 'NONE',  ( -30.87867591359218977, -26.64985754041175525, 6.700000000000000178 ) ) ;
#24685 = CARTESIAN_POINT ( 'NONE',  ( 1.158056475448751454, -26.21346265829786049, 6.894806418505346812 ) ) ;
#24686 = ORIENTED_EDGE ( 'NONE', *, *, #24891, .F. ) ;
#24687 = EDGE_CURVE ( 'NONE', #15530, #31847, #31737, .T. ) ;
#24688 = CARTESIAN_POINT ( 'NONE',  ( -0.2791676774040683928, -26.67527632528762993, 7.501983001166817822 ) ) ;
#24689 = ORIENTED_EDGE ( 'NONE', *, *, #21310, .T. ) ;
#24690 = EDGE_LOOP ( 'NONE', ( #11484, #11534, #31044, #3318, #4919, #15216, #13846, #38555, #364, #10574, #40523, #26065, #2531, #15480, #26640, #3351, #23363, #38256, #1259, #37964, #12990, #10266, #6362, #28821, #5032, #10302, #24319 ) ) ;
#24691 = CARTESIAN_POINT ( 'NONE',  ( 80.84870020435621996, 62.70902516261515558, -3.354617312347319746 ) ) ;
#24692 = CARTESIAN_POINT ( 'NONE',  ( -59.00096901216079459, 28.68090462335501201, -7.030006629679628638 ) ) ;
#24693 = ORIENTED_EDGE ( 'NONE', *, *, #30305, .T. ) ;
#24695 = CARTESIAN_POINT ( 'NONE',  ( 4.377466420158320659, -27.47391912907700373, 7.761597726988851420 ) ) ;
#24694 = CARTESIAN_POINT ( 'NONE',  ( 22.72517738501652573, 2.451757356526896636, 4.776331650956242569 ) ) ;
#24696 = VERTEX_POINT ( 'NONE', #7962 ) ;
#24697 = CARTESIAN_POINT ( 'NONE',  ( 81.87949262442919007, 63.91736224575971193, -2.817575383041753589 ) ) ;
#24698 = CARTESIAN_POINT ( 'NONE',  ( 0.9213240864078056092, -24.55319635012989110, 6.700000000000000178 ) ) ;
#24699 = VECTOR ( 'NONE', #1393, 1000.000000000000114 ) ;
#24700 = CIRCLE ( 'NONE', #37208, 7.744449365083023729 ) ;
#24701 = FACE_OUTER_BOUND ( 'NONE', #28133, .T. ) ;
#24702 = EDGE_CURVE ( 'NONE', #5611, #13148, #29400, .T. ) ;
#24704 = DIRECTION ( 'NONE',  ( -1.273455763949465810E-16, 1.000000000000000000, 0.000000000000000000 ) ) ;
#24703 = CARTESIAN_POINT ( 'NONE',  ( 4.882879936320184910, -28.37336910974825344, 7.692469944509197077 ) ) ;
#24705 = DIRECTION ( 'NONE',  ( 1.000000000000000000, -0.000000000000000000, 0.000000000000000000 ) ) ;
#24706 = CARTESIAN_POINT ( 'NONE',  ( 1.300000000000000044, -0.6000000000000003109, 4.030609108440248889 ) ) ;
#24707 = CARTESIAN_POINT ( 'NONE',  ( 73.59222858082205221, 59.63291812028631966, 3.785151435545463183 ) ) ;
#24708 = CARTESIAN_POINT ( 'NONE',  ( 22.22567626914783290, 3.610917974856977075, -4.269881377294811209 ) ) ;
#24709 = EDGE_LOOP ( 'NONE', ( #7096, #2292, #5511, #16037 ) ) ;
#24710 = VECTOR ( 'NONE', #22377, 1000.000000000000227 ) ;
#24711 = CARTESIAN_POINT ( 'NONE',  ( 21.85643539959776760, -1.092963988217814375, -14.35370713741404458 ) ) ;
#24712 = CARTESIAN_POINT ( 'NONE',  ( -58.92473026143643722, -52.43948302755219260, 2.500000000000000000 ) ) ;
#24713 = ORIENTED_EDGE ( 'NONE', *, *, #10577, .T. ) ;
#24714 = CARTESIAN_POINT ( 'NONE',  ( 80.82569761265843056, 65.28806468744768665, 2.919551171211351548 ) ) ;
#24715 = CARTESIAN_POINT ( 'NONE',  ( 86.68816865751659861, 0.9854590918928021193, 5.166709667929270999 ) ) ;
#24716 = CARTESIAN_POINT ( 'NONE',  ( -2.954197855305039422, -12.43481156997016157, 4.000000000000000000 ) ) ;
#24717 = CARTESIAN_POINT ( 'NONE',  ( 2.724709505007048893, -32.91668746611431118, 6.912143950357347855 ) ) ;
#24718 = CARTESIAN_POINT ( 'NONE',  ( 28.89421610208889746, -3.378331890283770012, 4.594240448401521348 ) ) ;
#24719 = CARTESIAN_POINT ( 'NONE',  ( 1.060668204554370719, -26.12889023809411171, 7.670465701733749420 ) ) ;
#24720 = CARTESIAN_POINT ( 'NONE',  ( 37.04404980618738819, -2.893053985391248251, -5.988017904622426890 ) ) ;
#24721 = CARTESIAN_POINT ( 'NONE',  ( 3.024075050411040078, -32.70932073997259693, 7.139196562012272373 ) ) ;
#24722 = CARTESIAN_POINT ( 'NONE',  ( -1.348441917761853182, -27.85102839191939950, 7.700536657684218689 ) ) ;
#24723 = EDGE_CURVE ( 'NONE', #17087, #24059, #34293, .T. ) ;
#24724 = CARTESIAN_POINT ( 'NONE',  ( 22.01541346579904967, 4.834729283906541220, -3.642368534677343117 ) ) ;
#24725 = VECTOR ( 'NONE', #14716, 1000.000000000000000 ) ;
#24726 = CARTESIAN_POINT ( 'NONE',  ( 1.721493557208823466, -33.06986693911196795, 7.744938106820261403 ) ) ;
#24727 = VECTOR ( 'NONE', #39431, 1000.000000000000000 ) ;
#24728 = ADVANCED_FACE ( 'NONE', ( #32698 ), #9902, .T. ) ;
#24729 = ORIENTED_EDGE ( 'NONE', *, *, #40, .T. ) ;
#24730 = CARTESIAN_POINT ( 'NONE',  ( 32.00271079493634119, 0.1412851624054302091, 4.903334175247278992 ) ) ;
#24731 = DIRECTION ( 'NONE',  ( -0.000000000000000000, -1.000000000000000000, -0.000000000000000000 ) ) ;
#24732 = ORIENTED_EDGE ( 'NONE', *, *, #23184, .F. ) ;
#24733 = CARTESIAN_POINT ( 'NONE',  ( 66.97838688114072170, 58.07970146089488850, -3.998003515188802037 ) ) ;
#24734 = CARTESIAN_POINT ( 'NONE',  ( 4.300627460203361174, -31.91262744306316179, 7.753200566781576875 ) ) ;
#24735 = AXIS2_PLACEMENT_3D ( 'NONE', #3379, #12803, #40191 ) ;
#24736 = EDGE_CURVE ( 'NONE', #32517, #19029, #35600, .T. ) ;
#24737 = EDGE_LOOP ( 'NONE', ( #40217, #25095, #30875, #30320 ) ) ;
#24738 = CARTESIAN_POINT ( 'NONE',  ( 87.74971820199947103, -0.2069237406511922894, -3.800190472810109021 ) ) ;
#24739 = CARTESIAN_POINT ( 'NONE',  ( -78.94357670570525443, -6.586313634853134147, -6.037452900681159917 ) ) ;
#24740 = CARTESIAN_POINT ( 'NONE',  ( 19.21387499064117321, 6.947138423917541772, 3.205187900248952726 ) ) ;
#24741 = VERTEX_POINT ( 'NONE', #241 ) ;
#24742 = DIRECTION ( 'NONE',  ( 0.9999026450364576490, 0.01395351027862084051, 0.000000000000000000 ) ) ;
#24743 = FACE_OUTER_BOUND ( 'NONE', #21214, .T. ) ;
#24744 = VERTEX_POINT ( 'NONE', #6624 ) ;
#24745 = CARTESIAN_POINT ( 'NONE',  ( 22.01556798311525753, 5.489466605003165967, 3.155826305233227824 ) ) ;
#24746 = CARTESIAN_POINT ( 'NONE',  ( 81.73765358980274698, 61.68994590043247683, -1.132734665583632117 ) ) ;
#24747 = CARTESIAN_POINT ( 'NONE',  ( 78.69119446862563905, 66.01295734309309182, 1.592560325354587913 ) ) ;
#24748 = CARTESIAN_POINT ( 'NONE',  ( -63.96695182803188828, 19.27020452292899222, 8.800414904976364028 ) ) ;
#24749 = ORIENTED_EDGE ( 'NONE', *, *, #17117, .T. ) ;
#24750 = CARTESIAN_POINT ( 'NONE',  ( 77.82713238777952824, 60.98268764611934500, -3.435658781985014176 ) ) ;
#24751 = B_SPLINE_CURVE_WITH_KNOTS ( 'NONE', 3,
 ( #18464, #25472, #37807, #34563, #21577, #19088, #24865, #37405, #40698, #3471 ),
 .UNSPECIFIED., .F., .F.,
 ( 4, 2, 2, 2, 4 ),
 ( 2.168404344971008868E-19, 8.504419282386946875E-05, 0.0001700883856477387207, 0.0003401767712954767908, 0.0006803535425909649657 ),
 .UNSPECIFIED. ) ;
#24753 = CARTESIAN_POINT ( 'NONE',  ( 1.826415646469069731, -26.07219983930859897, 7.750000000000000888 ) ) ;
#24752 = DIRECTION ( 'NONE',  ( 0.7660444431189770143, 0.6427876096865404731, -0.000000000000000000 ) ) ;
#24754 = CARTESIAN_POINT ( 'NONE',  ( 0.5944372483576262356, -26.35483013752983794, 7.785172627573962778 ) ) ;
#24755 = CARTESIAN_POINT ( 'NONE',  ( 80.13372729538053818, 65.27601544180762971, -3.162824939344919262 ) ) ;
#24756 = CARTESIAN_POINT ( 'NONE',  ( 76.46949791074166569, 63.77707083977482228, 3.308002540424330284 ) ) ;
#24757 = VERTEX_POINT ( 'NONE', #19171 ) ;
#24758 = CARTESIAN_POINT ( 'NONE',  ( 4.740217150655367639, -31.30470820734161563, 7.640616322432097540 ) ) ;
#24759 = EDGE_LOOP ( 'NONE', ( #20335, #11183, #1767, #24385 ) ) ;
#24760 = CARTESIAN_POINT ( 'NONE',  ( -58.72892591012804075, 29.68775822799332076, 5.573531433662443746 ) ) ;
#24761 = CARTESIAN_POINT ( 'NONE',  ( 81.23565735523312981, 65.86993722804051288, 1.793694987645560568 ) ) ;
#24762 =( BOUNDED_CURVE ( )  B_SPLINE_CURVE ( 3, ( #8843, #30278, #27181, #21429 ),
 .UNSPECIFIED., .F., .T. ) 
 B_SPLINE_CURVE_WITH_KNOTS ( ( 4, 4 ),
 ( 1.381924640371168467, 1.574767692156076926 ),
 .UNSPECIFIED. ) 
 CURVE ( )  GEOMETRIC_REPRESENTATION_ITEM ( )  RATIONAL_B_SPLINE_CURVE ( ( 1.000000000000000000, 0.9969033633783032089, 0.9969033633783032089, 1.000000000000000000 ) ) 
 REPRESENTATION_ITEM ( '' )  );
#24764 = CYLINDRICAL_SURFACE ( 'NONE', #16337, 0.09010775117052907679 ) ;
#24763 = DIRECTION ( 'NONE',  ( 1.000000000000000000, 0.000000000000000000, 0.000000000000000000 ) ) ;
#24765 = CARTESIAN_POINT ( 'NONE',  ( 31.71671097226645131, -1.585248588153130855, -6.002663613118158992 ) ) ;
#24766 = VECTOR ( 'NONE', #6480, 1000.000000000000114 ) ;
#24767 = CARTESIAN_POINT ( 'NONE',  ( -1.422348494510240480, -31.15059581268885580, 6.961115707816239784 ) ) ;
#24768 = CARTESIAN_POINT ( 'NONE',  ( -63.58520484588294153, 35.72026407271188475, -6.999999999999999112 ) ) ;
#24769 = CARTESIAN_POINT ( 'NONE',  ( 1.537640963180244347, -33.06615115872732247, 6.887547729233690852 ) ) ;
#24770 = CARTESIAN_POINT ( 'NONE',  ( 26.02598813970154623, 0.8351557787169782143, -4.424076136248003444 ) ) ;
#24771 = AXIS2_PLACEMENT_3D ( 'NONE', #28572, #18111, #21432 ) ;
#24772 = CARTESIAN_POINT ( 'NONE',  ( 3.021324086407803478, -26.64985754041175525, 6.700000000000000178 ) ) ;
#24774 = EDGE_CURVE ( 'NONE', #18417, #5658, #3551, .T. ) ;
#24773 = ORIENTED_EDGE ( 'NONE', *, *, #22977, .F. ) ;
#24775 = DIRECTION ( 'NONE',  ( 1.165409145176970240E-16, -1.000000000000000000, 0.000000000000000000 ) ) ;
#24776 = CARTESIAN_POINT ( 'NONE',  ( 80.71272553023811724, 61.13839519651874355, 1.655401764483099614 ) ) ;
#24777 = DIRECTION ( 'NONE',  ( 0.000000000000000000, 0.000000000000000000, 1.000000000000000000 ) ) ;
#24778 = CARTESIAN_POINT ( 'NONE',  ( 32.03508869243609070, 0.1963088816440640705, -4.819211608773691147 ) ) ;
#24779 = CARTESIAN_POINT ( 'NONE',  ( 75.38950776596149694, 59.47909021198979218, -3.241469810694041609 ) ) ;
#24780 = FACE_OUTER_BOUND ( 'NONE', #16276, .T. ) ;
#24781 = CARTESIAN_POINT ( 'NONE',  ( -89.20959394718985891, -30.20828278875847062, 6.894806418505347700 ) ) ;
#24782 = CARTESIAN_POINT ( 'NONE',  ( 0.4016364682254440766, -32.81725445528589091, 7.766640943994648438 ) ) ;
#24783 = B_SPLINE_CURVE_WITH_KNOTS ( 'NONE', 3,
 ( #15149, #14946, #3045, #40262, #9178, #31026, #12046, #15567, #28121, #27512, #24626, #24422, #8964, #37178, #5899, #21553, #11765, #7333, #30333 ),
 .UNSPECIFIED., .F., .F.,
 ( 4, 3, 3, 3, 3, 3, 4 ),
 ( 0.000000000000000000, 2.546128104244680068E-05, 5.711050680483513924E-05, 8.113074941675454152E-05, 0.0001053129305727007356, 0.0001360598016347043700, 0.0001612931755701971497 ),
 .UNSPECIFIED. ) ;
#24784 = FACE_OUTER_BOUND ( 'NONE', #35197, .T. ) ;
#24785 = CARTESIAN_POINT ( 'NONE',  ( 5.098113783035356228, -29.69476113458859601, 6.863904403958576594 ) ) ;
#24786 = CARTESIAN_POINT ( 'NONE',  ( 86.43572624768425783, -0.5192074800720990480, -5.777013305174518720 ) ) ;
#24787 = CARTESIAN_POINT ( 'NONE',  ( 2.829942967996462944, -26.36304532024056968, 7.680992449362121555 ) ) ;
#24788 = CARTESIAN_POINT ( 'NONE',  ( 21.81178528484681323, 1.722486916688236835, -6.429858153412585153 ) ) ;
#24789 = EDGE_CURVE ( 'NONE', #10043, #3556, #22479, .T. ) ;
#24790 = CARTESIAN_POINT ( 'NONE',  ( -12.99139449055068241, -10.90558813203967148, -2.500000000000000000 ) ) ;
#24791 = ORIENTED_EDGE ( 'NONE', *, *, #13402, .F. ) ;
#24792 = CARTESIAN_POINT ( 'NONE',  ( -2.485163400083383323, -30.43163963246801984, 7.754798119455333705 ) ) ;
#24793 = CARTESIAN_POINT ( 'NONE',  ( 69.29807964942261833, 58.55307042757259950, -3.976370928559293638 ) ) ;
#24794 = EDGE_CURVE ( 'NONE', #18006, #30906, #9447, .T. ) ;
#24795 = EDGE_CURVE ( 'NONE', #25345, #23979, #15487, .T. ) ;
#24796 = VERTEX_POINT ( 'NONE', #24006 ) ;
#24797 = CARTESIAN_POINT ( 'NONE',  ( 87.32189673294487875, -1.771757446153727322, -4.160567758657673920 ) ) ;
#24798 = EDGE_CURVE ( 'NONE', #30864, #34912, #21309, .T. ) ;
#24799 = DIRECTION ( 'NONE',  ( -0.000000000000000000, -1.000000000000000000, -0.000000000000000000 ) ) ;
#24800 = AXIS2_PLACEMENT_3D ( 'NONE', #36780, #8147, #8765 ) ;
#24801 = CARTESIAN_POINT ( 'NONE',  ( 4.851634552394991751, -30.84651091276440482, 7.754798119455333705 ) ) ;
#24802 = AXIS2_PLACEMENT_3D ( 'NONE', #31008, #12457, #15753 ) ;
#24803 = AXIS2_PLACEMENT_3D ( 'NONE', #4483, #17007, #20300 ) ;
#24804 = CARTESIAN_POINT ( 'NONE',  ( 5.033830403340459725, -30.23945351880105648, 7.782034975670476307 ) ) ;
#24805 = ORIENTED_EDGE ( 'NONE', *, *, #24167, .F. ) ;
#24806 = CARTESIAN_POINT ( 'NONE',  ( 22.38241241717832608, 4.945970055669522303, 3.038707014936568029 ) ) ;
#24807 = CARTESIAN_POINT ( 'NONE',  ( 22.20101428496644402, -3.080863327041267752, 3.573976167030509021 ) ) ;
#24808 = ORIENTED_EDGE ( 'NONE', *, *, #6847, .F. ) ;
#24809 = CARTESIAN_POINT ( 'NONE',  ( 79.24578529683977024, 64.32976145010148628, -3.589982250315052692 ) ) ;
#24810 = CARTESIAN_POINT ( 'NONE',  ( -1.676799063830336056, -29.96313308435724210, 6.997764925645183709 ) ) ;
#24811 = CARTESIAN_POINT ( 'NONE',  ( 78.89436432227893192, 66.15509128278823425, -1.313329331391854371 ) ) ;
#24812 = CARTESIAN_POINT ( 'NONE',  ( 79.66447349905094200, 63.54298318056227401, 3.741985197832887522 ) ) ;
#24813 = ORIENTED_EDGE ( 'NONE', *, *, #31116, .T. ) ;
#24814 = CARTESIAN_POINT ( 'NONE',  ( -64.08758708074093136, 38.13199975834322686, 3.043809435734689206 ) ) ;
#24815 = CARTESIAN_POINT ( 'NONE',  ( 2.896981936218417708, -32.75240845689362601, 7.703977250142848732 ) ) ;
#24816 = CARTESIAN_POINT ( 'NONE',  ( 21.85643539959779247, -11.31796667593991401, 0.7532527802845886411 ) ) ;
#24817 = EDGE_LOOP ( 'NONE', ( #11503, #35215, #760, #2081 ) ) ;
#24818 = CARTESIAN_POINT ( 'NONE',  ( -72.95667172690721713, 3.805589226921943791, 9.852272255005502188 ) ) ;
#24819 = CARTESIAN_POINT ( 'NONE',  ( 36.61039225523681040, -3.503863859546586745, 5.830862488035224445 ) ) ;
#24820 = AXIS2_PLACEMENT_3D ( 'NONE', #21372, #23827, #30433 ) ;
#24821 = CARTESIAN_POINT ( 'NONE',  ( 1.670112593087247577, -32.96979536792423460, 7.782167645815905033 ) ) ;
#24822 = CARTESIAN_POINT ( 'NONE',  ( 29.49012604331536025, 1.222189331997720618, -4.216495775964309800 ) ) ;
#24823 = CARTESIAN_POINT ( 'NONE',  ( 3.720465652270369183, -32.30476016926337479, 6.949473656533220023 ) ) ;
#24824 = CARTESIAN_POINT ( 'NONE',  ( 15.57083851783882444, 11.09451738654227171, 2.625278935214002018 ) ) ;
#24825 = FACE_OUTER_BOUND ( 'NONE', #28532, .T. ) ;
#24826 = CARTESIAN_POINT ( 'NONE',  ( 29.72221670659310178, -3.784665454809892360, 4.453569354697067162 ) ) ;
#24827 = CARTESIAN_POINT ( 'NONE',  ( 14.62586668347152496, -4.707709139745178462, 2.499999999999999556 ) ) ;
#24828 = CARTESIAN_POINT ( 'NONE',  ( 5.047799653463134639, -28.97418023640373974, 7.763628509615286610 ) ) ;
#24829 = VECTOR ( 'NONE', #14442, 1000.000000000000000 ) ;
#24830 = CARTESIAN_POINT ( 'NONE',  ( 3.913265336722258514, -32.15124441476239525, 7.692469944509199742 ) ) ;
#24831 = CARTESIAN_POINT ( 'NONE',  ( 21.73802686818168439, 0.3490801365243696996, -8.770837729082545664 ) ) ;
#24832 = CARTESIAN_POINT ( 'NONE',  ( 36.75577213747256167, -1.983309010297000130, -5.827804699962920054 ) ) ;
#24833 = CARTESIAN_POINT ( 'NONE',  ( 24.49910823378019842, 2.769216814238300017, -3.858631695855636590 ) ) ;
#24834 = VERTEX_POINT ( 'NONE', #37187 ) ;
#24835 = CARTESIAN_POINT ( 'NONE',  ( 67.50273067437429120, 58.00668225682344570, 3.993945454764282310 ) ) ;
#24836 = CARTESIAN_POINT ( 'NONE',  ( 36.14935728473858489, -3.245521681047676577, 5.848379498429883583 ) ) ;
#24837 = CARTESIAN_POINT ( 'NONE',  ( -12.99139449055068241, -10.90558813203967148, -2.500000000000000000 ) ) ;
#24838 = EDGE_CURVE ( 'NONE', #5805, #422, #11622, .T. ) ;
#24839 = CARTESIAN_POINT ( 'NONE',  ( -0.2487487021806331078, -26.64985754041175525, 6.700000000000000178 ) ) ;
#24840 = CARTESIAN_POINT ( 'NONE',  ( 88.76896161869186130, -1.545781173472005943, 2.128395682968124092 ) ) ;
#24841 = EDGE_CURVE ( 'NONE', #17923, #20627, #11426, .T. ) ;
#24843 = CARTESIAN_POINT ( 'NONE',  ( 22.47913989204488061, 3.956929407484332195, 2.823518125048976923 ) ) ;
#24842 = LINE ( 'NONE', #24217, #8341 ) ;
#24844 = FACE_OUTER_BOUND ( 'NONE', #30338, .T. ) ;
#24845 = AXIS2_PLACEMENT_3D ( 'NONE', #8326, #39844, #1989 ) ;
#24846 = EDGE_LOOP ( 'NONE', ( #38464, #36148, #10035, #8919 ) ) ;
#24847 = CARTESIAN_POINT ( 'NONE',  ( 24.47171158531734392, 2.787145917774926929, 3.848838691513146948 ) ) ;
#24848 = CARTESIAN_POINT ( 'NONE',  ( -7.890026461918810519, -29.56993018339340651, -6.000000000000000000 ) ) ;
#24849 = VERTEX_POINT ( 'NONE', #33928 ) ;
#24850 = CARTESIAN_POINT ( 'NONE',  ( -30.87867591359218977, -26.64985754041175525, 6.700000000000000178 ) ) ;
#24851 = AXIS2_PLACEMENT_3D ( 'NONE', #33897, #2611, #24401 ) ;
#24852 = VERTEX_POINT ( 'NONE', #30831 ) ;
#24853 = CARTESIAN_POINT ( 'NONE',  ( 80.95922275190012840, 61.28229338972344920, -1.760837461004916893 ) ) ;
#24854 = CARTESIAN_POINT ( 'NONE',  ( 81.23507808130548824, 61.62583295638711434, -2.125034277891705070 ) ) ;
#24855 = DIRECTION ( 'NONE',  ( -1.000000000000000000, -0.000000000000000000, -0.000000000000000000 ) ) ;
#24856 = AXIS2_PLACEMENT_3D ( 'NONE', #37661, #6190, #34626 ) ;
#24857 = CARTESIAN_POINT ( 'NONE',  ( 81.03586710326727882, 61.41218721227320998, 1.994058748902159062 ) ) ;
#24859 = VERTEX_POINT ( 'NONE', #8766 ) ;
#24858 = FACE_OUTER_BOUND ( 'NONE', #22488, .T. ) ;
#24860 = DIRECTION ( 'NONE',  ( -1.000000000000000000, 0.000000000000000000, 0.000000000000000000 ) ) ;
#24861 = CARTESIAN_POINT ( 'NONE',  ( -56.59682361629209879, 30.63869417066593925, 3.015094993620162978 ) ) ;
#24863 = CARTESIAN_POINT ( 'NONE',  ( -44.23414840393349579, -30.38627270959228710, 6.000000000000000000 ) ) ;
#24862 = LINE ( 'NONE', #37402, #38998 ) ;
#24864 = LINE ( 'NONE', #37404, #17578 ) ;
#24865 = CARTESIAN_POINT ( 'NONE',  ( -54.93018042890351182, 31.40271527509257865, 1.217153544005994181 ) ) ;
#24866 = CARTESIAN_POINT ( 'NONE',  ( 24.67792551878487117, 2.994442889702503940, -3.478280344776563560 ) ) ;
#24867 = VERTEX_POINT ( 'NONE', #24221 ) ;
#24868 = CARTESIAN_POINT ( 'NONE',  ( 5.025435985552490159, -30.27990892530747047, 7.754798119455333705 ) ) ;
#24869 = EDGE_CURVE ( 'NONE', #25800, #27373, #11440, .T. ) ;
#24870 = CARTESIAN_POINT ( 'NONE',  ( 24.99136039731803294, -2.601164552868876267, 6.036718378868273227 ) ) ;
#24871 = CARTESIAN_POINT ( 'NONE',  ( -80.58693949271321344, -5.694496834616916026, -2.621342879253132807 ) ) ;
#24872 = CARTESIAN_POINT ( 'NONE',  ( 5.008335689530277968, -30.35575962765878089, 6.911401339314956260 ) ) ;
#24873 = CARTESIAN_POINT ( 'NONE',  ( 81.15569957775159082, 61.29889919928260156, 1.113695828830617796 ) ) ;
#24874 = CARTESIAN_POINT ( 'NONE',  ( 85.94684271633954609, 0.9790069142357779031, 5.868308835085408681 ) ) ;
#24875 = CARTESIAN_POINT ( 'NONE',  ( 18.29979634815094869, 8.276402169532444120, 2.983512989312166130 ) ) ;
#24876 = ORIENTED_EDGE ( 'NONE', *, *, #8051, .F. ) ;
#24877 = VECTOR ( 'NONE', #33443, 1000.000000000000000 ) ;
#24878 = CARTESIAN_POINT ( 'NONE',  ( -64.58677651244121876, 34.69729445092669806, -5.982681548040577724 ) ) ;
#24879 = DIRECTION ( 'NONE',  ( 0.6427876096865425826, -0.7660444431189752379, 0.000000000000000000 ) ) ;
#24880 = ORIENTED_EDGE ( 'NONE', *, *, #3947, .F. ) ;
#24881 = EDGE_CURVE ( 'NONE', #40670, #10861, #3582, .T. ) ;
#24882 = CARTESIAN_POINT ( 'NONE',  ( -70.92837670882107659, 13.87661300689599742, 0.000000000000000000 ) ) ;
#24883 = DIRECTION ( 'NONE',  ( -0.000000000000000000, -0.000000000000000000, -1.000000000000000000 ) ) ;
#24884 = CARTESIAN_POINT ( 'NONE',  ( 25.29478483175916637, 1.731669011002412661, -4.154260948315759983 ) ) ;
#24885 = CARTESIAN_POINT ( 'NONE',  ( 85.57577930415899914, 1.015208198401525541, 5.782835925834406865 ) ) ;
#24886 = CARTESIAN_POINT ( 'NONE',  ( 1.881295483120765111, -26.17473677672775878, 6.887945620086118659 ) ) ;
#24887 = ORIENTED_EDGE ( 'NONE', *, *, #23021, .T. ) ;
#24888 = CARTESIAN_POINT ( 'NONE',  ( 37.04356103307386405, -2.892718132023992528, 5.987941619757027212 ) ) ;
#24889 = AXIS2_PLACEMENT_3D ( 'NONE', #35527, #10776, #4820 ) ;
#24890 = CARTESIAN_POINT ( 'NONE',  ( 87.74221684178165503, -0.1984978568185522818, 3.841619981418926244 ) ) ;
#24891 = EDGE_CURVE ( 'NONE', #28300, #10739, #7612, .T. ) ;
#24892 = ORIENTED_EDGE ( 'NONE', *, *, #23536, .T. ) ;
#24894 = CARTESIAN_POINT ( 'NONE',  ( -61.24591834330252027, -49.47158280949359010, 2.500000000000000000 ) ) ;
#24893 = CARTESIAN_POINT ( 'NONE',  ( 80.35608454708172133, 64.67152608030554006, -3.471690071579495829 ) ) ;
#24895 = CARTESIAN_POINT ( 'NONE',  ( 18.19526664008617800, -2.845337040135758500, 3.046209432008794238 ) ) ;
#24896 = CARTESIAN_POINT ( 'NONE',  ( -1.036828849638991690, -31.59861137850023738, 7.386948897581449458 ) ) ;
#24897 = CARTESIAN_POINT ( 'NONE',  ( -70.92837670882107659, 0.7293679304675899644, 0.000000000000000000 ) ) ;
#24898 = ORIENTED_EDGE ( 'NONE', *, *, #22801, .F. ) ;
#24899 = CARTESIAN_POINT ( 'NONE',  ( 27.17156870755912124, -4.509646516228694502, -3.611948544634925096 ) ) ;
#24900 = ORIENTED_EDGE ( 'NONE', *, *, #1938, .T. ) ;
#24901 = ORIENTED_EDGE ( 'NONE', *, *, #29347, .T. ) ;
#24902 = CONICAL_SURFACE ( 'NONE', #30845, 3.961287410364449979, 0.08726646259971682085 ) ;
#24903 = CARTESIAN_POINT ( 'NONE',  ( 78.72446908900997187, 66.04077733106291248, -1.541060042019481990 ) ) ;
#24904 = AXIS2_PLACEMENT_3D ( 'NONE', #22551, #721, #13671 ) ;
#24905 = CARTESIAN_POINT ( 'NONE',  ( -1.506684114051581869, -28.44091511309124343, 7.693875151218752428 ) ) ;
#24906 = ORIENTED_EDGE ( 'NONE', *, *, #30791, .F. ) ;
#24908 = CARTESIAN_POINT ( 'NONE',  ( 35.96429208010314227, -1.440254987971542500, 5.601774252719624592 ) ) ;
#24907 = CARTESIAN_POINT ( 'NONE',  ( 22.45948225295538592, 3.011618625913302871, 4.542466585459654205 ) ) ;
#24909 = ORIENTED_EDGE ( 'NONE', *, *, #13724, .T. ) ;
#24910 = CARTESIAN_POINT ( 'NONE',  ( 81.59006957456230680, 61.61658442860579044, -1.498428902123934980 ) ) ;
#24911 = CARTESIAN_POINT ( 'NONE',  ( 4.749222104228042696, -31.28883197486738510, 7.700536657684216024 ) ) ;
#24913 = CARTESIAN_POINT ( 'NONE',  ( 85.60328218737365091, 2.204055066975417976, -3.382088663712862431 ) ) ;
#24912 = CARTESIAN_POINT ( 'NONE',  ( -70.05495661583778144, -0.2787455909213534810, 5.936304882227261714 ) ) ;
#24914 = FACE_OUTER_BOUND ( 'NONE', #18127, .T. ) ;
#24915 = CARTESIAN_POINT ( 'NONE',  ( 0.5949730329236684323, -26.25663028810755861, 7.776484688137383472 ) ) ;
#24916 = CARTESIAN_POINT ( 'NONE',  ( 72.61754431144450450, 61.86111285056382059, 3.476886323448412419 ) ) ;
#24917 = EDGE_CURVE ( 'NONE', #28596, #16444, #12488, .T. ) ;
#24918 = CARTESIAN_POINT ( 'NONE',  ( 22.84217460911794007, 3.239333396839658707, -4.097155120049850829 ) ) ;
#24919 = ORIENTED_EDGE ( 'NONE', *, *, #3127, .F. ) ;
#24920 = AXIS2_PLACEMENT_3D ( 'NONE', #12153, #18534, #34225 ) ;
#24921 = CARTESIAN_POINT ( 'NONE',  ( 21.85643539959774273, 11.87292600555486466, 1.968928953175947072 ) ) ;
#24922 = CARTESIAN_POINT ( 'NONE',  ( 16.10603109340134509, 15.28195951422513232, -3.145749391471717615 ) ) ;
#24923 = ORIENTED_EDGE ( 'NONE', *, *, #23703, .T. ) ;
#24924 = CARTESIAN_POINT ( 'NONE',  ( 1.651251297819358754, -25.49307895267003587, 6.700000000000000178 ) ) ;
#24925 = CARTESIAN_POINT ( 'NONE',  ( 80.71932482181554747, 65.23126254902237520, 3.019969592843124939 ) ) ;
#24926 = CARTESIAN_POINT ( 'NONE',  ( 88.42181306311033495, -0.9618525881974497871, -1.725133412809377598 ) ) ;
#24927 = VERTEX_POINT ( 'NONE', #34751 ) ;
#24928 = EDGE_CURVE ( 'NONE', #20545, #15995, #4238, .T. ) ;
#24929 = CARTESIAN_POINT ( 'NONE',  ( -0.9128197825508301833, -27.39481314169073300, 7.635761828346577573 ) ) ;
#24930 = ORIENTED_EDGE ( 'NONE', *, *, #37373, .F. ) ;
#24931 = CARTESIAN_POINT ( 'NONE',  ( 23.84193253497030440, -2.761854320939544749, 3.927508210036176450 ) ) ;
#24932 = EDGE_CURVE ( 'NONE', #23657, #9954, #18649, .T. ) ;
#24933 = CARTESIAN_POINT ( 'NONE',  ( 1.300000000000000044, -0.6000000000000003109, 4.030609108440248889 ) ) ;
#24934 = CIRCLE ( 'NONE', #7839, 27.95745752244933158 ) ;
#24935 = CARTESIAN_POINT ( 'NONE',  ( 21.30795695682776625, 3.457868135880847849, -3.532020036634553328 ) ) ;
#24936 = CARTESIAN_POINT ( 'NONE',  ( 5.099675413223700993, -29.64036099912623712, 7.784476445165074310 ) ) ;
#24937 = CARTESIAN_POINT ( 'NONE',  ( 0.9716734364680117420, -32.99315042889409000, 7.753200566781576875 ) ) ;
#24938 = ORIENTED_EDGE ( 'NONE', *, *, #34007, .T. ) ;
#24939 = DIRECTION ( 'NONE',  ( -0.9267318687906771491, 0.3757233601570964532, 0.000000000000000000 ) ) ;
#24940 = EDGE_CURVE ( 'NONE', #19582, #29208, #31640, .T. ) ;
#24941 = ORIENTED_EDGE ( 'NONE', *, *, #33464, .F. ) ;
#24942 = EDGE_LOOP ( 'NONE', ( #34922, #11900 ) ) ;
#24943 = CARTESIAN_POINT ( 'NONE',  ( 33.11218242963668956, -0.1536849661985871807, 4.945614694268311240 ) ) ;
#24944 = CARTESIAN_POINT ( 'NONE',  ( -80.92837670882107659, 2.429809908903242555, 15.50000000000000000 ) ) ;
#24945 = ORIENTED_EDGE ( 'NONE', *, *, #543, .F. ) ;
#24946 = CARTESIAN_POINT ( 'NONE',  ( 66.58549141467136678, 57.79032289594774596, -3.999530551061463157 ) ) ;
#24947 = CIRCLE ( 'NONE', #12447, 7.538952224936807056 ) ;
#24948 = ORIENTED_EDGE ( 'NONE', *, *, #3566, .F. ) ;
#24949 = CARTESIAN_POINT ( 'NONE',  ( -57.16504416091206053, 33.41445838748276742, 3.999999999999999112 ) ) ;
#24950 = CYLINDRICAL_SURFACE ( 'NONE', #12142, 6.681288188914807691 ) ;
#24951 = CARTESIAN_POINT ( 'NONE',  ( -26.87867591359219333, -26.64985754041175525, 6.700000000000000178 ) ) ;
#24952 = CARTESIAN_POINT ( 'NONE',  ( -24.87867591359218977, -24.55319635012989110, 6.700000000000000178 ) ) ;
#24953 = VERTEX_POINT ( 'NONE', #350 ) ;
#24954 = CARTESIAN_POINT ( 'NONE',  ( 24.32733003514473680, 3.133098549323304116, 3.417467526496732688 ) ) ;
#24955 = CARTESIAN_POINT ( 'NONE',  ( 78.69036185089562707, 66.05857758962513060, -1.005837412005794906 ) ) ;
#24956 = ADVANCED_FACE ( 'NONE', ( #3259 ), #9469, .T. ) ;
#24957 = CARTESIAN_POINT ( 'NONE',  ( 79.31717123896756050, 65.40625759565881481, 2.968223699503263369 ) ) ;
#24958 = CIRCLE ( 'NONE', #30201, 0.1000000000000028644 ) ;
#24959 = CARTESIAN_POINT ( 'NONE',  ( -70.92837670224925262, -21.78291075600659354, 3.999987187540717137 ) ) ;
#24960 = ORIENTED_EDGE ( 'NONE', *, *, #302, .T. ) ;
#24961 = CARTESIAN_POINT ( 'NONE',  ( 75.88202180556027088, 63.57356190189722156, -3.253266109296521602 ) ) ;
#24963 = DIRECTION ( 'NONE',  ( -0.000000000000000000, -0.000000000000000000, 1.000000000000000000 ) ) ;
#24962 = CARTESIAN_POINT ( 'NONE',  ( 2.350580150463965623, -26.13084565137115689, 6.883108633650832253 ) ) ;
#24964 = CARTESIAN_POINT ( 'NONE',  ( 15.78541918192386362, 10.65456781717563040, -2.670094453781548083 ) ) ;
#24965 = CARTESIAN_POINT ( 'NONE',  ( 81.31240362382358455, 61.49079461182719086, -1.766895996212483722 ) ) ;
#24966 = FACE_OUTER_BOUND ( 'NONE', #23242, .T. ) ;
#24967 = CARTESIAN_POINT ( 'NONE',  ( 77.25588627614904169, 64.91391695767342185, 2.512892981323197716 ) ) ;
#24968 = ORIENTED_EDGE ( 'NONE', *, *, #5070, .T. ) ;
#24969 = CARTESIAN_POINT ( 'NONE',  ( -68.98592816613208356, -42.46322148352267334, -2.168404344971008868E-16 ) ) ;
#24970 = FACE_OUTER_BOUND ( 'NONE', #30190, .T. ) ;
#24971 = CARTESIAN_POINT ( 'NONE',  ( 82.13040900219787943, 64.82864533757677350, 1.905332024690495007 ) ) ;
#24973 = CARTESIAN_POINT ( 'NONE',  ( -1.579832256282212244, -30.79065755753165234, 7.651421919295140484 ) ) ;
#24972 = CARTESIAN_POINT ( 'NONE',  ( 4.254005347624293165, -31.96347340058011710, 6.951256099901589103 ) ) ;
#24974 = CARTESIAN_POINT ( 'NONE',  ( 31.47838864403340509, -3.170179483860372738, -5.357953045474171283 ) ) ;
#24975 = EDGE_CURVE ( 'NONE', #23320, #33375, #40465, .T. ) ;
#24976 = DIRECTION ( 'NONE',  ( -0.000000000000000000, -0.000000000000000000, -1.000000000000000000 ) ) ;
#24977 = CARTESIAN_POINT ( 'NONE',  ( -63.25792396345003255, 35.57414178363083579, -6.629687970507617045 ) ) ;
#24978 = CARTESIAN_POINT ( 'NONE',  ( 23.08405860376734964, 0.3616624716994971123, -5.928390910620995768 ) ) ;
#24979 = EDGE_CURVE ( 'NONE', #11346, #2378, #24592, .T. ) ;
#24980 = CIRCLE ( 'NONE', #30224, 0.04999999999999969746 ) ;
#24981 = CYLINDRICAL_SURFACE ( 'NONE', #35367, 3.000000000000004885 ) ;
#24982 = VERTEX_POINT ( 'NONE', #24848 ) ;
#24983 = DIRECTION ( 'NONE',  ( -0.000000000000000000, -0.000000000000000000, -1.000000000000000000 ) ) ;
#24984 = CARTESIAN_POINT ( 'NONE',  ( 0.5215462454007337989, -32.86543123519535925, 7.643192810543816940 ) ) ;
#24985 = CARTESIAN_POINT ( 'NONE',  ( 33.46397865298071395, -3.088978469517898340, -5.429261216816389179 ) ) ;
#24986 = CARTESIAN_POINT ( 'NONE',  ( 37.17919206969111912, -2.754564175853643437, -6.000958797263274747 ) ) ;
#24987 = CARTESIAN_POINT ( 'NONE',  ( 68.91559242293919851, 58.09233434678947816, -3.947612818959274072 ) ) ;
#24988 = CARTESIAN_POINT ( 'NONE',  ( 30.67121742200687962, -3.774223789334631096, 4.535454642798929292 ) ) ;
#24989 = CARTESIAN_POINT ( 'NONE',  ( 8.290806648384990041, -10.90558813203967148, -2.500000000000000000 ) ) ;
#24990 = DIRECTION ( 'NONE',  ( 0.000000000000000000, 1.000000000000000000, 0.000000000000000000 ) ) ;
#24991 = CARTESIAN_POINT ( 'NONE',  ( -17.07867591359219617, -24.55319635012989110, 6.700000000000000178 ) ) ;
#24992 = CARTESIAN_POINT ( 'NONE',  ( -64.08758708074093136, 38.13199975834722011, -3.043809435734137647 ) ) ;
#24993 = CARTESIAN_POINT ( 'NONE',  ( 20.70210560442331627, 10.21350129193277034, 2.500000000000000888 ) ) ;
#24994 = AXIS2_PLACEMENT_3D ( 'NONE', #3642, #9986, #21950 ) ;
#24995 = DIRECTION ( 'NONE',  ( 0.000000000000000000, 0.000000000000000000, 1.000000000000000000 ) ) ;
#24996 = ORIENTED_EDGE ( 'NONE', *, *, #35047, .F. ) ;
#24997 = SURFACE_SIDE_STYLE ('',( #18804 ) ) ;
#24998 = CARTESIAN_POINT ( 'NONE',  ( 69.37860636825551808, 58.34396603459876474, -3.943722715026765524 ) ) ;
#24999 = VERTEX_POINT ( 'NONE', #28749 ) ;
#25000 = DIRECTION ( 'NONE',  ( -0.7660444431189813441, 0.6427876096865353661, -0.000000000000000000 ) ) ;
#25001 = DIRECTION ( 'NONE',  ( 0.000000000000000000, 0.000000000000000000, 1.000000000000000000 ) ) ;
#25002 = CARTESIAN_POINT ( 'NONE',  ( 4.877799951173103388, -30.77995818745698031, 7.785868773668302545 ) ) ;
#25003 = DIRECTION ( 'NONE',  ( -0.4582725098355704407, 0.8888117386314197121, 0.000000000000000000 ) ) ;
#25004 = VERTEX_POINT ( 'NONE', #28541 ) ;
#25005 = CARTESIAN_POINT ( 'NONE',  ( 21.71132468300342921, 6.334557977395378181, 3.191024146652045257 ) ) ;
#25006 = CARTESIAN_POINT ( 'NONE',  ( -10.87867591359219155, -26.64985754041175525, 6.700000000000000178 ) ) ;
#25007 = ORIENTED_EDGE ( 'NONE', *, *, #26001, .F. ) ;
#25008 = CARTESIAN_POINT ( 'NONE',  ( 80.15150095960399312, 61.72183351646653193, -3.055712048904937639 ) ) ;
#25009 =( BOUNDED_CURVE ( )  B_SPLINE_CURVE ( 3, ( #38205, #18455, #31041, #12690 ),
 .UNSPECIFIED., .F., .T. ) 
 B_SPLINE_CURVE_WITH_KNOTS ( ( 4, 4 ),
 ( 1.347909859412854461, 1.534781240595299634 ),
 .UNSPECIFIED. ) 
 CURVE ( )  GEOMETRIC_REPRESENTATION_ITEM ( )  RATIONAL_B_SPLINE_CURVE ( ( 1.000000000000000000, 0.9970920404276226723, 0.9970920404276226723, 1.000000000000000000 ) ) 
 REPRESENTATION_ITEM ( '' )  );
#25011 = CARTESIAN_POINT ( 'NONE',  ( -1.482288828291198790, -30.76598833619782170, 7.680992449362119778 ) ) ;
#25010 = CARTESIAN_POINT ( 'NONE',  ( 21.73812098194953180, 0.3516627487957126319, 8.764633167989723361 ) ) ;
#25012 = CARTESIAN_POINT ( 'NONE',  ( 81.74641399446780099, 62.01249025250110947, -2.076176908533885701 ) ) ;
#25013 = CARTESIAN_POINT ( 'NONE',  ( 80.71160662450162704, 61.49558808705152302, 2.436540443961503044 ) ) ;
#25014 = EDGE_CURVE ( 'NONE', #141, #20369, #31233, .T. ) ;
#25015 = CARTESIAN_POINT ( 'NONE',  ( 4.433156500894046559, -27.54706021590136444, 6.979335674598000416 ) ) ;
#25016 = EDGE_CURVE ( 'NONE', #18362, #6354, #5040, .T. ) ;
#25017 = AXIS2_PLACEMENT_3D ( 'NONE', #40407, #37329, #8296 ) ;
#25018 = CARTESIAN_POINT ( 'NONE',  ( 82.43037228308448050, 64.59322875725442259, 1.000000000000000000 ) ) ;
#25019 = CARTESIAN_POINT ( 'NONE',  ( 4.667929121870860065, -31.42551012740447902, 7.753200566781599079 ) ) ;
#25020 = CARTESIAN_POINT ( 'NONE',  ( 21.85643539959774273, -8.640774161329524361, 8.772446831725494221 ) ) ;
#25021 = CARTESIAN_POINT ( 'NONE',  ( 21.85643539959776760, -15.17897001446843142, 1.975458193255289263 ) ) ;
#25022 = ORIENTED_EDGE ( 'NONE', *, *, #1420, .T. ) ;
#25023 = CARTESIAN_POINT ( 'NONE',  ( -71.84574099016961668, 0.8742997958048870366, 9.958011348621333525 ) ) ;
#25024 = CARTESIAN_POINT ( 'NONE',  ( 36.68439403812833177, -3.468466653191531357, 5.851900647971171487 ) ) ;
#25025 = ORIENTED_EDGE ( 'NONE', *, *, #38813, .T. ) ;
#25026 = EDGE_CURVE ( 'NONE', #21932, #31406, #19073, .T. ) ;
#25027 = CARTESIAN_POINT ( 'NONE',  ( -8.878675913592189772, -26.64985754041175525, 6.800000000000000711 ) ) ;
#25028 = EDGE_CURVE ( 'NONE', #5967, #12173, #15862, .T. ) ;
#25029 = CARTESIAN_POINT ( 'NONE',  ( -81.49198538235609135, 10.49122877029617129, -2.851835521983549615 ) ) ;
#25030 = CARTESIAN_POINT ( 'NONE',  ( 3.431207382034987763, -26.52784317818328219, 7.743886751744251562 ) ) ;
#25031 = CARTESIAN_POINT ( 'NONE',  ( 33.11474090711421780, -0.1493249260898398267, -4.939405552518099540 ) ) ;
#25032 = APPLICATION_CONTEXT ( 'automotive_design' ) ;
#25033 = CARTESIAN_POINT ( 'NONE',  ( -1.799583860900191734, -29.58343279012807159, 7.635761828346577573 ) ) ;
#25034 = DIRECTION ( 'NONE',  ( 1.000000000000000000, 0.000000000000000000, 0.000000000000000000 ) ) ;
#25035 = CARTESIAN_POINT ( 'NONE',  ( 0.05382362115409088099, -33.98870358965611160, 7.695279973900954751 ) ) ;
#25036 = CARTESIAN_POINT ( 'NONE',  ( 1.731470216958145070, -26.07006818241261215, 6.894806418505347700 ) ) ;
#25037 = CARTESIAN_POINT ( 'NONE',  ( 3.481305170888918887, -32.58295880691792945, 7.700536657684214248 ) ) ;
#25038 = AXIS2_PLACEMENT_3D ( 'NONE', #26999, #12154, #39547 ) ;
#25039 = CARTESIAN_POINT ( 'NONE',  ( 3.912857414353567709, -32.15159409943261437, 7.680992449362120666 ) ) ;
#25040 = CARTESIAN_POINT ( 'NONE',  ( 26.97785997608481523, 1.400405612006494716, -4.405071484031834572 ) ) ;
#25041 = DIRECTION ( 'NONE',  ( -0.000000000000000000, 1.000000000000000000, -0.000000000000000000 ) ) ;
#25042 = CARTESIAN_POINT ( 'NONE',  ( 24.46830168776173053, 2.964004347679559004, -3.655893466831604766 ) ) ;
#25043 = B_SPLINE_CURVE_WITH_KNOTS ( 'NONE', 3,
 ( #26865, #1175, #36143, #35942, #8108, #23373, #7723, #4456, #13499, #4841 ),
 .UNSPECIFIED., .F., .F.,
 ( 4, 3, 3, 4 ),
 ( 8.673617379884035472E-19, 3.025570593003193312E-05, 6.051145698343867694E-05, 6.468151674593740786E-05 ),
 .UNSPECIFIED. ) ;
#25044 = VERTEX_POINT ( 'NONE', #31036 ) ;
#25045 = ORIENTED_EDGE ( 'NONE', *, *, #19629, .T. ) ;
#25046 = CARTESIAN_POINT ( 'NONE',  ( 67.10699435067097340, 58.18157613906911507, 3.995511504169227290 ) ) ;
#25047 = CARTESIAN_POINT ( 'NONE',  ( 31.75252458562886915, -0.4599371113500814179, 5.162147417933157456 ) ) ;
#25048 = CARTESIAN_POINT ( 'NONE',  ( 3.963477911421234623, -32.23984282750152630, 7.750000000000001776 ) ) ;
#25049 = CARTESIAN_POINT ( 'NONE',  ( -63.03213158086114021, 38.26878225442446535, 4.032857076801014351 ) ) ;
#25050 = CARTESIAN_POINT ( 'NONE',  ( 88.14352194013933683, -1.303227188646099544, -4.271130342077624320 ) ) ;
#25051 = VECTOR ( 'NONE', #35277, 1000.000000000000000 ) ;
#25052 = CARTESIAN_POINT ( 'NONE',  ( 36.39130890773654414, -2.321068141369555082, -5.886141900820864414 ) ) ;
#25053 = EDGE_LOOP ( 'NONE', ( #21241, #36432, #34635, #16540 ) ) ;
#25054 = CARTESIAN_POINT ( 'NONE',  ( 25.65562067725548090, 2.148648913715160091, 4.136967372009855204 ) ) ;
#25055 = CARTESIAN_POINT ( 'NONE',  ( 0.6783104270758654186, -48.60743831809499227, 6.000000000000000000 ) ) ;
#25056 = ORIENTED_EDGE ( 'NONE', *, *, #19818, .T. ) ;
#25057 = FACE_OUTER_BOUND ( 'NONE', #21630, .T. ) ;
#25058 = VERTEX_POINT ( 'NONE', #2842 ) ;
#25059 = CARTESIAN_POINT ( 'NONE',  ( 80.00230669363345726, 63.71856487089240773, -3.706996517075249464 ) ) ;
#25060 = CARTESIAN_POINT ( 'NONE',  ( -1.699145597547422781, -29.51370389567643571, 7.785387725071483800 ) ) ;
#25061 = CARTESIAN_POINT ( 'NONE',  ( 80.03595747215288725, 63.73611138703241608, 3.702313260098205383 ) ) ;
#25064 = ORIENTED_EDGE ( 'NONE', *, *, #30841, .F. ) ;
#25063 = ORIENTED_EDGE ( 'NONE', *, *, #11054, .F. ) ;
#25062 = DIRECTION ( 'NONE',  ( 1.000000000000000000, 0.000000000000000000, -0.000000000000000000 ) ) ;
#25065 = VECTOR ( 'NONE', #20159, 1000.000000000000000 ) ;
#25066 = CARTESIAN_POINT ( 'NONE',  ( -0.01981084510887724456, -26.53464568598458229, 7.781480525794718162 ) ) ;
#25067 = CARTESIAN_POINT ( 'NONE',  ( -32.44874870218063734, -25.49307895267003587, 6.700000000000000178 ) ) ;
#25068 = DIRECTION ( 'NONE',  ( 0.000000000000000000, 0.7541618601367565677, -0.6566885781822819901 ) ) ;
#25069 = VECTOR ( 'NONE', #27992, 1000.000000000000000 ) ;
#25070 = CARTESIAN_POINT ( 'NONE',  ( -1.582528736513596490, -30.78337320113038444, 7.750000000000000000 ) ) ;
#25071 = CARTESIAN_POINT ( 'NONE',  ( 24.05978824533461591, 3.343990756392554609, -3.225742063477944566 ) ) ;
#25072 = ORIENTED_EDGE ( 'NONE', *, *, #1739, .T. ) ;
#25073 = CARTESIAN_POINT ( 'NONE',  ( 3.427626883898521548, -33.95934199490189087, 7.754798119455333705 ) ) ;
#25074 = EDGE_CURVE ( 'NONE', #38802, #12078, #11320, .T. ) ;
#25075 = ADVANCED_FACE ( 'NONE', ( #15575 ), #40682, .F. ) ;
#25076 = CARTESIAN_POINT ( 'NONE',  ( 24.25791012409692371, 0.7154099962172090210, -6.776768987914707942 ) ) ;
#25077 = VECTOR ( 'NONE', #7849, 1000.000000000000000 ) ;
#25078 = EDGE_CURVE ( 'NONE', #17373, #21802, #1722, .T. ) ;
#25079 = CARTESIAN_POINT ( 'NONE',  ( -75.83774951876674209, -5.401831623872992871, -8.713785153582826126 ) ) ;
#25080 = DIRECTION ( 'NONE',  ( -0.000000000000000000, -1.000000000000000000, -0.000000000000000000 ) ) ;
#25081 = CARTESIAN_POINT ( 'NONE',  ( 79.72834705192842364, 65.67299761742502540, 2.773332820898658291 ) ) ;
#25082 = CARTESIAN_POINT ( 'NONE',  ( 85.19771215196759329, 1.813128620488922760, 5.066052097874169213 ) ) ;
#25083 = CARTESIAN_POINT ( 'NONE',  ( 21.05507626271832677, 6.110270179408970215, 3.370876190096979474 ) ) ;
#25084 = ORIENTED_EDGE ( 'NONE', *, *, #31085, .T. ) ;
#25085 = CARTESIAN_POINT ( 'NONE',  ( -1.544665293549569052, -28.25920506871950622, 7.754798119455333705 ) ) ;
#25086 = CARTESIAN_POINT ( 'NONE',  ( 4.582084150952498547, -31.37432464074042215, 7.754798119455333705 ) ) ;
#25087 = CARTESIAN_POINT ( 'NONE',  ( 4.086607214483024997, -27.00946490984718196, 6.912143950357347855 ) ) ;
#25088 = CARTESIAN_POINT ( 'NONE',  ( 0.8807958757747544887, 0.5999999999999995337, 3.993526596136941720 ) ) ;
#25089 = CARTESIAN_POINT ( 'NONE',  ( -1.526829923184012339, -28.21528965334980654, 7.013842709614101167 ) ) ;
#25090 = CARTESIAN_POINT ( 'NONE',  ( 85.93940314300044747, 0.3675543374994592050, 5.999999582814343313 ) ) ;
#25091 = EDGE_LOOP ( 'NONE', ( #38974, #23376, #25907, #18304, #9855 ) ) ;
#25092 = CARTESIAN_POINT ( 'NONE',  ( 25.29564187210237591, 1.734060676602622975, 4.154394710188922701 ) ) ;
#25093 = B_SPLINE_CURVE_WITH_KNOTS ( 'NONE', 3,
 ( #30136, #4816, #33454, #39590, #20862, #1953, #17151, #14068, #14271, #26647, #27449, #40005, #23555, #17757, #39180, #17964, #17346, #30345, #29924, #2151, #27240, #26841, #14670, #39381, #39807, #36315, #8085, #33649, #20652, #11576, #24357 ),
 .UNSPECIFIED., .F., .F.,
 ( 4, 3, 3, 3, 3, 3, 3, 3, 3, 3, 4 ),
 ( 8.673617379884035472E-19, 3.077658087705791864E-05, 6.152638666998900326E-05, 9.267501192706637957E-05, 0.0001241882240135233184, 0.0001556618703051675047, 0.0001866161554452220868, 0.0002167966385861002884, 0.0002463805737537799290, 0.0002758761370306525443, 0.0002847094172290028265 ),
 .UNSPECIFIED. ) ;
#25094 = CARTESIAN_POINT ( 'NONE',  ( 87.09859342968812257, 0.5244505078549105415, -5.068689133590885909 ) ) ;
#25095 = ORIENTED_EDGE ( 'NONE', *, *, #18609, .T. ) ;
#25097 = DIRECTION ( 'NONE',  ( 0.000000000000000000, 0.000000000000000000, 1.000000000000000000 ) ) ;
#25096 = CARTESIAN_POINT ( 'NONE',  ( 81.20569604368299110, 61.99964894245921698, -2.688322534164195421 ) ) ;
#25098 = DIRECTION ( 'NONE',  ( 1.000000000000000000, 0.000000000000000000, 0.000000000000000000 ) ) ;
#25099 = CARTESIAN_POINT ( 'NONE',  ( 14.66483024702261773, 13.02142279098982591, -2.495199448944585452 ) ) ;
#25100 = VERTEX_POINT ( 'NONE', #25260 ) ;
#25101 = LINE ( 'NONE', #22429, #4351 ) ;
#25102 = ORIENTED_EDGE ( 'NONE', *, *, #2170, .F. ) ;
#25103 = CARTESIAN_POINT ( 'NONE',  ( 1.018372654493346685, -32.90083822981368655, 6.866852738645442322 ) ) ;
#25104 = VECTOR ( 'NONE', #6592, 1000.000000000000114 ) ;
#25105 = VERTEX_POINT ( 'NONE', #10793 ) ;
#25106 = CARTESIAN_POINT ( 'NONE',  ( 79.16740428156647624, 65.60392721301286656, -2.747716423863119761 ) ) ;
#25107 = CARTESIAN_POINT ( 'NONE',  ( 23.40509239944908870, 3.763556924256647562, 3.087706618777893652 ) ) ;
#25108 = ORIENTED_EDGE ( 'NONE', *, *, #17536, .T. ) ;
#25110 = CARTESIAN_POINT ( 'NONE',  ( 36.16041087367324280, -1.555341878182815440, 5.654033472726598397 ) ) ;
#25109 = CARTESIAN_POINT ( 'NONE',  ( 24.19261158263253719, 2.582287494170470321, 4.035689301652516825 ) ) ;
#25111 = EDGE_LOOP ( 'NONE', ( #28025, #659, #18690, #15946 ) ) ;
#25112 = CARTESIAN_POINT ( 'NONE',  ( 81.16771000429746152, 61.30329618601648889, -1.041818241550651614 ) ) ;
#25113 = CARTESIAN_POINT ( 'NONE',  ( -12.44874870218064267, -25.49307895267003587, 6.700000000000000178 ) ) ;
#25115 = DIRECTION ( 'NONE',  ( 0.000000000000000000, -1.147978770867004622E-16, 1.000000000000000000 ) ) ;
#25114 = DIRECTION ( 'NONE',  ( 0.000000000000000000, 0.000000000000000000, 1.000000000000000000 ) ) ;
#25116 = FACE_OUTER_BOUND ( 'NONE', #29954, .T. ) ;
#25117 = CARTESIAN_POINT ( 'NONE',  ( 0.5233279421899477146, -26.28305482120240910, 7.778495531946297170 ) ) ;
#25118 = CARTESIAN_POINT ( 'NONE',  ( 73.45088770829859470, 61.50831400533110127, 3.795548882783541522 ) ) ;
#25119 = CARTESIAN_POINT ( 'NONE',  ( 21.85424650998301743, 3.950402723962838092, -4.385458540445601905 ) ) ;
#25120 = VERTEX_POINT ( 'NONE', #14090 ) ;
#25121 = CARTESIAN_POINT ( 'NONE',  ( 5.144846875551112753, -28.94886861257825572, 7.635761828346576685 ) ) ;
#25122 = CARTESIAN_POINT ( 'NONE',  ( 21.85643539959776049, -3.688311691778667800, 15.92486026856874304 ) ) ;
#25124 = EDGE_CURVE ( 'NONE', #3011, #15995, #38804, .T. ) ;
#25123 = DIRECTION ( 'NONE',  ( 0.000000000000000000, -0.6662082868431813409, -0.7457657263118716573 ) ) ;
#25125 = ORIENTED_EDGE ( 'NONE', *, *, #16450, .F. ) ;
#25126 = CARTESIAN_POINT ( 'NONE',  ( 1.057293288892434457, -26.12951937787816448, 7.698786668945013290 ) ) ;
#25127 = CARTESIAN_POINT ( 'NONE',  ( 81.74641399446790047, 62.01249025250114499, 2.076176908533788446 ) ) ;
#25128 = CARTESIAN_POINT ( 'NONE',  ( 85.02283808163620904, 2.856037436078923797, 1.058370034767218248 ) ) ;
#25129 = ORIENTED_EDGE ( 'NONE', *, *, #22349, .F. ) ;
#25130 = CARTESIAN_POINT ( 'NONE',  ( 0.5270406883574831891, -32.76106163285440687, 7.775108481317162479 ) ) ;
#25131 = CARTESIAN_POINT ( 'NONE',  ( 17.12179616700453622, -3.119139029776307304, 2.877302616401834712 ) ) ;
#25132 = CARTESIAN_POINT ( 'NONE',  ( 36.78937917427825965, -3.042007186898596949, -5.948270393280488122 ) ) ;
#25133 = CARTESIAN_POINT ( 'NONE',  ( 5.098282653295018285, -29.68964042297140793, 7.757178535559534183 ) ) ;
#25134 = CARTESIAN_POINT ( 'NONE',  ( 4.834836695125773076, -27.99731481096146624, 7.387053503561885393 ) ) ;
#25135 = CARTESIAN_POINT ( 'NONE',  ( -76.50589831764405346, -4.344217460646190965, 9.790531055125489601 ) ) ;
#25136 = AXIS2_PLACEMENT_3D ( 'NONE', #4587, #23900, #14032 ) ;
#25137 = CARTESIAN_POINT ( 'NONE',  ( -1.229343149638864485, -31.29523348278805983, 7.730758795053808363 ) ) ;
#25138 = VERTEX_POINT ( 'NONE', #16770 ) ;
#25139 = VERTEX_POINT ( 'NONE', #7121 ) ;
#25140 = CARTESIAN_POINT ( 'NONE',  ( 37.18590179202365675, -2.963059666527390057, 6.000009849583459065 ) ) ;
#25141 = DIRECTION ( 'NONE',  ( -0.000000000000000000, -0.000000000000000000, -1.000000000000000000 ) ) ;
#25142 = ADVANCED_FACE ( 'NONE', ( #19875 ), #756, .F. ) ;
#25143 = CARTESIAN_POINT ( 'NONE',  ( 66.68223030933245354, 57.98259542220473861, -3.998057522776775841 ) ) ;
#25144 = ORIENTED_EDGE ( 'NONE', *, *, #29478, .F. ) ;
#25145 = CARTESIAN_POINT ( 'NONE',  ( -56.58158928110407970, 30.30283765713129540, 3.953813256333435611 ) ) ;
#25146 = CARTESIAN_POINT ( 'NONE',  ( -80.83360071539431146, -6.606523484500073096, -1.436172935955783991 ) ) ;
#25147 = ORIENTED_EDGE ( 'NONE', *, *, #8685, .T. ) ;
#25148 = FACE_BOUND ( 'NONE', #23129, .T. ) ;
#25149 = CARTESIAN_POINT ( 'NONE',  ( -70.92837670882107659, -60.53509472482660669, -5.950000000000010836 ) ) ;
#25150 = VERTEX_POINT ( 'NONE', #29744 ) ;
#25151 = CARTESIAN_POINT ( 'NONE',  ( 21.72876610684703635, 6.177728964813395507, 3.247520083845313987 ) ) ;
#25152 = CARTESIAN_POINT ( 'NONE',  ( 78.99593020234610208, 66.21156118037407623, -1.070820504727074685 ) ) ;
#25153 = ADVANCED_FACE ( 'NONE', ( #7517 ), #10599, .F. ) ;
#25154 = CARTESIAN_POINT ( 'NONE',  ( 81.09687786842310686, 61.96238702813622723, 2.735335646780897800 ) ) ;
#25155 = CARTESIAN_POINT ( 'NONE',  ( -1.750039336912785126, -28.98295539875205762, 7.744938106820263179 ) ) ;
#25156 = VERTEX_POINT ( 'NONE', #1368 ) ;
#25157 = CARTESIAN_POINT ( 'NONE',  ( 77.35226663217761711, 63.40502609692226343, -3.687756614093553154 ) ) ;
#25159 = CARTESIAN_POINT ( 'NONE',  ( -70.95330471031414277, 33.71485196875532608, -8.800414904976364028 ) ) ;
#25158 = CARTESIAN_POINT ( 'NONE',  ( -70.92837670882107659, -45.61702805680359063, 6.000000000000002665 ) ) ;
#25160 = CARTESIAN_POINT ( 'NONE',  ( 15.02851297552613907, 11.88222368738628276, -2.551960934427589756 ) ) ;
#25161 = CARTESIAN_POINT ( 'NONE',  ( 80.40747942978335061, 64.69963996956799690, -3.448515284080292620 ) ) ;
#25162 = CARTESIAN_POINT ( 'NONE',  ( -6.878675913592188884, -24.55319635012989110, 6.800000000000000711 ) ) ;
#25163 = CARTESIAN_POINT ( 'NONE',  ( 77.16059773406418287, 63.78117330919809547, 3.480716904142236334 ) ) ;
#25164 = ORIENTED_EDGE ( 'NONE', *, *, #9110, .F. ) ;
#25165 = VECTOR ( 'NONE', #7720, 1000.000000000000000 ) ;
#25166 = ORIENTED_EDGE ( 'NONE', *, *, #30893, .F. ) ;
#25167 = LINE ( 'NONE', #40594, #10241 ) ;
#25169 = EDGE_CURVE ( 'NONE', #5237, #35661, #25783, .T. ) ;
#25168 = DIRECTION ( 'NONE',  ( 0.000000000000000000, -1.000000000000000000, 0.000000000000000000 ) ) ;
#25170 = CARTESIAN_POINT ( 'NONE',  ( 78.97185648144790093, 66.19841638340301415, 1.173033592341439002 ) ) ;
#25172 = CARTESIAN_POINT ( 'NONE',  ( -1.583891440918162585, -30.77968007673214146, 7.635761828346579350 ) ) ;
#25171 = CARTESIAN_POINT ( 'NONE',  ( 4.267027349875077924, -31.94950500413386862, 7.009310105710487626 ) ) ;
#25173 = CARTESIAN_POINT ( 'NONE',  ( 29.34248944929254677, 1.775380825033272991, -3.063368523016994249 ) ) ;
#25174 =( BOUNDED_CURVE ( )  B_SPLINE_CURVE ( 3, ( #19862, #32434, #36126, #29731 ),
 .UNSPECIFIED., .F., .T. ) 
 B_SPLINE_CURVE_WITH_KNOTS ( ( 4, 4 ),
 ( 4.748221474220561511, 4.941946782021394924 ),
 .UNSPECIFIED. ) 
 CURVE ( )  GEOMETRIC_REPRESENTATION_ITEM ( )  RATIONAL_B_SPLINE_CURVE ( ( 1.000000000000000000, 0.9968749865767494445, 0.9968749865767494445, 1.000000000000000000 ) ) 
 REPRESENTATION_ITEM ( '' )  );
#25175 = CARTESIAN_POINT ( 'NONE',  ( -1.412656310956876826, -31.16960079952658091, 7.011627023500184741 ) ) ;
#25176 = CARTESIAN_POINT ( 'NONE',  ( -62.84881660470023945, 35.59796388917940391, -5.828906544001253742 ) ) ;
#25177 = CARTESIAN_POINT ( 'NONE',  ( -62.75216693000863444, 36.25077706935546473, 4.893820751807268721 ) ) ;
#25178 = CARTESIAN_POINT ( 'NONE',  ( 4.692798180838874345, -31.35690285333599903, 7.785344483711592822 ) ) ;
#25179 = ORIENTED_EDGE ( 'NONE', *, *, #37726, .F. ) ;
#25180 = DIRECTION ( 'NONE',  ( 1.000000000000000000, 0.000000000000000000, 0.000000000000000000 ) ) ;
#25181 = DIRECTION ( 'NONE',  ( 0.000000000000000000, 0.000000000000000000, 1.000000000000000000 ) ) ;
#25182 = CARTESIAN_POINT ( 'NONE',  ( 5.036005266467588726, -25.61570514420120048, 7.635761828346577573 ) ) ;
#25183 = CARTESIAN_POINT ( 'NONE',  ( 29.45350768790538609, 1.169329251362175803, -4.331148011843218626 ) ) ;
#25184 = CARTESIAN_POINT ( 'NONE',  ( 11.29080664838498826, -10.90558813203967148, 2.500000000000000000 ) ) ;
#25185 = CARTESIAN_POINT ( 'NONE',  ( 1.727929540585121382, -33.06982342786876217, 7.655937882338900380 ) ) ;
#25186 = PLANE ( 'NONE',  #8099 ) ;
#25187 = CARTESIAN_POINT ( 'NONE',  ( -22.87867591359218977, -24.55319635012989110, 6.700000000000000178 ) ) ;
#25188 = CARTESIAN_POINT ( 'NONE',  ( -75.68638550784876884, 8.581835957161722206, 10.20520400634731395 ) ) ;
#25189 = AXIS2_PLACEMENT_3D ( 'NONE', #14303, #11813, #17585 ) ;
#25190 = DIRECTION ( 'NONE',  ( -0.9396926207858986579, 0.3420201433256953027, 0.000000000000000000 ) ) ;
#25191 = ADVANCED_FACE ( 'NONE', ( #10198 ), #9998, .F. ) ;
#25192 = DIRECTION ( 'NONE',  ( 1.000000000000000000, 0.000000000000000000, 0.000000000000000000 ) ) ;
#25193 = CARTESIAN_POINT ( 'NONE',  ( -1.544331477769930183, -30.58574382593747742, 6.871394612369937427 ) ) ;
#25194 = ORIENTED_EDGE ( 'NONE', *, *, #26873, .T. ) ;
#25195 = B_SPLINE_CURVE_WITH_KNOTS ( 'NONE', 3,
 ( #28628, #25538, #22262, #3137, #10076, #16458, #34829, #834, #28200, #31, #25130, #22049, #38081, #636, #6605, #22659, #13176, #19564, #18950, #9883, #38475, #19151, #15857, #22458, #25940 ),
 .UNSPECIFIED., .F., .F.,
 ( 4, 3, 3, 3, 3, 3, 3, 3, 4 ),
 ( 6.468151674593708260E-05, 9.076621574722118632E-05, 0.0001210204262067982105, 0.0001512763324577447578, 0.0001815301820994211050, 0.0002117781465860732264, 0.0002420274594459720092, 0.0002722905548971162764, 0.0002816827545175584085 ),
 .UNSPECIFIED. ) ;
#25196 = CARTESIAN_POINT ( 'NONE',  ( 4.503588519744932128, -31.67704982672819014, 7.139344958878411695 ) ) ;
#25197 = CARTESIAN_POINT ( 'NONE',  ( 68.51828301517210207, 58.84837915819282728, -3.980709302925311555 ) ) ;
#25198 = AXIS2_PLACEMENT_3D ( 'NONE', #1235, #11059, #23240 ) ;
#25199 = ORIENTED_EDGE ( 'NONE', *, *, #28255, .T. ) ;
#25200 = LINE ( 'NONE', #37732, #37062 ) ;
#25201 = CARTESIAN_POINT ( 'NONE',  ( -32.24874870218063450, -26.64985754041175525, 6.800000000000000711 ) ) ;
#25202 = CARTESIAN_POINT ( 'NONE',  ( 21.85576838308406522, 3.890922448482609042, 4.421358135619450458 ) ) ;
#25203 = CARTESIAN_POINT ( 'NONE',  ( 5.047147375954016191, -28.54561077161946869, 6.912143950357347855 ) ) ;
#25204 = EDGE_CURVE ( 'NONE', #25800, #40638, #38199, .T. ) ;
#25205 = EDGE_CURVE ( 'NONE', #26823, #35733, #13525, .T. ) ;
#25206 = CARTESIAN_POINT ( 'NONE',  ( 3.522825846568940378, -26.58183247331710319, 6.865554069792297653 ) ) ;
#25207 = CARTESIAN_POINT ( 'NONE',  ( 5.025873565333792925, -30.27785960640749963, 7.757178535559534183 ) ) ;
#25208 = ORIENTED_EDGE ( 'NONE', *, *, #31297, .T. ) ;
#25209 = EDGE_CURVE ( 'NONE', #31513, #4122, #16432, .T. ) ;
#25210 = CARTESIAN_POINT ( 'NONE',  ( 23.44095116515602228, 3.798737197898152118, 3.085442469092725126 ) ) ;
#25211 = DIRECTION ( 'NONE',  ( -0.6427876096865179356, -0.7660444431189958880, 0.000000000000000000 ) ) ;
#25212 = VECTOR ( 'NONE', #5639, 1000.000000000000000 ) ;
#25213 = VERTEX_POINT ( 'NONE', #11196 ) ;
#25214 = CARTESIAN_POINT ( 'NONE',  ( 0.4702888575080005906, -26.29321669331516631, 7.710604733652626663 ) ) ;
#25215 = ORIENTED_EDGE ( 'NONE', *, *, #33013, .F. ) ;
#25216 = CARTESIAN_POINT ( 'NONE',  ( 80.42502267531087057, 61.03612496587228975, -1.832491541757258258 ) ) ;
#25217 = B_SPLINE_CURVE_WITH_KNOTS ( 'NONE', 3,
 ( #39384, #8498, #11176, #8908, #34068, #5022, #27452, #27650, #27048, #14275, #21081, #23747, #39810, #8702, #11989, #5843, #8088, #40008, #39594 ),
 .UNSPECIFIED., .F., .F.,
 ( 4, 3, 3, 3, 3, 3, 4 ),
 ( 4.336808689942017255E-19, 2.546128104244576053E-05, 5.711050680483990296E-05, 8.113074941675622203E-05, 0.0001053129305727039069, 0.0001360598016347098994, 0.0001612931755702010528 ),
 .UNSPECIFIED. ) ;
#25219 = CARTESIAN_POINT ( 'NONE',  ( -0.9993095062657011418, -27.34246030201092381, 7.730015791551952731 ) ) ;
#25218 = CARTESIAN_POINT ( 'NONE',  ( 25.36652333831873207, 0.7419792049594144956, 4.603917168115059688 ) ) ;
#25220 = CARTESIAN_POINT ( 'NONE',  ( 79.96642255696579582, 65.80764937177660556, -2.611089443229511087 ) ) ;
#25221 = CARTESIAN_POINT ( 'NONE',  ( 79.18319737856852214, 64.63648950223996792, 3.475409704257728105 ) ) ;
#25222 = VERTEX_POINT ( 'NONE', #1763 ) ;
#25223 = B_SPLINE_CURVE_WITH_KNOTS ( 'NONE', 3,
 ( #34382, #190, #31683, #18486 ),
 .UNSPECIFIED., .F., .F.,
 ( 4, 4 ),
 ( 2.602085213965210642E-18, 0.0006739815419856422761 ),
 .UNSPECIFIED. ) ;
#25224 = CARTESIAN_POINT ( 'NONE',  ( 82.18775271763095702, 62.23297483488567394, 1.000000000000000000 ) ) ;
#25225 = CARTESIAN_POINT ( 'NONE',  ( 2.748053412748273860, -32.80449376584813592, 7.754798119455333705 ) ) ;
#25226 = CARTESIAN_POINT ( 'NONE',  ( 21.85643539959774273, -5.916281280498693285, 11.28130179073419015 ) ) ;
#25227 = CARTESIAN_POINT ( 'NONE',  ( 3.300000000000000711, 5.204748896376251685E-16, 4.250000000000000000 ) ) ;
#25228 = EDGE_LOOP ( 'NONE', ( #21572, #3350, #12440, #9947 ) ) ;
#25229 = CARTESIAN_POINT ( 'NONE',  ( -74.22931914091192596, 6.964638644170447535, 9.493301944864269259 ) ) ;
#25230 = CARTESIAN_POINT ( 'NONE',  ( 36.65102539693456407, -3.484761920582832850, 5.842386807897074874 ) ) ;
#25231 = VERTEX_POINT ( 'NONE', #27261 ) ;
#25232 = DIRECTION ( 'NONE',  ( 0.1736481776669404897, -0.9848077530122062440, -0.000000000000000000 ) ) ;
#25233 = ORIENTED_EDGE ( 'NONE', *, *, #15704, .T. ) ;
#25234 = CARTESIAN_POINT ( 'NONE',  ( -81.58802495621657158, 10.48337376234404594, -2.413223970079951375 ) ) ;
#25235 = CARTESIAN_POINT ( 'NONE',  ( 28.65970685016134212, -3.315807845019801636, -4.679438410342736887 ) ) ;
#25236 = CARTESIAN_POINT ( 'NONE',  ( 34.14229113142901184, -3.848523386208314356, -5.234441351989421065 ) ) ;
#25237 = FACE_OUTER_BOUND ( 'NONE', #835, .T. ) ;
#25238 = CARTESIAN_POINT ( 'NONE',  ( 17.87965550805309789, 8.681448112502556214, 2.924000077491842209 ) ) ;
#25239 = CARTESIAN_POINT ( 'NONE',  ( -70.92837670882107659, 28.72470171467712063, 3.784187430299790211 ) ) ;
#25240 = CARTESIAN_POINT ( 'NONE',  ( 30.14635126286890809, -3.703246014866541813, 4.591439750246522067 ) ) ;
#25241 = DIRECTION ( 'NONE',  ( 0.000000000000000000, 0.000000000000000000, 1.000000000000000000 ) ) ;
#25242 = DIRECTION ( 'NONE',  ( 0.000000000000000000, 0.000000000000000000, 1.000000000000000000 ) ) ;
#25243 = CIRCLE ( 'NONE', #7475, 3.499999999999999556 ) ;
#25244 = CARTESIAN_POINT ( 'NONE',  ( 21.74663786822173250, 0.5495625321154745668, -8.317879680902361628 ) ) ;
#25245 = CARTESIAN_POINT ( 'NONE',  ( 33.45716606812183613, -3.829385970599605393, -5.093809925484540813 ) ) ;
#25246 = CARTESIAN_POINT ( 'NONE',  ( 24.35712842162025282, 2.896715692034056211, -3.774200513959965697 ) ) ;
#25247 = ORIENTED_EDGE ( 'NONE', *, *, #17443, .F. ) ;
#25248 = ORIENTED_EDGE ( 'NONE', *, *, #18499, .T. ) ;
#25249 = CARTESIAN_POINT ( 'NONE',  ( 67.02763120020985355, 57.94366503926806899, 3.998791315154376136 ) ) ;
#25250 = CARTESIAN_POINT ( 'NONE',  ( 34.76884925160979378, -3.305569524749743859, 5.632917832143227166 ) ) ;
#25251 = EDGE_CURVE ( 'NONE', #39141, #14763, #14494, .T. ) ;
#25252 = CIRCLE ( 'NONE', #12080, 0.1000000000000028644 ) ;
#25254 = ADVANCED_FACE ( 'NONE', ( #24180 ), #1976, .F. ) ;
#25253 = CARTESIAN_POINT ( 'NONE',  ( 86.11108918975101290, 0.7237488529220831301, -5.972109037703948076 ) ) ;
#25255 = CARTESIAN_POINT ( 'NONE',  ( 34.81543154690208297, -1.659450418315846276, -5.640188125924651352 ) ) ;
#25256 = CARTESIAN_POINT ( 'NONE',  ( -11.07867591359219794, -24.55319635012989110, 6.700000000000000178 ) ) ;
#25257 =( BOUNDED_CURVE ( )  B_SPLINE_CURVE ( 3, ( #21898, #15712, #18180, #40615 ),
 .UNSPECIFIED., .F., .T. ) 
 B_SPLINE_CURVE_WITH_KNOTS ( ( 4, 4 ),
 ( 1.347909859412854683, 1.534781240595299190 ),
 .UNSPECIFIED. ) 
 CURVE ( )  GEOMETRIC_REPRESENTATION_ITEM ( )  RATIONAL_B_SPLINE_CURVE ( ( 1.000000000000000000, 0.9970920404276226723, 0.9970920404276226723, 1.000000000000000000 ) ) 
 REPRESENTATION_ITEM ( '' )  );
#25258 = ORIENTED_EDGE ( 'NONE', *, *, #19496, .F. ) ;
#25259 = CARTESIAN_POINT ( 'NONE',  ( 24.45682347496569875, 2.962563052341233405, 3.663525943864573531 ) ) ;
#25260 = CARTESIAN_POINT ( 'NONE',  ( 22.01622206693788897, 4.835086392017111656, 3.641232820207879417 ) ) ;
#25261 = ADVANCED_FACE ( 'NONE', ( #14910 ), #14694, .F. ) ;
#25262 = CARTESIAN_POINT ( 'NONE',  ( 0.03162470699431392529, -32.53223031769636009, 7.693875151218754205 ) ) ;
#25263 = VERTEX_POINT ( 'NONE', #39613 ) ;
#25264 = VERTEX_POINT ( 'NONE', #20888 ) ;
#25265 = CARTESIAN_POINT ( 'NONE',  ( 79.79878548311195630, 63.97024398824578384, -3.714073935154548867 ) ) ;
#25266 = CARTESIAN_POINT ( 'NONE',  ( -1.697502466828836099, -29.45021994381539088, 7.757178535559534183 ) ) ;
#25267 = CARTESIAN_POINT ( 'NONE',  ( 81.01114204962451026, 61.40637449960412653, 2.012706562768916019 ) ) ;
#25270 = ORIENTED_EDGE ( 'NONE', *, *, #23425, .T. ) ;
#25269 = ORIENTED_EDGE ( 'NONE', *, *, #18030, .F. ) ;
#25268 = CARTESIAN_POINT ( 'NONE',  ( -1.336162095501038483, -31.09943851454543662, 7.006423389747789443 ) ) ;
#25271 = AXIS2_PLACEMENT_3D ( 'NONE', #18716, #28184, #3119 ) ;
#25272 = CARTESIAN_POINT ( 'NONE',  ( 7.121324086407810228, -24.55319635012989110, 6.700000000000000178 ) ) ;
#25273 = CARTESIAN_POINT ( 'NONE',  ( 25.30351261480555181, -5.499558619331433640, 2.998554388806299098 ) ) ;
#25274 = FACE_OUTER_BOUND ( 'NONE', #4048, .T. ) ;
#25275 = CARTESIAN_POINT ( 'NONE',  ( 5.036005266467588726, -25.61570514420120048, 7.635761828346577573 ) ) ;
#25276 = CARTESIAN_POINT ( 'NONE',  ( 21.83340148893537247, 5.944224929364805732, -3.144417420793418572 ) ) ;
#25277 = VERTEX_POINT ( 'NONE', #30578 ) ;
#25278 = DIRECTION ( 'NONE',  ( 0.5000000000000101030, -0.8660254037844328234, -0.000000000000000000 ) ) ;
#25279 = CIRCLE ( 'NONE', #40385, 3.499999999999999556 ) ;
#25280 = CARTESIAN_POINT ( 'NONE',  ( -0.9697213352172494583, -31.67483301990728251, 6.864651958020303368 ) ) ;
#25281 = CARTESIAN_POINT ( 'NONE',  ( -1.654012860102806792, -29.01496998062980381, 7.693875151218752428 ) ) ;
#25282 = CARTESIAN_POINT ( 'NONE',  ( -81.77719981938685123, -5.605734774677030963, -1.101378227362841855 ) ) ;
#25283 = VECTOR ( 'NONE', #9449, 1000.000000000000000 ) ;
#25284 = DIRECTION ( 'NONE',  ( -0.000000000000000000, -0.000000000000000000, -1.000000000000000000 ) ) ;
#25285 = CARTESIAN_POINT ( 'NONE',  ( 80.03255827398542976, 65.21842193378448371, 3.211742283750887328 ) ) ;
#25286 = CARTESIAN_POINT ( 'NONE',  ( 87.73180046618776373, -1.932853647757891258, -3.545598201197500465 ) ) ;
#25287 = CARTESIAN_POINT ( 'NONE',  ( -0.03042719556877983289, -32.61201718860353083, 7.743886751744253338 ) ) ;
#25288 = VERTEX_POINT ( 'NONE', #7920 ) ;
#25289 = CARTESIAN_POINT ( 'NONE',  ( 0.000000000000000000, 0.5999999999999995337, 3.730072921939604047 ) ) ;
#25290 = CARTESIAN_POINT ( 'NONE',  ( 24.95151757009657345, 3.450432584360191512, -1.327079065887385667 ) ) ;
#25291 = EDGE_CURVE ( 'NONE', #15467, #28971, #20554, .T. ) ;
#25292 = CARTESIAN_POINT ( 'NONE',  ( 4.088894828626523648, -27.01159991581719311, 6.989977667959445640 ) ) ;
#25293 = CARTESIAN_POINT ( 'NONE',  ( 17.06237155660811311, -3.282733088328227744, -2.837945724647277235 ) ) ;
#25294 = CARTESIAN_POINT ( 'NONE',  ( -28.97867591359219475, -26.64985754041175525, 6.700000000000000178 ) ) ;
#25295 = PLANE ( 'NONE',  #12822 ) ;
#25296 = EDGE_LOOP ( 'NONE', ( #26515, #6483, #40128, #8370 ) ) ;
#25297 = CARTESIAN_POINT ( 'NONE',  ( 36.97940331721468254, -2.956265398274180889, 5.977928256536974239 ) ) ;
#25298 = VECTOR ( 'NONE', #2306, 1000.000000000000000 ) ;
#25299 = VECTOR ( 'NONE', #15749, 1000.000000000000000 ) ;
#25300 = CARTESIAN_POINT ( 'NONE',  ( 87.34576652878352832, 0.2468139514080059382, -4.863684402402743245 ) ) ;
#25301 = ORIENTED_EDGE ( 'NONE', *, *, #17452, .T. ) ;
#25303 = CARTESIAN_POINT ( 'NONE',  ( 0.1825688514504806015, 0.5999999999999995337, 3.931742364880953744 ) ) ;
#25302 = CARTESIAN_POINT ( 'NONE',  ( 80.98905497205693393, 62.76708948751929995, -3.312281065658535528 ) ) ;
#25304 = CARTESIAN_POINT ( 'NONE',  ( -70.00729340478747531, -45.91674883463290513, 9.958481521799541270 ) ) ;
#25305 = DIRECTION ( 'NONE',  ( -5.786005779812646808E-17, 1.000000000000000000, 0.000000000000000000 ) ) ;
#25306 = EDGE_CURVE ( 'NONE', #8047, #23544, #30788, .T. ) ;
#25307 = ORIENTED_EDGE ( 'NONE', *, *, #15714, .T. ) ;
#25308 = ADVANCED_FACE ( 'NONE', ( #14294 ), #36337, .F. ) ;
#25309 = CARTESIAN_POINT ( 'NONE',  ( -1.651164297088600907, -28.99801832941991364, 7.748216051605116839 ) ) ;
#25310 = ADVANCED_FACE ( 'NONE', ( #36537, #17369 ), #21104, .T. ) ;
#25311 = ORIENTED_EDGE ( 'NONE', *, *, #24838, .F. ) ;
#25312 = CARTESIAN_POINT ( 'NONE',  ( -75.23198901687325701, -4.970357482903310142, 9.028257795211104053 ) ) ;
#25313 = EDGE_CURVE ( 'NONE', #37415, #35661, #36140, .T. ) ;
#25314 = EDGE_LOOP ( 'NONE', ( #26170, #33830, #13203, #16767 ) ) ;
#25315 = CARTESIAN_POINT ( 'NONE',  ( 78.79648636889818647, 65.96905942459900984, -1.896863055073860771 ) ) ;
#25316 = CARTESIAN_POINT ( 'NONE',  ( 35.96230930003272164, -3.155107722808913717, 5.819186136643963891 ) ) ;
#25318 = CARTESIAN_POINT ( 'NONE',  ( 37.14829660986974602, -2.504506050704642384, 5.969554084226253998 ) ) ;
#25317 = CARTESIAN_POINT ( 'NONE',  ( 23.09208776549577280, 1.724322394091927668, 5.081303647213513131 ) ) ;
#25320 = ORIENTED_EDGE ( 'NONE', *, *, #2630, .F. ) ;
#25319 = VERTEX_POINT ( 'NONE', #5243 ) ;
#25321 = CARTESIAN_POINT ( 'NONE',  ( 81.60411730068122438, 64.94496191031744559, -2.665107514501070085 ) ) ;
#25322 = CARTESIAN_POINT ( 'NONE',  ( -26.44874870218064089, -26.64985754041175525, 6.700000000000000178 ) ) ;
#25324 = CARTESIAN_POINT ( 'NONE',  ( 85.30708422457949780, 2.536758677189234756, -2.233489723537867011 ) ) ;
#25323 = CARTESIAN_POINT ( 'NONE',  ( 4.886497164546935501, -28.38302832708262713, 7.652160403243383868 ) ) ;
#25325 = DIRECTION ( 'NONE',  ( 1.000000000000000000, 0.000000000000000000, 0.000000000000000000 ) ) ;
#25326 = CARTESIAN_POINT ( 'NONE',  ( -75.45330471031414277, 33.71485196875532608, 15.50000000000000000 ) ) ;
#25327 = CARTESIAN_POINT ( 'NONE',  ( 71.62240613637702324, 61.07494268190700382, 3.699617110277040766 ) ) ;
#25328 = CARTESIAN_POINT ( 'NONE',  ( 23.89361308182833454, 3.044991201845574480, -3.758575451611194662 ) ) ;
#25329 = VERTEX_POINT ( 'NONE', #5451 ) ;
#25330 = AXIS2_PLACEMENT_3D ( 'NONE', #8602, #5527, #20549 ) ;
#25331 = CARTESIAN_POINT ( 'NONE',  ( 21.85643539959778892, -10.77729622265174392, -9.134175241038137827 ) ) ;
#25332 = CARTESIAN_POINT ( 'NONE',  ( -57.80924547062588204, 32.30639590073213441, -4.182592178550135209 ) ) ;
#25333 = CARTESIAN_POINT ( 'NONE',  ( -0.8786759135921904385, -24.55319635012989110, 6.800000000000000711 ) ) ;
#25334 = CARTESIAN_POINT ( 'NONE',  ( 81.40473435056813400, 64.45019880697493875, 3.071899782094677622 ) ) ;
#25335 = VECTOR ( 'NONE', #26258, 1000.000000000000000 ) ;
#25336 = CARTESIAN_POINT ( 'NONE',  ( 86.29974207331044056, 1.340767688666749446, -5.501321414410665689 ) ) ;
#25337 = ORIENTED_EDGE ( 'NONE', *, *, #31062, .F. ) ;
#25338 = CARTESIAN_POINT ( 'NONE',  ( -81.80090188080514224, -5.603160304130404334, -0.6545554231109831367 ) ) ;
#25339 = CARTESIAN_POINT ( 'NONE',  ( 33.10412314342393358, -3.384999426498728425, 5.361320240025687411 ) ) ;
#25340 = CARTESIAN_POINT ( 'NONE',  ( 33.68702248893509221, -3.103532886746783070, -5.464072601754253355 ) ) ;
#25341 = CARTESIAN_POINT ( 'NONE',  ( -1.659519015307392209, -30.57436305425760281, 7.387053503561888057 ) ) ;
#25342 = CARTESIAN_POINT ( 'NONE',  ( -1.339380734913657500, -27.83505459351727396, 7.750000000000002665 ) ) ;
#25343 = CARTESIAN_POINT ( 'NONE',  ( -1.292372527722988274, -31.18345358561926162, 7.774064877406527074 ) ) ;
#25344 = CARTESIAN_POINT ( 'NONE',  ( 33.45832265597695709, -3.170157842402876014, 5.428378461693221801 ) ) ;
#25345 = VERTEX_POINT ( 'NONE', #11396 ) ;
#25346 = CARTESIAN_POINT ( 'NONE',  ( 37.17543001156804650, -2.565671956813902810, 5.981153472165249063 ) ) ;
#25347 = CARTESIAN_POINT ( 'NONE',  ( 1.700390093233090871, -29.56993018339339940, 7.750000000000000888 ) ) ;
#25348 = CARTESIAN_POINT ( 'NONE',  ( 66.55026548882318593, 57.88912323611526034, -3.999530551066472039 ) ) ;
#25349 = EDGE_CURVE ( 'NONE', #18928, #19595, #4838, .T. ) ;
#25350 = AXIS2_PLACEMENT_3D ( 'NONE', #17249, #20543, #8390 ) ;
#25351 = EDGE_LOOP ( 'NONE', ( #24539, #20231, #5341, #26979 ) ) ;
#25352 = AXIS2_PLACEMENT_3D ( 'NONE', #39969, #30725, #5388 ) ;
#25353 = CARTESIAN_POINT ( 'NONE',  ( -55.71184120586745792, 30.71742687230118207, 1.474814583819915370 ) ) ;
#25355 = EDGE_CURVE ( 'NONE', #38144, #33085, #39404, .T. ) ;
#25354 = CARTESIAN_POINT ( 'NONE',  ( -77.15111496589565832, 10.95266906899447434, -7.837837878649032142 ) ) ;
#25356 = CARTESIAN_POINT ( 'NONE',  ( 4.935900671829004160, -28.52514296371000668, 6.863904403958575706 ) ) ;
#25357 = ORIENTED_EDGE ( 'NONE', *, *, #12980, .F. ) ;
#25358 = FACE_BOUND ( 'NONE', #5537, .T. ) ;
#25359 = DIRECTION ( 'NONE',  ( 0.000000000000000000, 0.000000000000000000, 1.000000000000000000 ) ) ;
#25360 = ORIENTED_EDGE ( 'NONE', *, *, #13429, .F. ) ;
#25361 = CARTESIAN_POINT ( 'NONE',  ( 22.66006657518957468, 4.460635658965687256, 3.191315208006852089 ) ) ;
#25362 = VECTOR ( 'NONE', #5442, 1000.000000000000000 ) ;
#25363 = CARTESIAN_POINT ( 'NONE',  ( 80.37799020243581083, 66.31529150154180741, -1.204231967108630785 ) ) ;
#25364 = CARTESIAN_POINT ( 'NONE',  ( 80.02704812381016097, 64.10187485078017744, 3.679799701112132837 ) ) ;
#25365 = ORIENTED_EDGE ( 'NONE', *, *, #24789, .F. ) ;
#25366 = CARTESIAN_POINT ( 'NONE',  ( 76.98341904138477787, 61.29654188154459860, -3.753756190332446785 ) ) ;
#25367 = B_SPLINE_CURVE_WITH_KNOTS ( 'NONE', 3,
 ( #28600, #25512, #18708, #19536, #35204, #38058, #12737, #611, #37636, #25713 ),
 .UNSPECIFIED., .F., .F.,
 ( 4, 2, 2, 2, 4 ),
 ( 0.001566344281586673362, 0.001957551653609702468, 0.002348759025632731357, 0.002739966397655760246, 0.003131173769678789135 ),
 .UNSPECIFIED. ) ;
#25369 = CARTESIAN_POINT ( 'NONE',  ( 5.651251297819362307, -26.64985754041175525, 6.700000000000000178 ) ) ;
#25368 = CARTESIAN_POINT ( 'NONE',  ( 3.907524105502494738, -32.26773122059653076, 7.785096263473212375 ) ) ;
#25370 = CARTESIAN_POINT ( 'NONE',  ( 16.22818509040511969, 10.38736679505083416, -2.694565954548105324 ) ) ;
#25371 = CARTESIAN_POINT ( 'NONE',  ( 81.29658979812199959, 62.90761208998645060, -3.189931650267181507 ) ) ;
#25372 = CARTESIAN_POINT ( 'NONE',  ( 78.21991615976332923, 63.09003589986990335, 3.816136337383044808 ) ) ;
#25373 = ORIENTED_EDGE ( 'NONE', *, *, #17231, .T. ) ;
#25374 = LINE ( 'NONE', #24969, #15510 ) ;
#25375 = CARTESIAN_POINT ( 'NONE',  ( -32.87867591359218977, -24.55319635012989110, 6.800000000000000711 ) ) ;
#25376 = CARTESIAN_POINT ( 'NONE',  ( 80.56094004998632840, 66.12977872868221141, 1.831286414254332806 ) ) ;
#25378 = CARTESIAN_POINT ( 'NONE',  ( -70.92837670882107659, 15.04836564048558500, -3.784187430299790211 ) ) ;
#25377 = CARTESIAN_POINT ( 'NONE',  ( -38.87867591359218977, -26.64985754041175525, 6.800000000000000711 ) ) ;
#25379 = CARTESIAN_POINT ( 'NONE',  ( 29.08816165369256268, -2.077165169587669613, 5.788842218736271583 ) ) ;
#25380 = ADVANCED_FACE ( 'NONE', ( #8106 ), #20674, .F. ) ;
#25381 = DIRECTION ( 'NONE',  ( -0.000000000000000000, -0.000000000000000000, -1.000000000000000000 ) ) ;
#25382 = DIRECTION ( 'NONE',  ( 1.000000000000000000, 0.000000000000000000, -0.000000000000000000 ) ) ;
#25383 = CARTESIAN_POINT ( 'NONE',  ( -64.09407456991031893, 35.62175799955464583, 4.126536650001270345 ) ) ;
#25384 = LINE ( 'NONE', #13223, #39918 ) ;
#25385 = VECTOR ( 'NONE', #34736, 1000.000000000000000 ) ;
#25386 = CARTESIAN_POINT ( 'NONE',  ( -0.6412884647684967687, -32.03499445358951903, 6.969307238440504371 ) ) ;
#25387 = AXIS2_PLACEMENT_3D ( 'NONE', #10744, #7671, #20223 ) ;
#25388 = PLANE ( 'NONE',  #5876 ) ;
#25389 = CARTESIAN_POINT ( 'NONE',  ( 36.17107013121489700, -3.462217916649524607, -5.816204344453734798 ) ) ;
#25390 = CARTESIAN_POINT ( 'NONE',  ( 79.42141780276817542, 60.69055068925465690, -2.271081754790353457 ) ) ;
#25391 = DIRECTION ( 'NONE',  ( 0.9396926207859135349, -0.3420201433256548351, 0.000000000000000000 ) ) ;
#25392 = CARTESIAN_POINT ( 'NONE',  ( 33.96533676093090293, -3.130127305233405099, -5.507510274953758334 ) ) ;
#25393 = DIRECTION ( 'NONE',  ( -0.000000000000000000, -0.000000000000000000, 1.000000000000000000 ) ) ;
#25394 = CARTESIAN_POINT ( 'NONE',  ( -78.80493796903779469, 10.24293490670538986, 7.984127664817240344 ) ) ;
#25395 = AXIS2_PLACEMENT_3D ( 'NONE', #38772, #10760, #10567 ) ;
#25396 = DIRECTION ( 'NONE',  ( -0.000000000000000000, -0.000000000000000000, 1.000000000000000000 ) ) ;
#25397 = EDGE_CURVE ( 'NONE', #8362, #142, #15313, .T. ) ;
#25398 = CARTESIAN_POINT ( 'NONE',  ( 0.4238093638620683556, -32.72117464255529029, 7.754798119455333705 ) ) ;
#25399 = ORIENTED_EDGE ( 'NONE', *, *, #25760, .F. ) ;
#25400 = ORIENTED_EDGE ( 'NONE', *, *, #20262, .F. ) ;
#25401 = CARTESIAN_POINT ( 'NONE',  ( -70.92837670882107659, 28.72470171467712063, 6.406751979251626317 ) ) ;
#25402 = CARTESIAN_POINT ( 'NONE',  ( 67.88769211468458309, 58.75904380331535037, -3.964697573200774539 ) ) ;
#25403 = ORIENTED_EDGE ( 'NONE', *, *, #23301, .F. ) ;
#25404 = CYLINDRICAL_SURFACE ( 'NONE', #35133, 3.399999999999999911 ) ;
#25406 = EDGE_CURVE ( 'NONE', #18768, #651, #11864, .T. ) ;
#25405 = CYLINDRICAL_SURFACE ( 'NONE', #8787, 0.09010775117052882699 ) ;
#25407 = CARTESIAN_POINT ( 'NONE',  ( 24.15678335194577286, 2.895156585529552906, 3.814851139992612161 ) ) ;
#25408 = CARTESIAN_POINT ( 'NONE',  ( 3.582330644718626722, -26.61893302209879408, 6.880828092187098122 ) ) ;
#25409 = DIRECTION ( 'NONE',  ( 0.000000000000000000, 0.000000000000000000, 1.000000000000000000 ) ) ;
#25410 = ORIENTED_EDGE ( 'NONE', *, *, #29699, .F. ) ;
#25411 = FACE_OUTER_BOUND ( 'NONE', #18747, .T. ) ;
#25412 = EDGE_LOOP ( 'NONE', ( #31627, #33976, #35049, #21550 ) ) ;
#25413 = CARTESIAN_POINT ( 'NONE',  ( 0.4697380470346541603, -26.29342357708423350, 7.700536657684214248 ) ) ;
#25414 = VERTEX_POINT ( 'NONE', #24588 ) ;
#25415 = CARTESIAN_POINT ( 'NONE',  ( 78.32432613507506858, 65.79895565947732905, -1.640065189519639199 ) ) ;
#25417 = LINE ( 'NONE', #9965, #5255 ) ;
#25416 = CARTESIAN_POINT ( 'NONE',  ( 25.29953812343164543, 0.8105978175163669475, 4.611665186302273511 ) ) ;
#25418 = CIRCLE ( 'NONE', #18916, 0.1000000000000028644 ) ;
#25419 = CARTESIAN_POINT ( 'NONE',  ( 81.57183863170791938, 63.40013557971743552, -3.079343812547459702 ) ) ;
#25420 = CARTESIAN_POINT ( 'NONE',  ( 80.27814043029276547, 62.51814696698978935, 3.475409704257726329 ) ) ;
#25421 = VECTOR ( 'NONE', #2717, 1000.000000000000000 ) ;
#25422 = CARTESIAN_POINT ( 'NONE',  ( 81.74784679736075077, 61.69507302169112251, 1.000000000000000000 ) ) ;
#25423 = CARTESIAN_POINT ( 'NONE',  ( -64.08758708073990817, 43.25085652376020562, 2.908220996737135966 ) ) ;
#25424 = CARTESIAN_POINT ( 'NONE',  ( 23.96136931976388951, 3.582231692328178063, -3.646207630380492226 ) ) ;
#25425 = LINE ( 'NONE', #38170, #32533 ) ;
#25426 = VERTEX_POINT ( 'NONE', #15731 ) ;
#25427 = CARTESIAN_POINT ( 'NONE',  ( -73.04279461669972306, 7.303834032481013594, 9.776029631287352473 ) ) ;
#25428 = CARTESIAN_POINT ( 'NONE',  ( 21.77915531863882848, 0.2033464020057170196, -8.424740673328486196 ) ) ;
#25429 = EDGE_LOOP ( 'NONE', ( #232, #2329, #26745, #24604 ) ) ;
#25430 = CARTESIAN_POINT ( 'NONE',  ( -0.06090154667645011205, -32.58437486080601531, 7.778495531946292729 ) ) ;
#25431 = CARTESIAN_POINT ( 'NONE',  ( -80.69318187898312544, 11.48007516437627196, -2.193839972823662166 ) ) ;
#25432 = CARTESIAN_POINT ( 'NONE',  ( 3.419291884707112761, -26.52109817239846734, 7.700536657684210695 ) ) ;
#25433 = CARTESIAN_POINT ( 'NONE',  ( 36.49343378766320711, -3.559996503287254033, -5.796408034747916993 ) ) ;
#25434 = CARTESIAN_POINT ( 'NONE',  ( -0.02684669743237798334, -25.18051837188491149, 7.754798119455333705 ) ) ;
#25435 = CARTESIAN_POINT ( 'NONE',  ( 20.51617099466335858, 5.905244554751226005, 3.408442687824492445 ) ) ;
#25436 = CARTESIAN_POINT ( 'NONE',  ( 5.196021075228325792, -29.74475591867008362, 7.006908160621407866 ) ) ;
#25437 = ADVANCED_FACE ( 'NONE', ( #12839 ), #31591, .F. ) ;
#25438 = CARTESIAN_POINT ( 'NONE',  ( -59.99245622168610481, 24.84364830758654463, -9.341017543843770810 ) ) ;
#25439 = EDGE_CURVE ( 'NONE', #14437, #28633, #3415, .T. ) ;
#25440 = CIRCLE ( 'NONE', #35337, 7.744449365083023729 ) ;
#25441 = DIRECTION ( 'NONE',  ( 0.9848077530122077983, -0.1736481776669321353, 0.000000000000000000 ) ) ;
#25442 = CARTESIAN_POINT ( 'NONE',  ( 32.10354844262580087, -3.770861253239083055, -4.822966298526184303 ) ) ;
#25443 = DIRECTION ( 'NONE',  ( 0.000000000000000000, 1.000000000000000000, 0.000000000000000000 ) ) ;
#25444 = ORIENTED_EDGE ( 'NONE', *, *, #19262, .T. ) ;
#25445 = B_SPLINE_CURVE_WITH_KNOTS ( 'NONE', 3,
 ( #19429, #3807, #35298, #22534, #9545, #10144, #22735, #16326, #28900, #13243, #905, #19635, #19026, #38548, #25809, #6874, #102, #15925, #32209, #22334, #28490, #15730, #35098, #4009, #16526 ),
 .UNSPECIFIED., .F., .F.,
 ( 4, 3, 3, 3, 3, 3, 3, 3, 4 ),
 ( 6.468151674593381644E-05, 9.076621574722021054E-05, 0.0001210204262067969501, 0.0001512763324577428333, 0.0001815301820994210237, 0.0002117781465860714375, 0.0002420274594459746113, 0.0002722905548971154633, 0.0002816827545175555896 ),
 .UNSPECIFIED. ) ;
#25446 = AXIS2_PLACEMENT_3D ( 'NONE', #32612, #13859, #16932 ) ;
#25447 = CARTESIAN_POINT ( 'NONE',  ( 66.89278707744533392, 57.85779714042387667, 3.998112125421894980 ) ) ;
#25448 = AXIS2_PLACEMENT_3D ( 'NONE', #24675, #11891, #22418 ) ;
#25449 = VECTOR ( 'NONE', #25396, 1000.000000000000000 ) ;
#25450 = B_SPLINE_CURVE_WITH_KNOTS ( 'NONE', 3,
 ( #31964, #13206, #32172, #29064, #4162, #4558, #19793, #16679, #871, #14004, #19985, #17084, #1277, #10512, #669, #35657, #38511, #10312, #19599 ),
 .UNSPECIFIED., .F., .F.,
 ( 4, 3, 3, 3, 3, 3, 4 ),
 ( 0.000000000000000000, 2.546128104244556401E-05, 5.711050680484009269E-05, 8.113074941675658795E-05, 0.0001053129305727048420, 0.0001360598016347089507, 0.0001612931755713726417 ),
 .UNSPECIFIED. ) ;
#25451 = DIRECTION ( 'NONE',  ( 0.000000000000000000, 1.000000000000000000, 0.000000000000000000 ) ) ;
#25452 = CARTESIAN_POINT ( 'NONE',  ( 87.41819985312852737, -0.4314763451276128481, -5.556477619079806196 ) ) ;
#25453 = EDGE_CURVE ( 'NONE', #7986, #12843, #17910, .T. ) ;
#25454 = ORIENTED_EDGE ( 'NONE', *, *, #24683, .F. ) ;
#25455 = CARTESIAN_POINT ( 'NONE',  ( 24.76215755375829275, 2.615058120370138628, 3.935479537194128241 ) ) ;
#25456 = CARTESIAN_POINT ( 'NONE',  ( -70.79763891489490391, -21.78299143688767359, 6.000000000000034639 ) ) ;
#25457 = CARTESIAN_POINT ( 'NONE',  ( 1.161761687666269749, -26.12572513379734218, 7.784725160561909441 ) ) ;
#25458 = ORIENTED_EDGE ( 'NONE', *, *, #28912, .F. ) ;
#25459 = DIRECTION ( 'NONE',  ( 0.000000000000000000, 1.000000000000000000, 0.000000000000000000 ) ) ;
#25460 = UNCERTAINTY_MEASURE_WITH_UNIT (LENGTH_MEASURE( 1.000000000000000082E-05 ), #39616, 'distance_accuracy_value', 'NONE');
#25461 = VERTEX_POINT ( 'NONE', #31185 ) ;
#25462 = CARTESIAN_POINT ( 'NONE',  ( 80.26059561567515743, 63.13455243780963144, -3.653685850874238028 ) ) ;
#25463 = DIRECTION ( 'NONE',  ( 1.000000000000000000, 0.000000000000000000, 0.000000000000000000 ) ) ;
#25464 = CARTESIAN_POINT ( 'NONE',  ( 80.89855423268610934, 61.90964448260509556, 2.818206040476791241 ) ) ;
#25466 = ORIENTED_EDGE ( 'NONE', *, *, #32833, .T. ) ;
#25465 = CARTESIAN_POINT ( 'NONE',  ( 2.510480264938812045, -26.15794710555851310, 7.387053503561887169 ) ) ;
#25467 = VECTOR ( 'NONE', #24244, 1000.000000000000000 ) ;
#25468 = CARTESIAN_POINT ( 'NONE',  ( -57.66410233176053879, 30.21301966603896361, 4.063147710751544572 ) ) ;
#25469 = B_SPLINE_CURVE_WITH_KNOTS ( 'NONE', 3,
 ( #37839, #34794, #6572, #400 ),
 .UNSPECIFIED., .F., .F.,
 ( 4, 4 ),
 ( 8.673617379884035472E-19, 2.475319317933456399E-05 ),
 .UNSPECIFIED. ) ;
#25470 = CARTESIAN_POINT ( 'NONE',  ( 0.9463359558106179126, -32.98775010660822460, 6.877402575842992860 ) ) ;
#25471 = CARTESIAN_POINT ( 'NONE',  ( 1.700390093233090871, -29.56993018339339940, 27.90461065042423527 ) ) ;
#25472 = CARTESIAN_POINT ( 'NONE',  ( -54.79610818216035995, 31.51396769785353058, 1.028877969214415433 ) ) ;
#25473 = CIRCLE ( 'NONE', #21542, 0.1000000000000028644 ) ;
#25474 = CARTESIAN_POINT ( 'NONE',  ( 22.00805480815993675, 5.522815187245081248, -3.139564157486774754 ) ) ;
#25475 = ORIENTED_EDGE ( 'NONE', *, *, #6764, .T. ) ;
#25476 = PLANE ( 'NONE',  #34755 ) ;
#25477 = VERTEX_POINT ( 'NONE', #19228 ) ;
#25478 = CARTESIAN_POINT ( 'NONE',  ( -1.346119371218626792, -31.29294500718514271, 6.894806418505347700 ) ) ;
#25479 = CARTESIAN_POINT ( 'NONE',  ( -62.92837670882106238, -23.80776546975053520, -6.000000000000000000 ) ) ;
#25480 = CARTESIAN_POINT ( 'NONE',  ( -78.79614016259206721, -5.365327593382188454, -7.951721105412269175 ) ) ;
#25481 = DIRECTION ( 'NONE',  ( -0.000000000000000000, -0.000000000000000000, 1.000000000000000000 ) ) ;
#25482 = CARTESIAN_POINT ( 'NONE',  ( 78.94073822560471854, 66.07870154842754573, 1.754135932968020173 ) ) ;
#25483 = CARTESIAN_POINT ( 'NONE',  ( 85.50394501772831291, 1.137698216002840157, 5.721642786829533200 ) ) ;
#25484 = CARTESIAN_POINT ( 'NONE',  ( -0.02105859379946962290, -32.61732735699371943, 7.720710062488898906 ) ) ;
#25485 = ORIENTED_EDGE ( 'NONE', *, *, #16621, .F. ) ;
#25486 = CARTESIAN_POINT ( 'NONE',  ( -66.12008681484671513, 35.44165918782573499, 8.117242773420016988 ) ) ;
#25487 = CARTESIAN_POINT ( 'NONE',  ( -1.078675913592196167, -26.64985754041175525, 6.800000000000000711 ) ) ;
#25488 = EDGE_CURVE ( 'NONE', #20646, #12996, #21516, .T. ) ;
#25489 = EDGE_CURVE ( 'NONE', #34205, #19079, #24508, .T. ) ;
#25490 = CARTESIAN_POINT ( 'NONE',  ( 1.694962496619858427, -26.16992440333174130, 7.763628509615287498 ) ) ;
#25491 = CARTESIAN_POINT ( 'NONE',  ( -1.799609906766908685, -29.56993018339339940, 6.929570838012926615 ) ) ;
#25492 = CARTESIAN_POINT ( 'NONE',  ( 4.674598849011252000, -27.92248298331306700, 7.785172627573962778 ) ) ;
#25493 = CARTESIAN_POINT ( 'NONE',  ( -67.83000114521873058, 27.33924089054923101, 15.50000000000000000 ) ) ;
#25494 = CARTESIAN_POINT ( 'NONE',  ( 36.91070730316501169, -2.639519445664956887, 5.967206582125117009 ) ) ;
#25495 = VECTOR ( 'NONE', #18271, 1000.000000000000000 ) ;
#25496 = CARTESIAN_POINT ( 'NONE',  ( 85.68874278272487288, 2.108061670072472360, -3.902156445801064244 ) ) ;
#25497 = ORIENTED_EDGE ( 'NONE', *, *, #29522, .F. ) ;
#25499 = CARTESIAN_POINT ( 'NONE',  ( -24.97867591359219475, -24.55319635012989110, 6.700000000000000178 ) ) ;
#25498 = CARTESIAN_POINT ( 'NONE',  ( 80.38786582577539264, 64.30167536105096815, -3.588566286536287731 ) ) ;
#25500 = CARTESIAN_POINT ( 'NONE',  ( -1.347083181716895339, -31.26079133133813315, 7.785593909369612931 ) ) ;
#25501 = EDGE_LOOP ( 'NONE', ( #31852, #5057, #29384, #38855 ) ) ;
#25502 = CARTESIAN_POINT ( 'NONE',  ( 2.912097039036203761, -32.85349084633266159, 7.638132480492516585 ) ) ;
#25503 = AXIS2_PLACEMENT_3D ( 'NONE', #12357, #14824, #21433 ) ;
#25504 = DIRECTION ( 'NONE',  ( -1.000000000000000000, -5.421010862427517240E-17, 0.000000000000000000 ) ) ;
#25505 = ORIENTED_EDGE ( 'NONE', *, *, #9860, .F. ) ;
#25506 = CARTESIAN_POINT ( 'NONE',  ( 1.551251297819356001, -26.64985754041175525, 6.700000000000000178 ) ) ;
#25507 = ORIENTED_EDGE ( 'NONE', *, *, #8860, .F. ) ;
#25508 = CARTESIAN_POINT ( 'NONE',  ( -73.80648002973117627, -3.552836831368545223, 9.577764321634322897 ) ) ;
#25510 = ORIENTED_EDGE ( 'NONE', *, *, #7116, .T. ) ;
#25509 = EDGE_LOOP ( 'NONE', ( #1606, #39045, #19964, #19661 ) ) ;
#25511 = CARTESIAN_POINT ( 'NONE',  ( 78.61848929481175219, 66.00753381999014380, -1.284346554836964582 ) ) ;
#25512 = CARTESIAN_POINT ( 'NONE',  ( -71.05898243613420107, 0.2170276505044492765, 6.000000000000012434 ) ) ;
#25513 = CARTESIAN_POINT ( 'NONE',  ( 24.20720853044049292, 2.174628992932770899, 4.300592713746694606 ) ) ;
#25515 = ORIENTED_EDGE ( 'NONE', *, *, #38522, .T. ) ;
#25514 = ORIENTED_EDGE ( 'NONE', *, *, #36865, .T. ) ;
#25516 = CARTESIAN_POINT ( 'NONE',  ( 80.02452723347238361, 66.12521016146372688, -2.110636331688537037 ) ) ;
#25517 = CARTESIAN_POINT ( 'NONE',  ( -42.83131703149249603, -32.06993018339340296, 6.800000000000000711 ) ) ;
#25518 = CARTESIAN_POINT ( 'NONE',  ( 4.695449071104084382, -27.96066553437519886, 6.864651958020304257 ) ) ;
#25519 = VECTOR ( 'NONE', #11815, 1000.000000000000000 ) ;
#25521 = CYLINDRICAL_SURFACE ( 'NONE', #11116, 0.1000000000000028644 ) ;
#25520 = CARTESIAN_POINT ( 'NONE',  ( 14.73500979046645831, 12.83520685450572074, -2.502377855999197820 ) ) ;
#25522 = CARTESIAN_POINT ( 'NONE',  ( 3.793404844923233377, -32.38367570474625978, 7.387053503561885393 ) ) ;
#25523 = CARTESIAN_POINT ( 'NONE',  ( 5.181826490399478402, -29.15396049260679945, 7.398879060202674829 ) ) ;
#25524 = CARTESIAN_POINT ( 'NONE',  ( 70.76671532128065678, 59.91573877893261368, 3.942344351592494966 ) ) ;
#25525 = CARTESIAN_POINT ( 'NONE',  ( 23.65416832550485893, 3.201561871976233320, -3.718035610939157465 ) ) ;
#25526 = ORIENTED_EDGE ( 'NONE', *, *, #8074, .F. ) ;
#25527 = EDGE_CURVE ( 'NONE', #9233, #34426, #5119, .T. ) ;
#25528 = ORIENTED_EDGE ( 'NONE', *, *, #15704, .F. ) ;
#25529 = AXIS2_PLACEMENT_3D ( 'NONE', #6141, #9412, #34577 ) ;
#25530 = CARTESIAN_POINT ( 'NONE',  ( 21.85643539959781023, -11.34362525346678474, 8.214566034197922306 ) ) ;
#25531 = EDGE_CURVE ( 'NONE', #31915, #7027, #22127, .T. ) ;
#25532 = CARTESIAN_POINT ( 'NONE',  ( -64.08758708074093136, 41.04287353446839859, -3.000000000000000000 ) ) ;
#25533 = LINE ( 'NONE', #5982, #39910 ) ;
#25534 = CARTESIAN_POINT ( 'NONE',  ( 79.96642255694898438, 65.80764937176724061, 2.611089443243009178 ) ) ;
#25535 = CARTESIAN_POINT ( 'NONE',  ( 87.14327233159831110, 0.3315334873356338141, 5.689878492676547772 ) ) ;
#25536 = ORIENTED_EDGE ( 'NONE', *, *, #250, .T. ) ;
#25537 = EDGE_CURVE ( 'NONE', #38454, #11061, #10683, .T. ) ;
#25538 = CARTESIAN_POINT ( 'NONE',  ( 0.5713750229309363382, -32.77700439067807281, 7.703977250142848732 ) ) ;
#25539 = VECTOR ( 'NONE', #20493, 1000.000000000000000 ) ;
#25540 = CARTESIAN_POINT ( 'NONE',  ( 14.85966502733631778, -5.942515497032718308, 2.521215392215149009 ) ) ;
#25541 = EDGE_CURVE ( 'NONE', #34099, #19152, #29103, .T. ) ;
#25542 = CARTESIAN_POINT ( 'NONE',  ( 33.62812902532535020, -1.230530048054541359, -5.454880852412670400 ) ) ;
#25543 = CARTESIAN_POINT ( 'NONE',  ( 5.100200997230469824, -29.53407189201577410, 7.691066658568944447 ) ) ;
#25544 = CARTESIAN_POINT ( 'NONE',  ( 5.140791489254627145, -28.92678305073006584, 7.695279973900954751 ) ) ;
#25545 = CARTESIAN_POINT ( 'NONE',  ( -73.39219586654201066, -0.5165367281780630648, 10.89398956819519348 ) ) ;
#25546 = ORIENTED_EDGE ( 'NONE', *, *, #21640, .F. ) ;
#25547 = FACE_OUTER_BOUND ( 'NONE', #40679, .T. ) ;
#25548 = CYLINDRICAL_SURFACE ( 'NONE', #21951, 0.1000000000000028644 ) ;
#25549 = VERTEX_POINT ( 'NONE', #26224 ) ;
#25550 = ORIENTED_EDGE ( 'NONE', *, *, #35860, .F. ) ;
#25551 = CARTESIAN_POINT ( 'NONE',  ( 35.21959567110821610, -1.049937720980187672, 5.413415876260859960 ) ) ;
#25552 = CIRCLE ( 'NONE', #22984, 3.000000000000002220 ) ;
#25553 = CARTESIAN_POINT ( 'NONE',  ( 1.657039758437295340, -33.05528407258798040, 7.785096263473211486 ) ) ;
#25554 = CARTESIAN_POINT ( 'NONE',  ( 66.68811621373450294, 57.96620201306357956, -3.998609561968404336 ) ) ;
#25555 = ORIENTED_EDGE ( 'NONE', *, *, #910, .T. ) ;
#25556 = CYLINDRICAL_SURFACE ( 'NONE', #10759, 12.38600677260393113 ) ;
#25557 = CARTESIAN_POINT ( 'NONE',  ( 3.011115207906999380, -26.32487479661073948, 7.754798119455333705 ) ) ;
#25558 = CARTESIAN_POINT ( 'NONE',  ( 2.293941986480968254, -26.12062633890310437, 7.636816916992233750 ) ) ;
#25559 = FACE_BOUND ( 'NONE', #20415, .T. ) ;
#25560 = ORIENTED_EDGE ( 'NONE', *, *, #6764, .F. ) ;
#25561 = CARTESIAN_POINT ( 'NONE',  ( 23.42426635392413914, 3.731876618793696920, 3.231681589700163393 ) ) ;
#25562 = CARTESIAN_POINT ( 'NONE',  ( 82.41151909044420165, 62.85445852417072388, -1.451695327222927379 ) ) ;
#25563 = CARTESIAN_POINT ( 'NONE',  ( 80.59816347408094828, 62.94305116675476341, 3.503057693382590099 ) ) ;
#25564 = CARTESIAN_POINT ( 'NONE',  ( 2.858160284951835717, -26.37311349386845549, 7.763628509615289275 ) ) ;
#25565 = ORIENTED_EDGE ( 'NONE', *, *, #12175, .F. ) ;
#25566 = ORIENTED_EDGE ( 'NONE', *, *, #14671, .T. ) ;
#25567 = CARTESIAN_POINT ( 'NONE',  ( 74.72645207833699033, 61.69672356374137223, -3.865308561588413738 ) ) ;
#25569 = CARTESIAN_POINT ( 'NONE',  ( -59.01947560891952804, 27.90920910948504385, -46.17089178453873188 ) ) ;
#25568 = DIRECTION ( 'NONE',  ( 0.4582725098355704407, -0.8888117386314197121, 3.083685177455368914E-15 ) ) ;
#25570 = CARTESIAN_POINT ( 'NONE',  ( 15.71090316427554967, 10.60011360582976003, -2.658464427050829304 ) ) ;
#25571 = CARTESIAN_POINT ( 'NONE',  ( 81.36058090587512481, 62.33601367849696118, -2.816708194897771911 ) ) ;
#25572 = CARTESIAN_POINT ( 'NONE',  ( 77.53347081925228679, 60.09046002684877408, 2.805892758502874340 ) ) ;
#25573 = EDGE_LOOP ( 'NONE', ( #6163, #14728 ) ) ;
#25574 = FACE_OUTER_BOUND ( 'NONE', #36958, .T. ) ;
#25575 = VECTOR ( 'NONE', #39939, 1000.000000000000114 ) ;
#25576 = CARTESIAN_POINT ( 'NONE',  ( -52.01549048184568846, -30.94667987854474234, 6.800000000000000711 ) ) ;
#25577 = CARTESIAN_POINT ( 'NONE',  ( 78.94658775073220625, 66.18447242754098170, 1.227604746834740856 ) ) ;
#25579 = CARTESIAN_POINT ( 'NONE',  ( 14.38908526677529842, 8.635444969966599160, 3.482730074327033520 ) ) ;
#25578 = CARTESIAN_POINT ( 'NONE',  ( -0.9707194483615372294, -31.83160614747662720, 7.638132480492516585 ) ) ;
#25580 = CARTESIAN_POINT ( 'NONE',  ( 27.99192205930350497, 2.110044335382625924, -3.171593750069938711 ) ) ;
#25581 = CARTESIAN_POINT ( 'NONE',  ( -1.699482881577310422, -29.59931989509443895, 7.661510568013095934 ) ) ;
#25582 = DIRECTION ( 'NONE',  ( -1.000000000000000000, 0.000000000000000000, 0.000000000000000000 ) ) ;
#25583 = EDGE_CURVE ( 'NONE', #26604, #5603, #8015, .T. ) ;
#25584 = CARTESIAN_POINT ( 'NONE',  ( 4.688455439100348343, -31.36368888288187406, 7.785593909369613819 ) ) ;
#25585 = CARTESIAN_POINT ( 'NONE',  ( 14.77222811005485603, -4.461988841550141416, 2.511961482897715481 ) ) ;
#25586 = DIRECTION ( 'NONE',  ( 0.000000000000000000, 1.000000000000000000, 0.000000000000000000 ) ) ;
#25587 = EDGE_CURVE ( 'NONE', #37354, #6054, #16336, .T. ) ;
#25588 = FACE_OUTER_BOUND ( 'NONE', #11851, .T. ) ;
#25589 = CARTESIAN_POINT ( 'NONE',  ( 25.49148164000159156, 2.250841665744788500, -4.142222679967197507 ) ) ;
#25590 = FACE_OUTER_BOUND ( 'NONE', #9535, .T. ) ;
#25591 = CARTESIAN_POINT ( 'NONE',  ( 1.736346942945644400, -33.06974547922812491, 7.695279973900954751 ) ) ;
#25592 = CARTESIAN_POINT ( 'NONE',  ( 1.733559400163837250, -32.96977048603782379, 7.670860738520327793 ) ) ;
#25593 = CARTESIAN_POINT ( 'NONE',  ( 2.099095770640518666, -32.94647852641658403, 7.006423389747791219 ) ) ;
#25594 = CARTESIAN_POINT ( 'NONE',  ( 22.12509260470467609, -10.94958406946211760, -2.499999999999999556 ) ) ;
#25595 = DIRECTION ( 'NONE',  ( 0.000000000000000000, 0.000000000000000000, 1.000000000000000000 ) ) ;
#25596 = VERTEX_POINT ( 'NONE', #4199 ) ;
#25597 = CARTESIAN_POINT ( 'NONE',  ( 4.921324086407802056, -24.55319635012989110, 6.800000000000000711 ) ) ;
#25598 = CARTESIAN_POINT ( 'NONE',  ( 68.05544300132015678, 58.31078564718745127, -3.995571880668737474 ) ) ;
#25599 = CARTESIAN_POINT ( 'NONE',  ( 2.976261230439396499, -26.31076574427040526, 6.865554069792297653 ) ) ;
#25600 = ORIENTED_EDGE ( 'NONE', *, *, #11400, .F. ) ;
#25601 = FACE_OUTER_BOUND ( 'NONE', #22436, .T. ) ;
#25602 = VECTOR ( 'NONE', #1830, 1000.000000000000000 ) ;
#25603 = CARTESIAN_POINT ( 'NONE',  ( -71.89960098016555889, -42.46322148352267334, -1.682209783512703227 ) ) ;
#25604 = CARTESIAN_POINT ( 'NONE',  ( 24.48230801151231262, 2.778427030854781599, 3.854342034842722420 ) ) ;
#25605 = CARTESIAN_POINT ( 'NONE',  ( -1.434533901437197168, -28.25375393532444335, 6.876076431790004939 ) ) ;
#25606 = CARTESIAN_POINT ( 'NONE',  ( 3.558149082814241915, -26.60364649932381198, 6.867199677474203234 ) ) ;
#25607 = DIRECTION ( 'NONE',  ( 0.8660254037844449249, -0.4999999999999888423, -0.000000000000000000 ) ) ;
#25608 = EDGE_LOOP ( 'NONE', ( #22336, #26486, #24166, #32383 ) ) ;
#25609 = LINE ( 'NONE', #16330, #5041 ) ;
#25610 = CARTESIAN_POINT ( 'NONE',  ( 79.25894186866877078, 65.67357942822117423, 2.700485128497465137 ) ) ;
#25611 = EDGE_LOOP ( 'NONE', ( #36905, #39159, #20051, #32046 ) ) ;
#25612 = CARTESIAN_POINT ( 'NONE',  ( -1.233825218002540414, -31.30161613693384481, 7.257242401810563237 ) ) ;
#25613 = EDGE_LOOP ( 'NONE', ( #9471, #7444, #397, #24478 ) ) ;
#25614 = CARTESIAN_POINT ( 'NONE',  ( 80.06304181921890972, 62.74582375469539386, -3.589982250315065127 ) ) ;
#25616 = CARTESIAN_POINT ( 'NONE',  ( -1.657321944901828825, -30.10450465805885045, 6.887041543973312585 ) ) ;
#25615 = CARTESIAN_POINT ( 'NONE',  ( 22.32644494669605706, 0.2764816045299239300, 7.043421893595684047 ) ) ;
#25617 = CARTESIAN_POINT ( 'NONE',  ( 81.69067057342168425, 62.21317191938595670, -2.410848004503902242 ) ) ;
#25618 = CARTESIAN_POINT ( 'NONE',  ( 80.68211079047073042, 61.32331416546044522, 2.218931858625937004 ) ) ;
#25619 = VERTEX_POINT ( 'NONE', #38150 ) ;
#25620 = VECTOR ( 'NONE', #19007, 1000.000000000000000 ) ;
#25621 = CARTESIAN_POINT ( 'NONE',  ( 3.977772666037320715, -27.04534534285276592, 7.754798119455333705 ) ) ;
#25622 = CARTESIAN_POINT ( 'NONE',  ( -1.601964535056334960, -30.69171433492233092, 7.782861076432731728 ) ) ;
#25623 = CARTESIAN_POINT ( 'NONE',  ( -63.53025880882105980, 43.42181481381274466, 3.125110315362289892 ) ) ;
#25624 = CARTESIAN_POINT ( 'NONE',  ( 22.71016324673079012, -4.497379315063210647, 7.328459856909534054 ) ) ;
#25625 = CARTESIAN_POINT ( 'NONE',  ( 3.875507134935765041, -26.95672030760948346, 7.635761828346577573 ) ) ;
#25626 = EDGE_LOOP ( 'NONE', ( #666, #3836, #35017, #2375, #22999 ) ) ;
#25627 = CARTESIAN_POINT ( 'NONE',  ( -71.87772275130814137, 3.993544671651554800, 9.955241825054214289 ) ) ;
#25628 = CARTESIAN_POINT ( 'NONE',  ( 25.40522817991440618, 0.6234987413466189787, -4.602598919802544764 ) ) ;
#25629 = VERTEX_POINT ( 'NONE', #26422 ) ;
#25630 = CARTESIAN_POINT ( 'NONE',  ( -0.1425244880348677801, -32.54239410267695121, 7.766640943994648438 ) ) ;
#25631 = ORIENTED_EDGE ( 'NONE', *, *, #32328, .F. ) ;
#25632 = DIRECTION ( 'NONE',  ( 1.000000000000000000, 0.000000000000000000, 0.000000000000000000 ) ) ;
#25633 = AXIS2_PLACEMENT_3D ( 'NONE', #11517, #14415, #11311 ) ;
#25634 = EDGE_CURVE ( 'NONE', #2581, #2062, #32130, .T. ) ;
#25635 = CARTESIAN_POINT ( 'NONE',  ( 29.58584611389639463, -3.738994457646588998, -4.503545041254670700 ) ) ;
#25636 = CARTESIAN_POINT ( 'NONE',  ( 36.20088530600373389, -3.650368342384689324, -5.718075320652626026 ) ) ;
#25637 = CARTESIAN_POINT ( 'NONE',  ( 3.780365410620694977, -32.25950308696851465, 6.865312560952604670 ) ) ;
#25638 = CARTESIAN_POINT ( 'NONE',  ( 16.93205111601292856, 9.104991719096041436, 2.849054098494264498 ) ) ;
#25639 = CARTESIAN_POINT ( 'NONE',  ( -75.45330471031414277, 33.71485196875532608, 8.800414904976364028 ) ) ;
#25640 = LINE ( 'NONE', #38182, #7561 ) ;
#25641 = LINE ( 'NONE', #3245, #17721 ) ;
#25642 = CARTESIAN_POINT ( 'NONE',  ( 1.746581778429556975, -26.07022345230773652, 6.880608371227950215 ) ) ;
#25643 = CARTESIAN_POINT ( 'NONE',  ( 23.62990479565404556, 0.6233627752244329523, -5.429377995287568481 ) ) ;
#25644 = CARTESIAN_POINT ( 'NONE',  ( 33.57278938729775319, -0.3416013291472669855, -5.045988930500178604 ) ) ;
#25645 = DIRECTION ( 'NONE',  ( -0.3420201433256726542, 0.9396926207859070956, -0.000000000000000000 ) ) ;
#25646 = ORIENTED_EDGE ( 'NONE', *, *, #20824, .T. ) ;
#25647 = CARTESIAN_POINT ( 'NONE',  ( 66.73227421799262515, 57.84320248636868200, 3.999246569070631363 ) ) ;
#25648 = VECTOR ( 'NONE', #11000, 1000.000000000000000 ) ;
#25649 = CARTESIAN_POINT ( 'NONE',  ( 2.289108667884883985, -26.11979771739482459, 7.747520101777647383 ) ) ;
#25650 = CARTESIAN_POINT ( 'NONE',  ( 88.36457133188896762, -1.562442635866588381, -3.606418352999261945 ) ) ;
#25651 = DIRECTION ( 'NONE',  ( 1.000000000000000000, 0.000000000000000000, 0.000000000000000000 ) ) ;
#25652 = VERTEX_POINT ( 'NONE', #16527 ) ;
#25653 = CARTESIAN_POINT ( 'NONE',  ( -72.91739463649112452, 3.507283232836214015, -10.95474081624619167 ) ) ;
#25654 = EDGE_CURVE ( 'NONE', #38807, #24578, #13333, .T. ) ;
#25655 =( NAMED_UNIT ( * ) SI_UNIT ( $, .STERADIAN. ) SOLID_ANGLE_UNIT ( ) );
#25656 = CARTESIAN_POINT ( 'NONE',  ( -3.078675913592197944, -26.64985754041175525, 6.700000000000000178 ) ) ;
#25657 = CARTESIAN_POINT ( 'NONE',  ( -24.44874870218064089, -25.49307895267003587, 6.700000000000000178 ) ) ;
#25658 = VERTEX_POINT ( 'NONE', #29507 ) ;
#25659 = CARTESIAN_POINT ( 'NONE',  ( -6.348748702180634140, -26.64985754041175525, 6.700000000000000178 ) ) ;
#25660 = ORIENTED_EDGE ( 'NONE', *, *, #37274, .F. ) ;
#25661 = ORIENTED_EDGE ( 'NONE', *, *, #12675, .F. ) ;
#25662 = CARTESIAN_POINT ( 'NONE',  ( 80.87650043350832618, 61.69514696456053571, -2.603857329607536464 ) ) ;
#25663 = CYLINDRICAL_SURFACE ( 'NONE', #33234, 0.1000000000000028644 ) ;
#25664 = CARTESIAN_POINT ( 'NONE',  ( 81.04520860822712791, 61.30615853997439046, 1.682919622592479625 ) ) ;
#25666 = ORIENTED_EDGE ( 'NONE', *, *, #35615, .F. ) ;
#25665 = DIRECTION ( 'NONE',  ( -1.000000000000000000, -0.000000000000000000, -0.000000000000000000 ) ) ;
#25667 = DIRECTION ( 'NONE',  ( -0.2312332387574689563, -0.9728983447892853853, -0.000000000000000000 ) ) ;
#25668 = EDGE_CURVE ( 'NONE', #16321, #22181, #7269, .T. ) ;
#25669 = PLANE ( 'NONE',  #19915 ) ;
#25670 = CARTESIAN_POINT ( 'NONE',  ( 0.9556399531351862375, -32.98977626601526936, 6.872971584836693459 ) ) ;
#25671 = CARTESIAN_POINT ( 'NONE',  ( -1.793434212015915241, -29.46706035826072068, 7.771081512783700518 ) ) ;
#25672 = CARTESIAN_POINT ( 'NONE',  ( 21.85643539959775694, 4.302923821179891029, -14.48878861646959315 ) ) ;
#25673 = CARTESIAN_POINT ( 'NONE',  ( 23.74238088461279972, 3.559840393902792055, -3.189493409904875953 ) ) ;
#25674 = EDGE_LOOP ( 'NONE', ( #5188, #24598, #4603, #17471 ) ) ;
#25675 = CARTESIAN_POINT ( 'NONE',  ( -63.84700662236061675, 35.83977057131340871, -7.343444254795444159 ) ) ;
#25676 = VECTOR ( 'NONE', #11836, 1000.000000000000000 ) ;
#25677 = CARTESIAN_POINT ( 'NONE',  ( -0.5222078730473904695, -32.14287757506037480, 6.894806418505348589 ) ) ;
#25678 = CARTESIAN_POINT ( 'NONE',  ( -74.92283640148284007, 18.87330372387142674, 9.800414904976365804 ) ) ;
#25679 = CARTESIAN_POINT ( 'NONE',  ( -80.91065676098011750, -6.597313057213480825, -0.5950503846463365276 ) ) ;
#25680 = EDGE_CURVE ( 'NONE', #22934, #11656, #13244, .T. ) ;
#25681 = CARTESIAN_POINT ( 'NONE',  ( -0.02499863111512088884, -26.64024867341794334, 7.661510568013094158 ) ) ;
#25682 = DIRECTION ( 'NONE',  ( -0.000000000000000000, -0.000000000000000000, 1.000000000000000000 ) ) ;
#25683 = CARTESIAN_POINT ( 'NONE',  ( 79.64653587341234697, 65.62447382577090593, 2.816708194897748374 ) ) ;
#25684 = CARTESIAN_POINT ( 'NONE',  ( 86.70396871743868417, -0.5679530053852996918, -5.718564545587779158 ) ) ;
#25685 = CARTESIAN_POINT ( 'NONE',  ( 22.06617482514043616, 4.214940469348163354, -2.278054249745394166 ) ) ;
#25686 = CARTESIAN_POINT ( 'NONE',  ( 3.388683086819756163, -26.61871572696936994, 7.635761828346577573 ) ) ;
#25687 = CARTESIAN_POINT ( 'NONE',  ( 24.90994014085372399, 3.541349694169430684, -0.3428566583711011306 ) ) ;
#25688 = EDGE_LOOP ( 'NONE', ( #10902, #35207, #13672, #40469, #28919 ) ) ;
#25689 = CARTESIAN_POINT ( 'NONE',  ( 1.720943750993247701, -26.16997840318206059, 7.779495906702013741 ) ) ;
#25690 = AXIS2_PLACEMENT_3D ( 'NONE', #12768, #28421, #6810 ) ;
#25691 = LINE ( 'NONE', #39029, #2228 ) ;
#25692 = CARTESIAN_POINT ( 'NONE',  ( 4.484829609511931103, -25.15321385373581720, 6.954324564059724878 ) ) ;
#25693 = CARTESIAN_POINT ( 'NONE',  ( 68.66337269546751543, 58.46565884629779930, 3.990501929453249108 ) ) ;
#25694 = CARTESIAN_POINT ( 'NONE',  ( 31.71897322010782005, -0.5584286422544006978, 5.156910915900758674 ) ) ;
#25695 = ADVANCED_FACE ( 'NONE', ( #4405 ), #22536, .F. ) ;
#25696 = CARTESIAN_POINT ( 'NONE',  ( 72.29787722903529357, 59.46803282872462404, -3.909340765805334961 ) ) ;
#25697 = CARTESIAN_POINT ( 'NONE',  ( 4.285375923250596131, -31.77851530935270929, 7.782167645815903256 ) ) ;
#25698 = CARTESIAN_POINT ( 'NONE',  ( 86.00040182524281818, 1.757991441285688961, 4.533237565279400805 ) ) ;
#25699 = EDGE_LOOP ( 'NONE', ( #1458, #4356, #38604, #5764 ) ) ;
#25701 = CARTESIAN_POINT ( 'NONE',  ( -0.4019653665099892637, -26.77169832722271181, 6.980586498568963627 ) ) ;
#25700 = CARTESIAN_POINT ( 'NONE',  ( 81.25428736789774575, 61.63226232517330061, -2.112861953993772968 ) ) ;
#25702 = CARTESIAN_POINT ( 'NONE',  ( -1.363502849816506712, -31.24056455800023002, 7.780491323090173772 ) ) ;
#25703 = DIRECTION ( 'NONE',  ( 0.2567910337120216657, 0.7055275666422177183, -0.6605219282605403475 ) ) ;
#25704 = CARTESIAN_POINT ( 'NONE',  ( 3.991766160750894077, -32.22459883366656896, 7.255881584735161205 ) ) ;
#25705 = ORIENTED_EDGE ( 'NONE', *, *, #21905, .T. ) ;
#25706 = AXIS2_PLACEMENT_3D ( 'NONE', #30774, #18802, #22721 ) ;
#25707 = FACE_OUTER_BOUND ( 'NONE', #23450, .T. ) ;
#25708 = ORIENTED_EDGE ( 'NONE', *, *, #351, .T. ) ;
#25709 = CARTESIAN_POINT ( 'NONE',  ( -76.98048151946119333, -6.014858136247810627, 7.963062423954818669 ) ) ;
#25710 = ORIENTED_EDGE ( 'NONE', *, *, #35567, .T. ) ;
#25711 = CARTESIAN_POINT ( 'NONE',  ( 80.23783879855322709, 63.84144632218769999, -3.668443954219269276 ) ) ;
#25712 = ADVANCED_FACE ( 'NONE', ( #16929 ), #23128, .F. ) ;
#25713 = CARTESIAN_POINT ( 'NONE',  ( -71.92837670882107659, -0.7829914368874774100, 5.916079783099621459 ) ) ;
#25714 = EDGE_CURVE ( 'NONE', #19304, #30375, #9367, .T. ) ;
#25715 = CARTESIAN_POINT ( 'NONE',  ( 22.53613453900640451, 1.693789802652694521, 5.566700593757581750 ) ) ;
#25716 = ORIENTED_EDGE ( 'NONE', *, *, #15845, .T. ) ;
#25717 = EDGE_CURVE ( 'NONE', #2507, #30413, #12486, .T. ) ;
#25718 = AXIS2_PLACEMENT_3D ( 'NONE', #39909, #23842, #24049 ) ;
#25719 = DIRECTION ( 'NONE',  ( 0.000000000000000000, 0.000000000000000000, 1.000000000000000000 ) ) ;
#25720 = B_SPLINE_CURVE_WITH_KNOTS ( 'NONE', 3,
 ( #13016, #3778, #29476, #32375, #677, #4173, #10116, #1088, #25578, #38123 ),
 .UNSPECIFIED., .F., .F.,
 ( 4, 3, 3, 4 ),
 ( 0.0002170292169044743470, 0.0002420761345915946555, 0.0002723302478206985223, 0.0002816811360866763132 ),
 .UNSPECIFIED. ) ;
#25722 = CARTESIAN_POINT ( 'NONE',  ( 85.33631068939730824, 2.503930124734163432, 2.279864513413099925 ) ) ;
#25721 = CARTESIAN_POINT ( 'NONE',  ( -58.94134291052900920, 28.40740006353605906, -6.287813344559351592 ) ) ;
#25723 = CARTESIAN_POINT ( 'NONE',  ( -24.97867591359219475, -26.64985754041175525, 6.700000000000000178 ) ) ;
#25724 = CARTESIAN_POINT ( 'NONE',  ( -64.08758708074093136, 43.61223003902852469, -1.151575380241328439 ) ) ;
#25725 = CARTESIAN_POINT ( 'NONE',  ( 71.26393988290669768, 58.68354208002635630, 3.837797619696095897 ) ) ;
#25726 = CARTESIAN_POINT ( 'NONE',  ( 22.41273418899857361, 3.677808312967091098, -4.075635063406390479 ) ) ;
#25727 = ORIENTED_EDGE ( 'NONE', *, *, #20853, .F. ) ;
#25728 = VERTEX_POINT ( 'NONE', #30518 ) ;
#25729 = CARTESIAN_POINT ( 'NONE',  ( 21.85643539959777826, -11.73360331217645225, -7.400322805736739618 ) ) ;
#25730 = CARTESIAN_POINT ( 'NONE',  ( 21.20506779834672884, 9.695729361094967302, 1.510497956681738305E-12 ) ) ;
#25731 = ORIENTED_EDGE ( 'NONE', *, *, #22573, .T. ) ;
#25732 = DIRECTION ( 'NONE',  ( -0.000000000000000000, -0.000000000000000000, -1.000000000000000000 ) ) ;
#25733 = CARTESIAN_POINT ( 'NONE',  ( 81.64001200210110198, 62.74592715519806774, 2.852119850618822117 ) ) ;
#25734 = CARTESIAN_POINT ( 'NONE',  ( 85.96608680028057847, 1.729603650198207054, 5.123763289084741324 ) ) ;
#25735 = EDGE_CURVE ( 'NONE', #18355, #18960, #23717, .T. ) ;
#25736 = ORIENTED_EDGE ( 'NONE', *, *, #11131, .T. ) ;
#25737 = DIRECTION ( 'NONE',  ( 1.000000000000000000, 0.000000000000000000, 0.000000000000000000 ) ) ;
#25738 = EDGE_LOOP ( 'NONE', ( #20692, #1535, #11230, #18212 ) ) ;
#25739 = CARTESIAN_POINT ( 'NONE',  ( 14.74798687898900162, -4.496105769315120959, 2.508178052513492684 ) ) ;
#25740 = CARTESIAN_POINT ( 'NONE',  ( 36.39182469969075839, -2.321310407235841033, 5.886222402629798900 ) ) ;
#25741 = CYLINDRICAL_SURFACE ( 'NONE', #7216, 0.09010775117052950700 ) ;
#25742 = CARTESIAN_POINT ( 'NONE',  ( 21.25554376393856160, 3.326128914239820489, -3.523839690267918545 ) ) ;
#25743 = LINE ( 'NONE', #38284, #35219 ) ;
#25744 = CARTESIAN_POINT ( 'NONE',  ( 11.65737507970504439, -32.06993018339339585, 6.000000000000000000 ) ) ;
#25745 = PRODUCT_DEFINITION_SHAPE ( 'NONE', 'NONE',  #38149 ) ;
#25746 = CARTESIAN_POINT ( 'NONE',  ( -73.02027574113616026, 0.7163629790712561229, 10.94380017644704495 ) ) ;
#25747 = CARTESIAN_POINT ( 'NONE',  ( 2.913833110970087681, -32.85284901314008010, 7.750000000000001776 ) ) ;
#25748 = EDGE_CURVE ( 'NONE', #37415, #35810, #3275, .T. ) ;
#25749 = CARTESIAN_POINT ( 'NONE',  ( -1.302126302899671906, -31.16520435485670859, 7.757178535559533294 ) ) ;
#25750 = VECTOR ( 'NONE', #18116, 1000.000000000000114 ) ;
#25751 = CYLINDRICAL_SURFACE ( 'NONE', #14048, 95.38357402481355507 ) ;
#25752 = EDGE_LOOP ( 'NONE', ( #17017, #8100, #6322, #20576 ) ) ;
#25753 = ORIENTED_EDGE ( 'NONE', *, *, #28742, .T. ) ;
#25754 = CARTESIAN_POINT ( 'NONE',  ( 35.72916689304948790, -1.306553130388697470, 5.539900376742572519 ) ) ;
#25755 = CARTESIAN_POINT ( 'NONE',  ( 11.29080664838498826, -10.90558813203967148, 6.000000000000000000 ) ) ;
#25756 = CARTESIAN_POINT ( 'NONE',  ( 66.68517307240369973, 57.97439930951417608, -3.998354769216140525 ) ) ;
#25757 = EDGE_CURVE ( 'NONE', #29308, #1802, #18561, .T. ) ;
#25758 = CARTESIAN_POINT ( 'NONE',  ( -79.95330471031414277, 33.71485196875532608, 8.800414904976364028 ) ) ;
#25759 = ORIENTED_EDGE ( 'NONE', *, *, #33305, .F. ) ;
#25760 = EDGE_CURVE ( 'NONE', #17865, #12529, #6095, .T. ) ;
#25761 = FACE_OUTER_BOUND ( 'NONE', #27056, .T. ) ;
#25762 = CARTESIAN_POINT ( 'NONE',  ( -64.85784325972055342, 34.81586596186931359, 6.466735817496056526 ) ) ;
#25763 = CARTESIAN_POINT ( 'NONE',  ( -70.92837670882107659, -23.80776546975053520, 0.000000000000000000 ) ) ;
#25764 = ORIENTED_EDGE ( 'NONE', *, *, #14723, .T. ) ;
#25765 = FACE_BOUND ( 'NONE', #3772, .T. ) ;
#25766 = CARTESIAN_POINT ( 'NONE',  ( 3.801569219118249965, -32.36904792630235050, 6.931070083220557621 ) ) ;
#25767 = VERTEX_POINT ( 'NONE', #36891 ) ;
#25768 = EDGE_CURVE ( 'NONE', #14030, #18413, #694, .T. ) ;
#25769 = CARTESIAN_POINT ( 'NONE',  ( 81.44533364721141311, 61.45470812716253306, -1.173033592341551579 ) ) ;
#25770 = CARTESIAN_POINT ( 'NONE',  ( 2.851183333853939850, -26.37060056268141039, 7.756377446753168314 ) ) ;
#25771 = ORIENTED_EDGE ( 'NONE', *, *, #24940, .F. ) ;
#25772 = CARTESIAN_POINT ( 'NONE',  ( 74.72764284544139457, 63.14151651683601330, -3.204585025132376419 ) ) ;
#25774 = PLANE ( 'NONE',  #39337 ) ;
#25773 = CARTESIAN_POINT ( 'NONE',  ( 3.551251297819357777, -26.64985754041175525, 6.700000000000000178 ) ) ;
#25775 = CARTESIAN_POINT ( 'NONE',  ( 14.77413646174418993, 12.29989388524484717, -2.512259327332496461 ) ) ;
#25776 = CARTESIAN_POINT ( 'NONE',  ( 76.03108743707696249, 63.27561679962268215, 3.498861892150627373 ) ) ;
#25777 = VERTEX_POINT ( 'NONE', #36096 ) ;
#25778 = CARTESIAN_POINT ( 'NONE',  ( 4.357793904757863324, -27.44903297171773460, 6.870716933885666400 ) ) ;
#25779 = CARTESIAN_POINT ( 'NONE',  ( 1.794853143836061315, -26.07837181994090159, 7.776484688137384360 ) ) ;
#25780 = AXIS2_PLACEMENT_3D ( 'NONE', #31096, #31703, #12545 ) ;
#25781 = LINE ( 'NONE', #7840, #28232 ) ;
#25782 = CARTESIAN_POINT ( 'NONE',  ( 81.43190433112084747, 61.44807093728565661, 1.203271478923120696 ) ) ;
#25783 = B_SPLINE_CURVE_WITH_KNOTS ( 'NONE', 3,
 ( #35349, #13900, #19684, #4246, #4056, #16572, #22981, #29352, #32654, #23371, #35741, #13287, #1172, #28951, #35149, #4453, #19483, #20076, #38602 ),
 .UNSPECIFIED., .F., .F.,
 ( 4, 3, 3, 3, 3, 3, 4 ),
 ( 4.336808689942017736E-19, 2.546128104244715982E-05, 5.711050680484228820E-05, 8.113074941675809228E-05, 0.0001053129305727074576, 0.0001360598016347136941, 0.0001612931755713733735 ),
 .UNSPECIFIED. ) ;
#25785 = CARTESIAN_POINT ( 'NONE',  ( 13.68084590952481427, 8.951769248947412549, 3.481680054008543745 ) ) ;
#25784 = CARTESIAN_POINT ( 'NONE',  ( -64.08758708074093136, 43.61223004741322740, 1.151969611512877467 ) ) ;
#25786 = CARTESIAN_POINT ( 'NONE',  ( 27.46505532721044318, 0.1961140298417080874, 5.884446595982424810 ) ) ;
#25787 = CARTESIAN_POINT ( 'NONE',  ( 2.378989766893257141, -26.23833859934407187, 7.778050822775631978 ) ) ;
#25788 = CARTESIAN_POINT ( 'NONE',  ( -80.92837670882107659, 2.429809908903242555, 12.50000000000000000 ) ) ;
#25789 = VECTOR ( 'NONE', #35487, 1000.000000000000000 ) ;
#25790 = CARTESIAN_POINT ( 'NONE',  ( 27.60344192425479193, 81.15229837709949834, -4.000000000000000000 ) ) ;
#25791 = LINE ( 'NONE', #7046, #25077 ) ;
#25792 = DIRECTION ( 'NONE',  ( -1.000000000000000000, 0.000000000000000000, 0.000000000000000000 ) ) ;
#25793 = CARTESIAN_POINT ( 'NONE',  ( 37.05407933310225133, -3.059547152614165544, -5.984220936588256379 ) ) ;
#25794 = DIRECTION ( 'NONE',  ( 0.000000000000000000, 0.000000000000000000, 1.000000000000000000 ) ) ;
#25795 = CARTESIAN_POINT ( 'NONE',  ( 3.262282976461500894, -25.12033811116058502, 7.695279973900954751 ) ) ;
#25796 = CARTESIAN_POINT ( 'NONE',  ( 3.416617830832153757, -32.50498765347735031, 7.748216051605118615 ) ) ;
#25797 = CARTESIAN_POINT ( 'NONE',  ( -80.23765913646487036, 10.48825455491124536, 6.049483936935463824 ) ) ;
#25798 = LINE ( 'NONE', #4186, #30716 ) ;
#25799 = CARTESIAN_POINT ( 'NONE',  ( -1.477019764706915872, -28.35990217932980073, 7.785868773668302545 ) ) ;
#25800 = VERTEX_POINT ( 'NONE', #1922 ) ;
#25801 = FACE_OUTER_BOUND ( 'NONE', #28615, .T. ) ;
#25802 = CARTESIAN_POINT ( 'NONE',  ( 67.76947924466990969, 58.18518750870053680, -3.996132678073307964 ) ) ;
#25803 = VERTEX_POINT ( 'NONE', #11345 ) ;
#25804 = CARTESIAN_POINT ( 'NONE',  ( 28.52663967383706023, 50.14399159706753295, -1.000000000000000000 ) ) ;
#25805 = CYLINDRICAL_SURFACE ( 'NONE', #30504, 0.9999999999999977796 ) ;
#25806 = CARTESIAN_POINT ( 'NONE',  ( 24.12107463544779407, 2.969626750525581560, 3.756100707807366046 ) ) ;
#25807 = CARTESIAN_POINT ( 'NONE',  ( 5.045002655040953243, -28.53863642728069649, 7.006908160621412307 ) ) ;
#25808 =( REPRESENTATION_RELATIONSHIP ('NONE','NONE', #24012, #28236 ) REPRESENTATION_RELATIONSHIP_WITH_TRANSFORMATION ( #21514 )SHAPE_REPRESENTATION_RELATIONSHIP( ) );
#25809 = CARTESIAN_POINT ( 'NONE',  ( 1.159600155072761707, -26.21319852615044610, 7.785868773668302545 ) ) ;
#25810 =( GEOMETRIC_REPRESENTATION_CONTEXT ( 3 ) GLOBAL_UNCERTAINTY_ASSIGNED_CONTEXT ( ( #8979 ) ) GLOBAL_UNIT_ASSIGNED_CONTEXT ( ( #27662, #12000, #37131 ) ) REPRESENTATION_CONTEXT ( 'NONE', 'WORKASPACE' ) );
#25812 = EDGE_CURVE ( 'NONE', #14380, #39731, #36486, .T. ) ;
#25811 = CARTESIAN_POINT ( 'NONE',  ( -36.24874870218063450, -26.64985754041175525, 6.700000000000000178 ) ) ;
#25813 = ORIENTED_EDGE ( 'NONE', *, *, #21613, .T. ) ;
#25814 = EDGE_CURVE ( 'NONE', #27970, #22388, #29899, .T. ) ;
#25815 = ADVANCED_FACE ( 'NONE', ( #1714 ), #36686, .F. ) ;
#25816 = DIRECTION ( 'NONE',  ( 1.000000000000000000, -0.000000000000000000, 0.000000000000000000 ) ) ;
#25817 = CARTESIAN_POINT ( 'NONE',  ( 79.96011558216464721, 64.80970700093439518, 3.432259906339278022 ) ) ;
#25818 = EDGE_CURVE ( 'NONE', #19388, #13396, #11148, .T. ) ;
#25819 = DIRECTION ( 'NONE',  ( 1.000000000000000000, 0.000000000000000000, 0.000000000000000000 ) ) ;
#25820 = ORIENTED_EDGE ( 'NONE', *, *, #3448, .F. ) ;
#25821 = CARTESIAN_POINT ( 'NONE',  ( 80.07249602437107683, 61.49066053983646896, -2.889371261047466000 ) ) ;
#25823 = CARTESIAN_POINT ( 'NONE',  ( -1.710676486807355845, -28.78592482586367396, 6.908075350836297979 ) ) ;
#25822 = CARTESIAN_POINT ( 'NONE',  ( 22.30986545779548536, 0.2685651372915308088, 7.076871089830634176 ) ) ;
#25824 = CARTESIAN_POINT ( 'NONE',  ( 80.02729359676482090, 65.84138187185882884, -2.563845612518027117 ) ) ;
#25825 = CARTESIAN_POINT ( 'NONE',  ( 78.07544678589873399, 65.62285883043881540, 1.832491541757240494 ) ) ;
#25826 = DIRECTION ( 'NONE',  ( 0.000000000000000000, -1.000000000000000000, 0.000000000000000000 ) ) ;
#25827 = CARTESIAN_POINT ( 'NONE',  ( 80.36293583174433763, 66.30725055998102846, 1.299258709308648729 ) ) ;
#25829 = ORIENTED_EDGE ( 'NONE', *, *, #1351, .T. ) ;
#25828 = CARTESIAN_POINT ( 'NONE',  ( -63.68258360981171506, 44.25809753515871137, 1.883067893878278998 ) ) ;
#25830 = CARTESIAN_POINT ( 'NONE',  ( 24.19350110911862828, 1.223952504169800948, -6.554579921768042716 ) ) ;
#25831 = LINE ( 'NONE', #28302, #17355 ) ;
#25832 = ORIENTED_EDGE ( 'NONE', *, *, #23301, .T. ) ;
#25833 = VECTOR ( 'NONE', #10009, 1000.000000000000000 ) ;
#25834 = CARTESIAN_POINT ( 'NONE',  ( -77.85578999393689514, -5.090959542573109786, 7.225404102923549843 ) ) ;
#25835 = CARTESIAN_POINT ( 'NONE',  ( 24.74194048200748597, 0.5346423267196033224, -4.782325428828064773 ) ) ;
#25836 = CARTESIAN_POINT ( 'NONE',  ( -0.1177018426203055718, -32.54868846376324143, 7.780491323090173772 ) ) ;
#25837 = ORIENTED_EDGE ( 'NONE', *, *, #12119, .T. ) ;
#25838 = CARTESIAN_POINT ( 'NONE',  ( 24.15143939495542469, 3.654138348660112445, 2.050033071069497392 ) ) ;
#25839 = CARTESIAN_POINT ( 'NONE',  ( 25.73330770164922043, 2.636588466549696808, -3.521397845908182944 ) ) ;
#25840 =( NAMED_UNIT ( * ) PLANE_ANGLE_UNIT ( ) SI_UNIT ( $, .RADIAN. ) );
#25841 = CARTESIAN_POINT ( 'NONE',  ( 3.358563326585730646, -32.65222908060306395, 6.863784140767622333 ) ) ;
#25842 = CARTESIAN_POINT ( 'NONE',  ( 19.21638140921048432, 7.328436742462230313, 3.172542048904986256 ) ) ;
#25843 = CARTESIAN_POINT ( 'NONE',  ( 5.196273801610021614, -29.73962725910407201, 6.895394898881660239 ) ) ;
#25844 = DIRECTION ( 'NONE',  ( 1.000000000000000000, -0.000000000000000000, 0.000000000000000000 ) ) ;
#25845 = DIRECTION ( 'NONE',  ( 0.000000000000000000, -1.000000000000000000, 0.000000000000000000 ) ) ;
#25846 = VECTOR ( 'NONE', #37541, 1000.000000000000000 ) ;
#25847 = FACE_OUTER_BOUND ( 'NONE', #1609, .T. ) ;
#25848 = CARTESIAN_POINT ( 'NONE',  ( 22.45284782988909811, 0.4695142227150546077, -6.716274792382588288 ) ) ;
#25849 = CARTESIAN_POINT ( 'NONE',  ( 35.79905751890628096, -1.348410822439406020, -5.558858606210413278 ) ) ;
#25850 = CARTESIAN_POINT ( 'NONE',  ( 14.77222812468949620, -65.19654454972992141, 2.511961485181804843 ) ) ;
#25851 = ORIENTED_EDGE ( 'NONE', *, *, #29231, .F. ) ;
#25852 =( BOUNDED_CURVE ( )  B_SPLINE_CURVE ( 3, ( #517, #16142, #9961, #22741 ),
 .UNSPECIFIED., .F., .F. ) 
 B_SPLINE_CURVE_WITH_KNOTS ( ( 4, 4 ),
 ( 4.708531083176465515, 4.895802057644187855 ),
 .UNSPECIFIED. ) 
 CURVE ( )  GEOMETRIC_REPRESENTATION_ITEM ( )  RATIONAL_B_SPLINE_CURVE ( ( 1.000000000000000000, 0.9970795998553221295, 0.9970795998553221295, 1.000000000000000000 ) ) 
 REPRESENTATION_ITEM ( '' )  );
#25853 = ORIENTED_EDGE ( 'NONE', *, *, #15939, .F. ) ;
#25854 = CARTESIAN_POINT ( 'NONE',  ( 66.56005047484954673, 57.86167872611329699, 3.999845987730311858 ) ) ;
#25855 = CARTESIAN_POINT ( 'NONE',  ( 87.21044761576042958, -0.9232309944945271685, 5.337239039084527015 ) ) ;
#25856 = ORIENTED_EDGE ( 'NONE', *, *, #20772, .T. ) ;
#25857 = CARTESIAN_POINT ( 'NONE',  ( -73.02118209071689137, 4.148434801556117435, -10.94370216587312328 ) ) ;
#25858 = CARTESIAN_POINT ( 'NONE',  ( 0.000000000000000000, 0.000000000000000000, 0.000000000000000000 ) ) ;
#25859 = CARTESIAN_POINT ( 'NONE',  ( 2.231244765351310999, -32.92823233136791572, 7.785172627573962778 ) ) ;
#25860 = CARTESIAN_POINT ( 'NONE',  ( -14.87867591359218977, -26.64985754041175525, 6.700000000000000178 ) ) ;
#25861 = VERTEX_POINT ( 'NONE', #17726 ) ;
#25862 = FILL_AREA_STYLE_COLOUR ( '', #37887 ) ;
#25863 = ADVANCED_FACE ( 'NONE', ( #8466 ), #30310, .F. ) ;
#25864 = ORIENTED_EDGE ( 'NONE', *, *, #25397, .F. ) ;
#25865 = CARTESIAN_POINT ( 'NONE',  ( 80.24949846641645479, 62.81397012663808255, -3.564905221331803098 ) ) ;
#25866 = CARTESIAN_POINT ( 'NONE',  ( -1.722970638209900596, -28.84261588273779964, 7.754798119455333705 ) ) ;
#25867 = CARTESIAN_POINT ( 'NONE',  ( 80.78018476400359305, 61.88220158024267903, 2.864416008774245626 ) ) ;
#25871 = VERTEX_POINT ( 'NONE', #18548 ) ;
#25870 = VERTEX_POINT ( 'NONE', #24952 ) ;
#25869 = CARTESIAN_POINT ( 'NONE',  ( 2.721684545581986470, -26.21510794498386332, 7.139344958878412584 ) ) ;
#25868 = AXIS2_PLACEMENT_3D ( 'NONE', #32718, #17427, #7583 ) ;
#25872 = DIRECTION ( 'NONE',  ( -0.000000000000000000, -0.000000000000000000, -1.000000000000000000 ) ) ;
#25873 = CARTESIAN_POINT ( 'NONE',  ( 0.9057233922578412644, -32.97852313274928804, 6.935328752148349096 ) ) ;
#25874 = DIRECTION ( 'NONE',  ( -0.9848077530122069101, -0.1736481776669374644, -0.000000000000000000 ) ) ;
#25875 = CARTESIAN_POINT ( 'NONE',  ( -80.78329181448161478, 33.71485196875532608, -8.800414904976364028 ) ) ;
#25876 = CARTESIAN_POINT ( 'NONE',  ( 23.14179022917130624, 4.013511596053603192, -3.137277550560443995 ) ) ;
#25877 = ORIENTED_EDGE ( 'NONE', *, *, #27060, .T. ) ;
#25878 = CARTESIAN_POINT ( 'NONE',  ( 5.200336455197794194, -29.55055330619316223, 7.643192810543819604 ) ) ;
#25879 = CARTESIAN_POINT ( 'NONE',  ( -1.032376314427851050, -31.59280015088546278, 6.979335674598005745 ) ) ;
#25880 = CARTESIAN_POINT ( 'NONE',  ( -72.95330471031414277, 33.71485196875532608, -8.800414904976364028 ) ) ;
#25881 = AXIS2_PLACEMENT_3D ( 'NONE', #29729, #10980, #23561 ) ;
#25882 = CARTESIAN_POINT ( 'NONE',  ( -73.70917786874233002, -1.221531673705063215, -10.83923324353724382 ) ) ;
#25883 = DIRECTION ( 'NONE',  ( -0.7055275666422188285, 0.2567910337120248299, 0.6605219282605380160 ) ) ;
#25884 = CARTESIAN_POINT ( 'NONE',  ( -70.92837670882238399, -21.78299143689875095, 10.00000000000113154 ) ) ;
#25885 = CARTESIAN_POINT ( 'NONE',  ( 81.36058090587516745, 62.33601367849698249, 2.816708194897752815 ) ) ;
#25886 = CARTESIAN_POINT ( 'NONE',  ( 84.54687988124997844, 2.467165036067117789, -3.672804150685311964 ) ) ;
#25887 = LINE ( 'NONE', #19303, #8840 ) ;
#25888 = CARTESIAN_POINT ( 'NONE',  ( -1.267760583032661037, -27.71561997405539302, 7.754798119455333705 ) ) ;
#25889 = FACE_OUTER_BOUND ( 'NONE', #18959, .T. ) ;
#25890 = EDGE_CURVE ( 'NONE', #13304, #2129, #21459, .T. ) ;
#25891 = VERTEX_POINT ( 'NONE', #37488 ) ;
#25892 = AXIS2_PLACEMENT_3D ( 'NONE', #23571, #11391, #33472 ) ;
#25893 = FACE_OUTER_BOUND ( 'NONE', #3522, .T. ) ;
#25894 = CARTESIAN_POINT ( 'NONE',  ( 18.54755872719595544, 7.518511093671114587, -3.101193132418598175 ) ) ;
#25895 = CARTESIAN_POINT ( 'NONE',  ( 3.913023411691590514, -33.78267210696904499, 6.894806418505347700 ) ) ;
#25896 = CARTESIAN_POINT ( 'NONE',  ( -0.9894248136993964993, -27.33053388830764874, 7.635761828346571356 ) ) ;
#25897 = ORIENTED_EDGE ( 'NONE', *, *, #21424, .T. ) ;
#25898 = CARTESIAN_POINT ( 'NONE',  ( 68.59886892412534110, 58.63590986220410173, 3.993768376023888234 ) ) ;
#25899 = CARTESIAN_POINT ( 'NONE',  ( 31.71961843867553199, -0.5565345743523945066, 5.157011617862919728 ) ) ;
#25900 = EDGE_CURVE ( 'NONE', #29061, #34783, #35696, .T. ) ;
#25901 = DIRECTION ( 'NONE',  ( -0.000000000000000000, -1.000000000000000000, -0.000000000000000000 ) ) ;
#25902 = CARTESIAN_POINT ( 'NONE',  ( 88.28392341775159480, -0.8069683938931414557, -2.555979571574120257 ) ) ;
#25903 = ORIENTED_EDGE ( 'NONE', *, *, #24975, .T. ) ;
#25905 = CARTESIAN_POINT ( 'NONE',  ( -4.348748702180639469, -25.49307895267003587, 6.700000000000000178 ) ) ;
#25904 = CARTESIAN_POINT ( 'NONE',  ( 80.70080623961231936, 63.70112813535636320, -3.588566286536281069 ) ) ;
#25906 = CARTESIAN_POINT ( 'NONE',  ( 4.358291535071522560, -27.29274773012506827, 7.686927408461905920 ) ) ;
#25907 = ORIENTED_EDGE ( 'NONE', *, *, #38331, .T. ) ;
#25908 = DIRECTION ( 'NONE',  ( 1.000000000000000000, 1.241493069327139093E-16, 0.000000000000000000 ) ) ;
#25909 = EDGE_LOOP ( 'NONE', ( #12110, #34136, #34041, #38291 ) ) ;
#25910 = DIRECTION ( 'NONE',  ( 0.000000000000000000, 0.000000000000000000, -1.000000000000000000 ) ) ;
#25911 = AXIS2_PLACEMENT_3D ( 'NONE', #24584, #8515, #24377 ) ;
#25912 = AXIS2_PLACEMENT_3D ( 'NONE', #28812, #13159, #6783 ) ;
#25913 = AXIS2_PLACEMENT_3D ( 'NONE', #15131, #40243, #12028 ) ;
#25914 = ORIENTED_EDGE ( 'NONE', *, *, #20688, .T. ) ;
#25915 = EDGE_CURVE ( 'NONE', #21520, #24796, #18761, .T. ) ;
#25916 = CARTESIAN_POINT ( 'NONE',  ( 80.57397677244573231, 62.93365480201026685, -3.508091314521179171 ) ) ;
#25917 = FACE_OUTER_BOUND ( 'NONE', #36593, .T. ) ;
#25918 = CARTESIAN_POINT ( 'NONE',  ( 24.13837906798738686, 1.684127973681580848, 4.584305409718924196 ) ) ;
#25920 = VERTEX_POINT ( 'NONE', #15061 ) ;
#25919 = ORIENTED_EDGE ( 'NONE', *, *, #32226, .F. ) ;
#25921 = CARTESIAN_POINT ( 'NONE',  ( 79.97870788650297413, 66.10023056730543090, -2.166533184762310604 ) ) ;
#25922 = AXIS2_PLACEMENT_3D ( 'NONE', #23123, #16523, #29099 ) ;
#25923 = CARTESIAN_POINT ( 'NONE',  ( 5.671973749040267521, -26.25500220387225170, 7.635761828346577573 ) ) ;
#25924 = CIRCLE ( 'NONE', #31190, 0.1000000000000028644 ) ;
#25926 = CARTESIAN_POINT ( 'NONE',  ( 85.63625186893746388, 2.167021955807470590, 3.489522741179289067 ) ) ;
#25925 = CARTESIAN_POINT ( 'NONE',  ( 4.607344540115766662, -31.33336738918632847, 6.874555630061443878 ) ) ;
#25927 = DIRECTION ( 'NONE',  ( 1.000000000000000000, 0.000000000000000000, 0.000000000000000000 ) ) ;
#25928 = CARTESIAN_POINT ( 'NONE',  ( 70.86714415968630476, 59.66805877367134769, 3.971832046809244510 ) ) ;
#25929 = CARTESIAN_POINT ( 'NONE',  ( 22.77263692411995066, 3.805474047185834596, -3.697090138710067198 ) ) ;
#25930 = ORIENTED_EDGE ( 'NONE', *, *, #25668, .T. ) ;
#25931 = CARTESIAN_POINT ( 'NONE',  ( 5.149333021513059272, -30.16559723925941228, 7.756742906098589074 ) ) ;
#25932 = VERTEX_POINT ( 'NONE', #15880 ) ;
#25933 = EDGE_CURVE ( 'NONE', #5343, #25658, #12172, .T. ) ;
#25934 = CARTESIAN_POINT ( 'NONE',  ( 21.85643539959774273, 10.54442680926682208, -0.8960936389291185300 ) ) ;
#25935 = CARTESIAN_POINT ( 'NONE',  ( 21.77466435201619888, 5.668278662187346661, -2.100676170762209249 ) ) ;
#25936 = CARTESIAN_POINT ( 'NONE',  ( 0.4870777624547221185, -32.74607263478868191, 6.889465824494258150 ) ) ;
#25937 = CARTESIAN_POINT ( 'NONE',  ( 81.55127126995144238, 61.75833066296597451, 1.907437723464473711 ) ) ;
#25938 = CARTESIAN_POINT ( 'NONE',  ( 88.61980888719223515, -1.376070350315937940, 2.940712392697649058 ) ) ;
#25939 = ORIENTED_EDGE ( 'NONE', *, *, #24444, .T. ) ;
#25940 = CARTESIAN_POINT ( 'NONE',  ( 0.4238093638620683556, -32.72117464255529029, 7.754798119455333705 ) ) ;
#25941 = ORIENTED_EDGE ( 'NONE', *, *, #1875, .T. ) ;
#25942 = FACE_OUTER_BOUND ( 'NONE', #11282, .T. ) ;
#25943 = AXIS2_PLACEMENT_3D ( 'NONE', #1504, #13847, #26613 ) ;
#25944 = VECTOR ( 'NONE', #529, 1000.000000000000000 ) ;
#25945 = CARTESIAN_POINT ( 'NONE',  ( 32.39520944364767274, -3.784153674530718714, 4.877599362950213013 ) ) ;
#25946 = CARTESIAN_POINT ( 'NONE',  ( 36.78920673448757128, -3.041418453456746551, -5.948243479880678919 ) ) ;
#25947 = CARTESIAN_POINT ( 'NONE',  ( 0.5502190760550982329, -32.76947806258566231, 7.635761828346577573 ) ) ;
#25948 = DIRECTION ( 'NONE',  ( -0.6427876096865545730, 0.7660444431189653569, 0.000000000000000000 ) ) ;
#25949 = ADVANCED_FACE ( 'NONE', ( #3160 ), #18977, .T. ) ;
#25950 = EDGE_CURVE ( 'NONE', #25461, #40182, #8716, .T. ) ;
#25951 = DIRECTION ( 'NONE',  ( -0.000000000000000000, -0.000000000000000000, 1.000000000000000000 ) ) ;
#25952 = ORIENTED_EDGE ( 'NONE', *, *, #29421, .T. ) ;
#25953 = ADVANCED_FACE ( 'NONE', ( #24743 ), #12384, .T. ) ;
#25954 = VECTOR ( 'NONE', #3342, 1000.000000000000000 ) ;
#25955 = DIRECTION ( 'NONE',  ( 0.000000000000000000, 0.000000000000000000, 1.000000000000000000 ) ) ;
#25956 = CARTESIAN_POINT ( 'NONE',  ( 33.44054677433027933, -3.435571797939218186, 5.408185224205094954 ) ) ;
#25957 = VERTEX_POINT ( 'NONE', #5807 ) ;
#25958 = ORIENTED_EDGE ( 'NONE', *, *, #25537, .T. ) ;
#25959 = CARTESIAN_POINT ( 'NONE',  ( 34.79243474202561970, -3.834671068451598330, 5.377539100044668174 ) ) ;
#25960 = CARTESIAN_POINT ( 'NONE',  ( -80.92837670882107659, 2.429809908903242555, 15.50000000000000000 ) ) ;
#25961 = DIRECTION ( 'NONE',  ( 0.000000000000000000, 0.000000000000000000, -1.000000000000000000 ) ) ;
#25962 = CARTESIAN_POINT ( 'NONE',  ( 87.79841724921489288, -2.358232370636156094, -2.005059250078357724 ) ) ;
#25963 = ORIENTED_EDGE ( 'NONE', *, *, #9843, .T. ) ;
#25964 = DIRECTION ( 'NONE',  ( 0.000000000000000000, 0.000000000000000000, -1.000000000000000000 ) ) ;
#25965 = EDGE_CURVE ( 'NONE', #18869, #12672, #22075, .T. ) ;
#25966 = ORIENTED_EDGE ( 'NONE', *, *, #17697, .F. ) ;
#25967 = FACE_BOUND ( 'NONE', #30506, .T. ) ;
#25968 = CARTESIAN_POINT ( 'NONE',  ( 3.816332953347056467, -32.35790253036758202, 7.011627023500185629 ) ) ;
#25969 = VERTEX_POINT ( 'NONE', #31541 ) ;
#25970 = CARTESIAN_POINT ( 'NONE',  ( 22.91573592208010623, 4.163909958596558880, 3.247526573974286013 ) ) ;
#25971 = CARTESIAN_POINT ( 'NONE',  ( 81.96987370863051581, 65.13652322159772723, -1.905332024691357429 ) ) ;
#25972 = COLOUR_RGB ( '',0.7921568627450980005, 0.8196078431372548767, 0.9333333333333333481 ) ;
#25973 = VECTOR ( 'NONE', #39479, 1000.000000000000000 ) ;
#25974 = LINE ( 'NONE', #29656, #10782 ) ;
#25975 = ORIENTED_EDGE ( 'NONE', *, *, #38478, .F. ) ;
#25976 = CARTESIAN_POINT ( 'NONE',  ( 75.42787669100914627, 61.66269772210893763, -3.901127667181031100 ) ) ;
#25978 = DIRECTION ( 'NONE',  ( -0.000000000000000000, -0.000000000000000000, -1.000000000000000000 ) ) ;
#25977 = PLANE ( 'NONE',  #39032 ) ;
#25979 = PLANE ( 'NONE',  #15212 ) ;
#25980 = CARTESIAN_POINT ( 'NONE',  ( 77.82713238777958509, 60.98268764611925974, 3.435658781984941346 ) ) ;
#25981 = ORIENTED_EDGE ( 'NONE', *, *, #27979, .F. ) ;
#25982 = LINE ( 'NONE', #16298, #33337 ) ;
#25983 = VECTOR ( 'NONE', #13993, 1000.000000000000114 ) ;
#25984 = CARTESIAN_POINT ( 'NONE',  ( 1.700951572572590331, -26.07317559334259371, 7.767720160662275219 ) ) ;
#25985 = CARTESIAN_POINT ( 'NONE',  ( 25.94849358905778658, 1.816623773615693160, -4.256288009898165470 ) ) ;
#25986 = CARTESIAN_POINT ( 'NONE',  ( 80.91683595914895477, 65.70075836866587338, 2.460680857248573883 ) ) ;
#25987 = CARTESIAN_POINT ( 'NONE',  ( -64.08758708074093136, 43.61223004741322740, 1.000000000000000000 ) ) ;
#25988 = CARTESIAN_POINT ( 'NONE',  ( 29.14988983353436680, -2.161137664473038900, -5.740130334263455758 ) ) ;
#25989 = CARTESIAN_POINT ( 'NONE',  ( -1.699450209411329737, -29.60309949032410515, 7.670860738520326905 ) ) ;
#25990 = CARTESIAN_POINT ( 'NONE',  ( 30.13156937888698650, -4.637989059070824815, 0.4506576151153146581 ) ) ;
#25991 = ADVANCED_FACE ( 'NONE', ( #24533 ), #21250, .F. ) ;
#25992 = PLANE ( 'NONE',  #4444 ) ;
#25993 = CARTESIAN_POINT ( 'NONE',  ( -0.5341021525900384592, -32.13256682235309114, 6.880147297696980857 ) ) ;
#25994 = CARTESIAN_POINT ( 'NONE',  ( 3.922483456672744673, -26.86580350659783178, 7.695279973900954751 ) ) ;
#25995 = EDGE_CURVE ( 'NONE', #26563, #22837, #3198, .T. ) ;
#25996 = CARTESIAN_POINT ( 'NONE',  ( 36.88189763748390959, -2.428839298856057205, -5.959479764620102316 ) ) ;
#25997 = DIRECTION ( 'NONE',  ( 0.000000000000000000, 0.000000000000000000, 1.000000000000000000 ) ) ;
#25998 = LINE ( 'NONE', #26802, #37104 ) ;
#25999 = CARTESIAN_POINT ( 'NONE',  ( -42.44874870218064444, -26.64985754041175525, 6.800000000000000711 ) ) ;
#26000 = CARTESIAN_POINT ( 'NONE',  ( 2.198740986243329587, -32.93322359727931570, 6.866852738645442322 ) ) ;
#26001 = EDGE_CURVE ( 'NONE', #4425, #25619, #30936, .T. ) ;
#26002 = CARTESIAN_POINT ( 'NONE',  ( 21.86476427169857217, -13.72881702355425659, -2.499999999999999556 ) ) ;
#26003 = VECTOR ( 'NONE', #27752, 1000.000000000000000 ) ;
#26004 = CARTESIAN_POINT ( 'NONE',  ( -1.500935203769204973, -28.42471564332976541, 7.748216051605119503 ) ) ;
#26005 = AXIS2_PLACEMENT_3D ( 'NONE', #27156, #39709, #24060 ) ;
#26006 = CYLINDRICAL_SURFACE ( 'NONE', #21423, 12.73502530973474123 ) ;
#26007 = EDGE_LOOP ( 'NONE', ( #25515, #23866, #38449, #33537 ) ) ;
#26008 = CARTESIAN_POINT ( 'NONE',  ( 36.73497401824715780, -2.304546233985284687, 5.935212642074513489 ) ) ;
#26009 = CARTESIAN_POINT ( 'NONE',  ( -1.347521135996686992, -31.09247807141954212, 7.386948897581450346 ) ) ;
#26010 = EDGE_CURVE ( 'NONE', #7366, #23047, #14007, .T. ) ;
#26011 = CARTESIAN_POINT ( 'NONE',  ( 67.77942698303134250, 58.15829091545840157, -3.995247128881093790 ) ) ;
#26012 = DIRECTION ( 'NONE',  ( 0.000000000000000000, 0.000000000000000000, 1.000000000000000000 ) ) ;
#26013 = ORIENTED_EDGE ( 'NONE', *, *, #10457, .F. ) ;
#26014 = PLANE ( 'NONE',  #9494 ) ;
#26015 = CARTESIAN_POINT ( 'NONE',  ( 30.71442180045753290, -3.288768831658976932, 4.965733434219046671 ) ) ;
#26016 = CARTESIAN_POINT ( 'NONE',  ( 23.47630927499801246, 3.090003628763607679, 3.883072686897193648 ) ) ;
#26017 = CARTESIAN_POINT ( 'NONE',  ( 2.323431556773316586, -32.91235948273799750, 7.670860738520328681 ) ) ;
#26018 = DIRECTION ( 'NONE',  ( 1.000000000000000000, 3.965082230804130614E-15, 0.000000000000000000 ) ) ;
#26019 = CARTESIAN_POINT ( 'NONE',  ( 1.245175783478524867, -26.09964713766223099, 6.880828092187098122 ) ) ;
#26020 = ORIENTED_EDGE ( 'NONE', *, *, #29916, .F. ) ;
#26021 = CARTESIAN_POINT ( 'NONE',  ( 22.38222497467343430, 4.936969384760538482, 3.050972054430843183 ) ) ;
#26022 = CARTESIAN_POINT ( 'NONE',  ( 78.75316082766835279, 66.06368344870412557, 1.496866203714574572 ) ) ;
#26023 = CARTESIAN_POINT ( 'NONE',  ( 0.4724743091557946362, -26.29239483759356588, 7.720710062488890024 ) ) ;
#26024 = ORIENTED_EDGE ( 'NONE', *, *, #31351, .T. ) ;
#26025 = CARTESIAN_POINT ( 'NONE',  ( 78.19628368166274868, 65.45398019160434444, -2.372109611208335078 ) ) ;
#26027 = CARTESIAN_POINT ( 'NONE',  ( -1.740368116565756518, -28.92869283221914145, 6.891642963669610822 ) ) ;
#26026 = CARTESIAN_POINT ( 'NONE',  ( 26.75149414979017237, 0.8971556662521585901, 4.382797809037470849 ) ) ;
#26028 = CARTESIAN_POINT ( 'NONE',  ( 78.84958593098521362, 66.12877247161736705, -1.370814772365197554 ) ) ;
#26029 = CARTESIAN_POINT ( 'NONE',  ( 80.40236172895532718, 61.11465044667751556, 2.108843360059433625 ) ) ;
#26030 = EDGE_CURVE ( 'NONE', #27970, #37105, #40368, .T. ) ;
#26031 = AXIS2_PLACEMENT_3D ( 'NONE', #35776, #13533, #34986 ) ;
#26032 = FACE_OUTER_BOUND ( 'NONE', #32907, .T. ) ;
#26033 = VECTOR ( 'NONE', #24587, 1000.000000000000000 ) ;
#26034 = CARTESIAN_POINT ( 'NONE',  ( 82.54681503119226704, 63.20390409618732974, 1.263752851812355305 ) ) ;
#26035 = CARTESIAN_POINT ( 'NONE',  ( -64.08758708074091714, 41.79071634614418684, 3.815532762722622095 ) ) ;
#26036 = CARTESIAN_POINT ( 'NONE',  ( 22.82080504511013430, -6.970192185297126031, -1.116939615399285657 ) ) ;
#26037 = CARTESIAN_POINT ( 'NONE',  ( -63.39880662924674226, 35.63549842397627998, -6.795986594146541826 ) ) ;
#26038 = ORIENTED_EDGE ( 'NONE', *, *, #2297, .F. ) ;
#26039 = CARTESIAN_POINT ( 'NONE',  ( -80.77097820227440650, -5.650553507305215994, 4.970441783940528602 ) ) ;
#26040 = CARTESIAN_POINT ( 'NONE',  ( 26.76517688821456886, 0.8539537780654303800, -4.383552559536760818 ) ) ;
#26041 = EDGE_CURVE ( 'NONE', #32186, #12012, #24213, .T. ) ;
#26042 = CIRCLE ( 'NONE', #25395, 1.000000000000005107 ) ;
#26043 = DIRECTION ( 'NONE',  ( -0.000000000000000000, -0.000000000000000000, -1.000000000000000000 ) ) ;
#26044 = CARTESIAN_POINT ( 'NONE',  ( 1.736346942945568905, -25.86893018339335981, 7.695279973900954751 ) ) ;
#26045 = EDGE_CURVE ( 'NONE', #35202, #5880, #37480, .T. ) ;
#26046 = EDGE_LOOP ( 'NONE', ( #36040, #25365, #22880, #39377 ) ) ;
#26047 = CARTESIAN_POINT ( 'NONE',  ( 36.49309394506007465, -3.558324574553789699, -5.797191926096202153 ) ) ;
#26048 = CYLINDRICAL_SURFACE ( 'NONE', #37763, 0.09010775117052929883 ) ;
#26049 = PLANE ( 'NONE',  #31477 ) ;
#26050 = CARTESIAN_POINT ( 'NONE',  ( -1.089794412209061480, -31.68295418363346272, 7.006908160621417636 ) ) ;
#26051 = CARTESIAN_POINT ( 'NONE',  ( 5.195250593675200257, -29.75957179320715085, 6.931070083220548739 ) ) ;
#26052 = LINE ( 'NONE', #32241, #25335 ) ;
#26053 = CARTESIAN_POINT ( 'NONE',  ( -28.44874870218064444, -26.64985754041175525, 6.700000000000000178 ) ) ;
#26054 = EDGE_CURVE ( 'NONE', #422, #36032, #26375, .T. ) ;
#26055 = CARTESIAN_POINT ( 'NONE',  ( -26.97867591359219475, -24.55319635012989110, 6.700000000000000178 ) ) ;
#26056 = CARTESIAN_POINT ( 'NONE',  ( 22.80317954561651561, 0.6168027127662122355, -6.115043150466682675 ) ) ;
#26057 = CARTESIAN_POINT ( 'NONE',  ( 32.98075398114073664, -0.1054326221632065214, -4.920934273367439715 ) ) ;
#26058 = EDGE_CURVE ( 'NONE', #37348, #109, #31952, .T. ) ;
#26059 = CARTESIAN_POINT ( 'NONE',  ( 19.45444762198869881, 11.13896630807285781, -2.499999999999990230 ) ) ;
#26060 = ORIENTED_EDGE ( 'NONE', *, *, #907, .T. ) ;
#26061 = CARTESIAN_POINT ( 'NONE',  ( 66.70872257673579497, 57.90880667275003901, 3.999713739233790921 ) ) ;
#26062 = DIRECTION ( 'NONE',  ( -0.000000000000000000, -0.000000000000000000, -1.000000000000000000 ) ) ;
#26063 = CARTESIAN_POINT ( 'NONE',  ( 84.10435792013542766, 3.012680099502687892, -0.4953216543819284889 ) ) ;
#26064 = VECTOR ( 'NONE', #2798, 1000.000000000000000 ) ;
#26065 = ORIENTED_EDGE ( 'NONE', *, *, #37090, .T. ) ;
#26066 = CARTESIAN_POINT ( 'NONE',  ( -8.295002936191391285, 28.24537450226321411, 2.500000000000000000 ) ) ;
#26067 = APPLICATION_PROTOCOL_DEFINITION ( 'draft international standard', 'automotive_design', 1998, #4008 ) ;
#26068 = VECTOR ( 'NONE', #16206, 1000.000000000000000 ) ;
#26069 = CARTESIAN_POINT ( 'NONE',  ( 2.322457828100205290, -32.91253870567615536, 7.721096864323903297 ) ) ;
#26070 = CARTESIAN_POINT ( 'NONE',  ( -61.24591834330252027, 10.37661300689600097, -2.500000000000000000 ) ) ;
#26071 = ORIENTED_EDGE ( 'NONE', *, *, #28738, .T. ) ;
#26072 = PLANE ( 'NONE',  #37985 ) ;
#26073 = ORIENTED_EDGE ( 'NONE', *, *, #297, .F. ) ;
#26074 = VECTOR ( 'NONE', #19798, 1000.000000000000000 ) ;
#26075 = CARTESIAN_POINT ( 'NONE',  ( 80.83921286824487140, 61.18398161863571971, -1.552792442904344261 ) ) ;
#26076 = CARTESIAN_POINT ( 'NONE',  ( 5.166866161692755810, -29.08666662507720702, 7.750000000000000888 ) ) ;
#26077 = CARTESIAN_POINT ( 'NONE',  ( 78.63837616148850884, 65.82632162494860495, 2.064111563736254595 ) ) ;
#26078 = CARTESIAN_POINT ( 'NONE',  ( -1.666958026621576883, -30.04000107135736641, 7.754798119455333705 ) ) ;
#26079 = CARTESIAN_POINT ( 'NONE',  ( 24.20923528093676680, 2.663529708714821087, 3.984834686794740399 ) ) ;
#26080 = DIRECTION ( 'NONE',  ( 0.000000000000000000, 0.000000000000000000, 1.000000000000000000 ) ) ;
#26081 = CYLINDRICAL_SURFACE ( 'NONE', #14987, 0.09010775117053118621 ) ;
#26082 = CARTESIAN_POINT ( 'NONE',  ( 21.85643539959776049, -3.688311691778667800, 15.92486026856874304 ) ) ;
#26083 = CYLINDRICAL_SURFACE ( 'NONE', #23096, 0.09010775117052960415 ) ;
#26084 = CARTESIAN_POINT ( 'NONE',  ( 24.06794754132348046, 3.349686124075685445, -3.202891862519920529 ) ) ;
#26085 = ORIENTED_EDGE ( 'NONE', *, *, #31768, .F. ) ;
#26086 = DIRECTION ( 'NONE',  ( 1.000000000000000000, 0.000000000000000000, -0.000000000000000000 ) ) ;
#26087 = EDGE_LOOP ( 'NONE', ( #14842, #9675, #29855, #12274, #5547 ) ) ;
#26088 = CARTESIAN_POINT ( 'NONE',  ( -1.020414035563122601, -31.60885757119451256, 7.013842709614101167 ) ) ;
#26089 = LINE ( 'NONE', #38824, #28078 ) ;
#26090 = MANIFOLD_SOLID_BREP ( 'Fillet14', #26858 ) ;
#26091 = CARTESIAN_POINT ( 'NONE',  ( -72.95563224246589584, 3.799282472582091508, -9.852485720729166729 ) ) ;
#26092 = DIRECTION ( 'NONE',  ( -0.000000000000000000, -0.000000000000000000, -1.000000000000000000 ) ) ;
#26093 = CYLINDRICAL_SURFACE ( 'NONE', #16872, 3.000000000000002665 ) ;
#26094 = CARTESIAN_POINT ( 'NONE',  ( 81.20101650719863073, 62.86240828450105766, 3.233552917234625124 ) ) ;
#26095 = CARTESIAN_POINT ( 'NONE',  ( 86.27652758060003180, -0.2533697966053802819, -5.917929974479952726 ) ) ;
#26096 =( BOUNDED_SURFACE ( )  B_SPLINE_SURFACE ( 3, 2, ( 
 ( #28147, #19091, #38218 ),
 ( #19293, #6742, #31860 ),
 ( #25675, #12704, #12908 ),
 ( #40701, #10015, #12503 ) ),
 .UNSPECIFIED., .F., .F., .F. ) 
 B_SPLINE_SURFACE_WITH_KNOTS ( ( 4, 4 ),
 ( 3, 3 ),
 ( 1.734723475976807094E-18, 0.0006385966863608955914 ),
 ( 0.000000000000000000, 1.000000000000000000 ),
 .UNSPECIFIED. ) 
 GEOMETRIC_REPRESENTATION_ITEM ( )  RATIONAL_B_SPLINE_SURFACE ( (
 ( 1.000000000000000000, 0.5652620711642704077, 1.000000000000000000),
 ( 1.000000000000000000, 0.5746205253747180830, 1.000000000000000000),
 ( 1.000000000000000000, 0.5840949208454062624, 1.000000000000000000),
 ( 1.000000000000000000, 0.5935057080259644735, 1.000000000000000000) ) ) 
 REPRESENTATION_ITEM ( '' )  SURFACE ( )  );
#26097 = CARTESIAN_POINT ( 'NONE',  ( -0.03448549664302677509, -32.60970101154014600, 7.750000000000000000 ) ) ;
#26098 = CARTESIAN_POINT ( 'NONE',  ( -0.8809027425463855643, -31.78283038357269419, 7.695279973900954751 ) ) ;
#26099 = CARTESIAN_POINT ( 'NONE',  ( 3.922523015185340522, -26.86583601202378802, 7.698786668945015066 ) ) ;
#26100 = AXIS2_PLACEMENT_3D ( 'NONE', #7676, #11151, #13658 ) ;
#26101 = VECTOR ( 'NONE', #28307, 1000.000000000000000 ) ;
#26102 = AXIS2_PLACEMENT_3D ( 'NONE', #986, #28777, #16997 ) ;
#26103 = ORIENTED_EDGE ( 'NONE', *, *, #16813, .T. ) ;
#26104 = EDGE_CURVE ( 'NONE', #33055, #27373, #8094, .T. ) ;
#26105 = CARTESIAN_POINT ( 'NONE',  ( 1.062037487867982355, -25.86893018339336692, 6.894806418505347700 ) ) ;
#26106 = CARTESIAN_POINT ( 'NONE',  ( -0.3962189974208576992, -26.89332219547525327, 6.864276522220859711 ) ) ;
#26107 = EDGE_CURVE ( 'NONE', #14959, #25549, #19382, .T. ) ;
#26108 = DIRECTION ( 'NONE',  ( 0.000000000000000000, 0.000000000000000000, 1.000000000000000000 ) ) ;
#26109 = ORIENTED_EDGE ( 'NONE', *, *, #21958, .F. ) ;
#26110 = CARTESIAN_POINT ( 'NONE',  ( 35.78611850173684417, -3.163414878908757277, 5.791687301379355723 ) ) ;
#26111 = CARTESIAN_POINT ( 'NONE',  ( 4.227867036651674404, -31.84410382479391188, 7.759451378593101190 ) ) ;
#26112 = CARTESIAN_POINT ( 'NONE',  ( 87.14484084030976874, 0.3304612005822565313, -5.669005978848654870 ) ) ;
#26114 = CARTESIAN_POINT ( 'NONE',  ( 4.819878230686599707, -30.92226195030272606, 6.920489980334474822 ) ) ;
#26113 = CARTESIAN_POINT ( 'NONE',  ( 79.42059605865689775, 65.48104909687435793, -2.923497156821688314 ) ) ;
#26115 = CARTESIAN_POINT ( 'NONE',  ( -1.233832883691663662, -27.66196159070634408, 6.989977667959444751 ) ) ;
#26116 = CARTESIAN_POINT ( 'NONE',  ( -57.65239026484333351, 32.60637517809080066, 4.103028154974615482 ) ) ;
#26117 = ORIENTED_EDGE ( 'NONE', *, *, #37421, .T. ) ;
#26118 = PLANE ( 'NONE',  #18790 ) ;
#26119 = EDGE_LOOP ( 'NONE', ( #15679, #34648, #19371 ) ) ;
#26120 = LINE ( 'NONE', #406, #33398 ) ;
#26121 = VECTOR ( 'NONE', #7594, 1000.000000000000000 ) ;
#26122 = ORIENTED_EDGE ( 'NONE', *, *, #964, .T. ) ;
#26123 = CARTESIAN_POINT ( 'NONE',  ( 80.15465141033460839, 63.79803065853134569, -3.683925914261567680 ) ) ;
#26124 = CARTESIAN_POINT ( 'NONE',  ( -88.78960668556791802, 4.298224710795182091, 15.50000000000000000 ) ) ;
#26125 = AXIS2_PLACEMENT_3D ( 'NONE', #12611, #7245, #37924 ) ;
#26126 = B_SPLINE_CURVE_WITH_KNOTS ( 'NONE', 3,
 ( #21533, #34315, #126, #5883, #2813, #3028, #40047, #3236, #6085, #34111 ),
 .UNSPECIFIED., .F., .F.,
 ( 4, 3, 3, 4 ),
 ( 0.0002170292169044765425, 0.0002420761345915954958, 0.0002723302478207011244, 0.0002816811360866737111 ),
 .UNSPECIFIED. ) ;
#26127 = CARTESIAN_POINT ( 'NONE',  ( 23.86924164457367681, 1.381515540322357793, 4.867119774624979023 ) ) ;
#26128 = ORIENTED_EDGE ( 'NONE', *, *, #34109, .T. ) ;
#26129 = VECTOR ( 'NONE', #38196, 1000.000000000000000 ) ;
#26130 = FACE_OUTER_BOUND ( 'NONE', #7419, .T. ) ;
#26132 = CARTESIAN_POINT ( 'NONE',  ( 86.45266110354762645, 1.249992354373530290, 4.889332228698039629 ) ) ;
#26131 = CARTESIAN_POINT ( 'NONE',  ( 4.602267184982021142, -31.34168336721522508, 6.870716933885666400 ) ) ;
#26133 = CARTESIAN_POINT ( 'NONE',  ( -1.253435461249161831, -27.88620972153293565, 7.748216051605118615 ) ) ;
#26134 = CARTESIAN_POINT ( 'NONE',  ( 70.90076320674430121, 59.58500768881799559, 3.976054184260641833 ) ) ;
#26135 = CARTESIAN_POINT ( 'NONE',  ( 23.66861057507165356, 3.139937292340087893, -3.766843508339346780 ) ) ;
#26136 = VERTEX_POINT ( 'NONE', #16282 ) ;
#26137 = CARTESIAN_POINT ( 'NONE',  ( 5.121205169401321200, -30.24961392475126232, 7.782861076432731728 ) ) ;
#26138 = EDGE_LOOP ( 'NONE', ( #28368, #9035, #35698, #39323 ) ) ;
#26139 = EDGE_CURVE ( 'NONE', #27725, #29312, #17285, .T. ) ;
#26140 = CARTESIAN_POINT ( 'NONE',  ( 21.85643539959774273, 10.58808081918846256, 0.01331417752983106093 ) ) ;
#26141 = CARTESIAN_POINT ( 'NONE',  ( 21.38787910473958220, 9.379444465846978218, 3.308503362033488049 ) ) ;
#26142 = CARTESIAN_POINT ( 'NONE',  ( -12.24874870218063627, -25.49307895267003587, 6.700000000000000178 ) ) ;
#26143 = CARTESIAN_POINT ( 'NONE',  ( 79.04416262434369855, 66.14279969385417246, 1.662073781718003351 ) ) ;
#26144 = CARTESIAN_POINT ( 'NONE',  ( 87.00363285854439255, 0.09201467311058098009, -5.867932143725643535 ) ) ;
#26145 = FACE_OUTER_BOUND ( 'NONE', #16823, .T. ) ;
#26146 = VERTEX_POINT ( 'NONE', #35252 ) ;
#26147 = CARTESIAN_POINT ( 'NONE',  ( -80.83812573300635052, -5.651420041020555729, 4.817690839865847785 ) ) ;
#26148 = CARTESIAN_POINT ( 'NONE',  ( 19.69258716046599744, -2.691695111070238955, 3.279902512047694341 ) ) ;
#26149 = VECTOR ( 'NONE', #20538, 1000.000000000000000 ) ;
#26150 = DIRECTION ( 'NONE',  ( 0.000000000000000000, -0.000000000000000000, -1.000000000000000000 ) ) ;
#26151 = CARTESIAN_POINT ( 'NONE',  ( 14.85065079210121652, -6.130908026932606170, -2.524201239090782867 ) ) ;
#26152 = ADVANCED_FACE ( 'NONE', ( #7021 ), #19589, .F. ) ;
#26153 = CARTESIAN_POINT ( 'NONE',  ( 36.97934183402728792, -2.956306430206838254, -5.977918660598608547 ) ) ;
#26154 = FACE_OUTER_BOUND ( 'NONE', #11699, .T. ) ;
#26155 = CARTESIAN_POINT ( 'NONE',  ( -1.765620486186735949, -30.05597079739024835, 7.753200566781599079 ) ) ;
#26156 = CARTESIAN_POINT ( 'NONE',  ( 29.83052353176027793, -3.763946442397907877, -4.488211747472833579 ) ) ;
#26157 = CARTESIAN_POINT ( 'NONE',  ( 2.902716051567627797, -32.85547488104512581, 7.762796336881261361 ) ) ;
#26158 = VECTOR ( 'NONE', #18350, 1000.000000000000000 ) ;
#26159 =( GEOMETRIC_REPRESENTATION_CONTEXT ( 3 ) GLOBAL_UNCERTAINTY_ASSIGNED_CONTEXT ( ( #37794 ) ) GLOBAL_UNIT_ASSIGNED_CONTEXT ( ( #6529, #10201, #35352 ) ) REPRESENTATION_CONTEXT ( 'NONE', 'WORKASPACE' ) );
#26160 = CARTESIAN_POINT ( 'NONE',  ( 3.422521930177921057, -32.50152978473241205, 7.652160403243384756 ) ) ;
#26161 = DIRECTION ( 'NONE',  ( -1.000000000000000000, 0.000000000000000000, 0.000000000000000000 ) ) ;
#26162 = VERTEX_POINT ( 'NONE', #32760 ) ;
#26163 = ORIENTED_EDGE ( 'NONE', *, *, #22966, .T. ) ;
#26164 = CARTESIAN_POINT ( 'NONE',  ( 37.17655189852746389, -2.564752334915549437, 5.980995930358914414 ) ) ;
#26165 = CARTESIAN_POINT ( 'NONE',  ( -1.635341556108417027, -30.62959728375151514, 6.875780273367530171 ) ) ;
#26166 = CARTESIAN_POINT ( 'NONE',  ( -62.81463675898083210, 36.67811266762162603, -4.600311178732273021 ) ) ;
#26167 = CARTESIAN_POINT ( 'NONE',  ( 87.91634809178921728, -2.499602875977831484, 0.5197879843876231920 ) ) ;
#26168 = ORIENTED_EDGE ( 'NONE', *, *, #39201, .F. ) ;
#26169 = DIRECTION ( 'NONE',  ( -0.000000000000000000, -1.000000000000000000, -0.000000000000000000 ) ) ;
#26170 = ORIENTED_EDGE ( 'NONE', *, *, #26282, .T. ) ;
#26171 = CARTESIAN_POINT ( 'NONE',  ( -57.02355111755383632, 29.45914411650375442, -1.982879248426652863 ) ) ;
#26172 = EDGE_CURVE ( 'NONE', #31547, #37682, #39513, .T. ) ;
#26173 = DIRECTION ( 'NONE',  ( -0.6427876096865430267, 0.7660444431189749048, -0.000000000000000000 ) ) ;
#26174 = ORIENTED_EDGE ( 'NONE', *, *, #8902, .T. ) ;
#26175 = CARTESIAN_POINT ( 'NONE',  ( 22.11225299742777750, 4.986280216054901793, 3.411143437232363240 ) ) ;
#26176 = CARTESIAN_POINT ( 'NONE',  ( 81.67240355425528264, 65.37253450681788536, -2.134985007310160832 ) ) ;
#26177 = VECTOR ( 'NONE', #6938, 1000.000000000000000 ) ;
#26178 = DIRECTION ( 'NONE',  ( -0.000000000000000000, -0.000000000000000000, 1.000000000000000000 ) ) ;
#26179 = ORIENTED_EDGE ( 'NONE', *, *, #36764, .F. ) ;
#26180 = CARTESIAN_POINT ( 'NONE',  ( 75.46848212330048966, 60.05767933327602748, -3.584990529380367441 ) ) ;
#26182 = CARTESIAN_POINT ( 'NONE',  ( -1.003736583562490070, -27.34783681995376270, 7.695279973900954751 ) ) ;
#26181 = CARTESIAN_POINT ( 'NONE',  ( -1.598573221982714454, -28.40080711106888600, 7.660770905198783787 ) ) ;
#26183 = DIRECTION ( 'NONE',  ( 1.000000000000000000, -0.000000000000000000, 0.000000000000000000 ) ) ;
#26184 = ADVANCED_FACE ( 'NONE', ( #36236 ), #11295, .F. ) ;
#26185 = CARTESIAN_POINT ( 'NONE',  ( 75.30130074865816425, 63.36357894040062178, 3.230144225280452641 ) ) ;
#26186 = CIRCLE ( 'NONE', #24856, 1.000000000000000222 ) ;
#26187 = ORIENTED_EDGE ( 'NONE', *, *, #854, .T. ) ;
#26188 = CARTESIAN_POINT ( 'NONE',  ( -64.08758708074093136, 36.87876644325631759, 4.900609702795903466 ) ) ;
#26189 = EDGE_CURVE ( 'NONE', #34939, #9457, #38907, .T. ) ;
#26190 = DIRECTION ( 'NONE',  ( 0.000000000000000000, 0.000000000000000000, 1.000000000000000000 ) ) ;
#26191 = CARTESIAN_POINT ( 'NONE',  ( 1.651482305834180986, -26.06346787019676370, 7.255881584735163869 ) ) ;
#26192 = DIRECTION ( 'NONE',  ( -0.000000000000000000, -1.000000000000000000, -0.000000000000000000 ) ) ;
#26193 = CARTESIAN_POINT ( 'NONE',  ( 80.13359286145602312, 66.18419574793108495, 1.944145319385262471 ) ) ;
#26194 = CARTESIAN_POINT ( 'NONE',  ( 86.50262394474026451, 1.193871719766480100, -4.934721793127618383 ) ) ;
#26195 = CARTESIAN_POINT ( 'NONE',  ( 28.10280119166142399, -0.8120181649793116740, 6.074162340139093175 ) ) ;
#26196 = LINE ( 'NONE', #10327, #13536 ) ;
#26197 = CARTESIAN_POINT ( 'NONE',  ( 3.570212250164635392, -26.73024761574886199, 6.911401339314953596 ) ) ;
#26198 = FACE_OUTER_BOUND ( 'NONE', #7131, .T. ) ;
#26199 = ORIENTED_EDGE ( 'NONE', *, *, #26873, .F. ) ;
#26200 = CARTESIAN_POINT ( 'NONE',  ( 0.6845764506890200662, -26.32520861239037302, 6.871394612369935651 ) ) ;
#26201 = CARTESIAN_POINT ( 'NONE',  ( 1.847632973160104664, 12.44248440543094958, -7.000000000000000000 ) ) ;
#26202 = DIRECTION ( 'NONE',  ( 0.5751513419797962268, -0.4826092789263561333, -0.6605219282605402364 ) ) ;
#26203 = EDGE_CURVE ( 'NONE', #19840, #1813, #33187, .T. ) ;
#26204 = CARTESIAN_POINT ( 'NONE',  ( 33.82080240299477225, -0.7236866431670748723, -5.383600818459516546 ) ) ;
#26205 = CARTESIAN_POINT ( 'NONE',  ( 3.751251297819363728, -26.64985754041175525, 6.700000000000000178 ) ) ;
#26206 = CARTESIAN_POINT ( 'NONE',  ( 4.976896699542257885, -28.33927813719497024, 7.700536657684219577 ) ) ;
#26207 = AXIS2_PLACEMENT_3D ( 'NONE', #4520, #36202, #34872 ) ;
#26208 = CARTESIAN_POINT ( 'NONE',  ( 3.293813124479239018, -32.57342865076346783, 7.754798119455333705 ) ) ;
#26209 = DIRECTION ( 'NONE',  ( 0.000000000000000000, 1.000000000000000000, 0.000000000000000000 ) ) ;
#26210 = DIRECTION ( 'NONE',  ( -0.000000000000000000, -0.000000000000000000, -1.000000000000000000 ) ) ;
#26211 = CARTESIAN_POINT ( 'NONE',  ( -16.34874870218063592, -26.64985754041175525, 6.700000000000000178 ) ) ;
#26212 = EDGE_LOOP ( 'NONE', ( #27234, #34641 ) ) ;
#26213 = CARTESIAN_POINT ( 'NONE',  ( 33.43765011243894492, -3.587404715383258669, 5.336366798597405037 ) ) ;
#26214 = PLANE ( 'NONE',  #2135 ) ;
#26215 = CARTESIAN_POINT ( 'NONE',  ( 67.49481586879284123, 58.02828806359071478, -3.995059460290581121 ) ) ;
#26216 = AXIS2_PLACEMENT_3D ( 'NONE', #34319, #15551, #30391 ) ;
#26217 = EDGE_CURVE ( 'NONE', #40515, #13771, #12923, .T. ) ;
#26218 = CARTESIAN_POINT ( 'NONE',  ( 11.65737507970504616, -30.94667987854474234, 6.000000000000000000 ) ) ;
#26219 = VERTEX_POINT ( 'NONE', #8016 ) ;
#26220 = CARTESIAN_POINT ( 'NONE',  ( 30.78887672857765168, -3.335710177092375162, 4.962067852009124813 ) ) ;
#26221 = CARTESIAN_POINT ( 'NONE',  ( 85.89661503870057402, 0.4533383911654620402, -5.989758072366164754 ) ) ;
#26222 = CARTESIAN_POINT ( 'NONE',  ( 0.4695943777967593880, -26.29347754267606874, 7.695279973900954751 ) ) ;
#26223 = CARTESIAN_POINT ( 'NONE',  ( 0.3259002109880320686, -32.78874652230489062, 6.935328752148349096 ) ) ;
#26224 = CARTESIAN_POINT ( 'NONE',  ( 8.290806648384990041, -25.50263309590217276, 6.000000000000001776 ) ) ;
#26225 = ORIENTED_EDGE ( 'NONE', *, *, #25291, .T. ) ;
#26226 = CARTESIAN_POINT ( 'NONE',  ( 21.98943303986548514, 5.609607562178218210, 3.094355746606469726 ) ) ;
#26227 = DIRECTION ( 'NONE',  ( 0.000000000000000000, 0.000000000000000000, 1.000000000000000000 ) ) ;
#26228 = CARTESIAN_POINT ( 'NONE',  ( 81.17453961776598703, 62.25628865055540473, 2.899379378185771738 ) ) ;
#26229 = MANIFOLD_SOLID_BREP ( 'Boss-Extrude7', #34124 ) ;
#26230 = CLOSED_SHELL ( 'NONE', ( #1424, #31482, #31765, #38756, #14429, #27437, #29059, #13669, #15106, #40476, #17167, #37879, #16305 ) ) ;
#26231 = CYLINDRICAL_SURFACE ( 'NONE', #16030, 7.341749246864647915 ) ;
#26232 = CARTESIAN_POINT ( 'NONE',  ( 79.07090634323701295, 63.55465448991838429, -3.774260586041105370 ) ) ;
#26234 = CARTESIAN_POINT ( 'NONE',  ( -1.738754558334627331, -28.92005600624478845, 6.883132039304661554 ) ) ;
#26233 = CARTESIAN_POINT ( 'NONE',  ( 23.59121300012005307, 0.4241677973105192345, 5.524108833373179372 ) ) ;
#26235 = ADVANCED_FACE ( 'NONE', ( #35808 ), #30219, .F. ) ;
#26236 = ADVANCED_FACE ( 'NONE', ( #23630 ), #4896, .T. ) ;
#26237 = CARTESIAN_POINT ( 'NONE',  ( 81.29034902432738363, 64.00233822786356086, -3.292658836668130196 ) ) ;
#26238 = CARTESIAN_POINT ( 'NONE',  ( 80.62600653171161014, 61.47375110407241294, 2.475680338657083812 ) ) ;
#26239 = ADVANCED_FACE ( 'NONE', ( #17639 ), #8169, .F. ) ;
#26240 = CARTESIAN_POINT ( 'NONE',  ( 82.51683713915190310, 64.24667231656799515, 1.319711737399753781 ) ) ;
#26242 = ORIENTED_EDGE ( 'NONE', *, *, #7348, .T. ) ;
#26241 = CARTESIAN_POINT ( 'NONE',  ( 11.29080664838498826, -10.90558813203967148, 6.000000000000000000 ) ) ;
#26243 = B_SPLINE_CURVE_WITH_KNOTS ( 'NONE', 3,
 ( #7998, #35634, #7406, #32541, #16862, #29443, #1256, #13792, #26360, #37580, #18234, #40674, #34535, #33138, #2833, #21750, #36978, #2629, #27708, #18437, #9376, #37385, #2426, #21962, #34333 ),
 .UNSPECIFIED., .F., .F.,
 ( 4, 3, 3, 3, 3, 3, 3, 3, 4 ),
 ( 6.468151674593709615E-05, 9.076621574722030540E-05, 0.0001210204262067986035, 0.0001512763324577439175, 0.0001815301820994234361, 0.0002117781465860742022, 0.0002420274594459773760, 0.0002722905548971168727, 0.0002816827545175609564 ),
 .UNSPECIFIED. ) ;
#26244 = CARTESIAN_POINT ( 'NONE',  ( 22.35506120569036170, 4.170988562608182626, 6.826273348963533216 ) ) ;
#26245 = CARTESIAN_POINT ( 'NONE',  ( -62.76544114002936681, 35.76323014769233311, -5.464922856233972226 ) ) ;
#26246 = ORIENTED_EDGE ( 'NONE', *, *, #30094, .F. ) ;
#26247 = CARTESIAN_POINT ( 'NONE',  ( -78.23674730379569553, -6.442058846907860570, 6.837204711868661633 ) ) ;
#26248 = LINE ( 'NONE', #12861, #8125 ) ;
#26249 = VECTOR ( 'NONE', #25443, 1000.000000000000000 ) ;
#26250 = CARTESIAN_POINT ( 'NONE',  ( 5.551251297819359110, -26.64985754041175525, 6.700000000000000178 ) ) ;
#26251 = CARTESIAN_POINT ( 'NONE',  ( -0.9934091780005464001, -31.78413689346535520, 7.783750581861599294 ) ) ;
#26252 = CARTESIAN_POINT ( 'NONE',  ( 35.22080398260825262, -1.047803307765222902, -5.411327744522335337 ) ) ;
#26253 = FILL_AREA_STYLE ('',( #20060 ) ) ;
#26254 = CARTESIAN_POINT ( 'NONE',  ( -4.444218661349752963, -35.94265729135299381, -2.500000000000000000 ) ) ;
#26255 = CARTESIAN_POINT ( 'NONE',  ( -1.059861091245062559, -31.72193407659015207, 6.867199677474204123 ) ) ;
#26256 = CARTESIAN_POINT ( 'NONE',  ( 5.200096824318753086, -29.61612186858987172, 6.880608371227953768 ) ) ;
#26257 = PRODUCT ( 'Measuring Ruler', 'Measuring Ruler', '', ( #17991 ) ) ;
#26258 = DIRECTION ( 'NONE',  ( -0.000000000000000000, -0.000000000000000000, -1.000000000000000000 ) ) ;
#26259 = CARTESIAN_POINT ( 'NONE',  ( 5.093940842300026084, -29.77924726035835334, 6.969307238440511476 ) ) ;
#26260 = CARTESIAN_POINT ( 'NONE',  ( 1.882503106173801566, -26.07466918923286414, 6.912143950357346078 ) ) ;
#26261 = CIRCLE ( 'NONE', #1963, 6.781342077912186461 ) ;
#26262 = LINE ( 'NONE', #7111, #39347 ) ;
#26263 = EDGE_LOOP ( 'NONE', ( #18085, #6160, #23222, #15441 ) ) ;
#26264 = CARTESIAN_POINT ( 'NONE',  ( 66.84168730393145097, 57.99964773888063974, 3.999029912551661070 ) ) ;
#26265 = CARTESIAN_POINT ( 'NONE',  ( 84.13636243568421946, 2.973867306686137191, 1.134085816324387430 ) ) ;
#26266 = DIRECTION ( 'NONE',  ( 0.4582725098355734938, -0.8888117386314180468, 0.000000000000000000 ) ) ;
#26267 = ORIENTED_EDGE ( 'NONE', *, *, #18126, .T. ) ;
#26268 = CARTESIAN_POINT ( 'NONE',  ( 2.870175459834257925, -26.27120282332167633, 7.730015791551948290 ) ) ;
#26269 = ADVANCED_FACE ( 'NONE', ( #27125 ), #20138, .F. ) ;
#26270 = CARTESIAN_POINT ( 'NONE',  ( 2.326171464738295835, -32.91184545387483951, 7.695279973900954751 ) ) ;
#26271 = FACE_OUTER_BOUND ( 'NONE', #29996, .T. ) ;
#26272 = CIRCLE ( 'NONE', #33509, 0.1000000000000028644 ) ;
#26273 = VERTEX_POINT ( 'NONE', #7783 ) ;
#26274 = DIRECTION ( 'NONE',  ( 0.000000000000000000, 1.000000000000000000, 0.000000000000000000 ) ) ;
#26275 = EDGE_LOOP ( 'NONE', ( #6883, #11494, #32544, #11816 ) ) ;
#26276 = EDGE_CURVE ( 'NONE', #9457, #26319, #19284, .T. ) ;
#26277 = ORIENTED_EDGE ( 'NONE', *, *, #37499, .F. ) ;
#26278 = CARTESIAN_POINT ( 'NONE',  ( 79.84106601136197412, 63.63461245521319398, -3.725738571856551662 ) ) ;
#26279 = CARTESIAN_POINT ( 'NONE',  ( 33.78683981622189947, -4.850133216411556702, 3.460854720750057290 ) ) ;
#26280 = CARTESIAN_POINT ( 'NONE',  ( 80.95177907874119683, 61.22464621339454283, 1.448968528257557287 ) ) ;
#26281 = CARTESIAN_POINT ( 'NONE',  ( -12.99139449055068241, -10.90558813203967148, 2.500000000000000000 ) ) ;
#26282 = EDGE_CURVE ( 'NONE', #14626, #1980, #21908, .T. ) ;
#26283 = CARTESIAN_POINT ( 'NONE',  ( 25.78209274739939971, 1.896337777400309399, 4.230317134137809632 ) ) ;
#26284 = CARTESIAN_POINT ( 'NONE',  ( 0.9089306018589854430, -32.97926988754144162, 6.984548363133216142 ) ) ;
#26285 = DIRECTION ( 'NONE',  ( 0.000000000000000000, 0.000000000000000000, -1.000000000000000000 ) ) ;
#26286 = CARTESIAN_POINT ( 'NONE',  ( 21.85643539959777470, -5.967561930184303698, -15.30482168765389694 ) ) ;
#26287 = CARTESIAN_POINT ( 'NONE',  ( 3.504784550580148483, -26.68823612567400971, 7.754798119455333705 ) ) ;
#26288 = EDGE_LOOP ( 'NONE', ( #3131, #28796, #24996, #14986 ) ) ;
#26289 = CARTESIAN_POINT ( 'NONE',  ( 67.37492487370475658, 58.42787741793769385, -4.000000000000127898 ) ) ;
#26290 = ORIENTED_EDGE ( 'NONE', *, *, #23514, .T. ) ;
#26291 = CARTESIAN_POINT ( 'NONE',  ( 14.66134950408317472, -4.888884664723367024, -2.500000000000003553 ) ) ;
#26292 = CARTESIAN_POINT ( 'NONE',  ( -63.08758708074093136, -21.25669541281728669, 3.000000000000000000 ) ) ;
#26293 = CARTESIAN_POINT ( 'NONE',  ( -74.81248793487165472, -2.854500793830079264, -10.54724492771533839 ) ) ;
#26294 = CARTESIAN_POINT ( 'NONE',  ( 5.140791489254627145, -28.92678305073006584, 7.695279973900954751 ) ) ;
#26295 = CARTESIAN_POINT ( 'NONE',  ( -70.92837670882107659, -65.19654454972992141, 0.000000000000000000 ) ) ;
#26296 = CARTESIAN_POINT ( 'NONE',  ( 81.33630325801044592, 62.05105258569627580, 2.628317182735721680 ) ) ;
#26297 = CARTESIAN_POINT ( 'NONE',  ( 1.300000000000000044, 0.5999999999999995337, -4.030609108440248889 ) ) ;
#26298 = CARTESIAN_POINT ( 'NONE',  ( 3.876017184916769942, -26.95713821644390862, 7.756377446753162097 ) ) ;
#26299 = CARTESIAN_POINT ( 'NONE',  ( -1.582528736513596490, -30.78337320113038444, 7.750000000000000000 ) ) ;
#26300 = CARTESIAN_POINT ( 'NONE',  ( -2.515717719208200531, -28.88150288888238393, 7.695279973900954751 ) ) ;
#26301 = VECTOR ( 'NONE', #37466, 1000.000000000000000 ) ;
#26302 = CARTESIAN_POINT ( 'NONE',  ( 4.472525015499347667, -27.43328141189353886, 6.875780273367532835 ) ) ;
#26303 = FACE_OUTER_BOUND ( 'NONE', #28954, .T. ) ;
#26304 = CARTESIAN_POINT ( 'NONE',  ( 4.978554560952730412, -30.79615924950642025, 6.894806418505347700 ) ) ;
#26305 = CARTESIAN_POINT ( 'NONE',  ( 1.700390093233090871, -29.56993018339339940, 7.750000000000000888 ) ) ;
#26306 = CARTESIAN_POINT ( 'NONE',  ( -10.34874870218063769, -26.64985754041175525, 6.800000000000000711 ) ) ;
#26307 = CARTESIAN_POINT ( 'NONE',  ( 68.51828301517210207, 58.84837915819282728, 3.980709302925309778 ) ) ;
#26308 = CARTESIAN_POINT ( 'NONE',  ( 25.29826323614737404, 1.741216666318694317, 4.154803837446060299 ) ) ;
#26309 = CARTESIAN_POINT ( 'NONE',  ( 4.240191228329224238, -31.83034962878108942, 7.774064877406530627 ) ) ;
#26310 = CARTESIAN_POINT ( 'NONE',  ( 85.25019696446999262, 2.600657147776545663, -2.704904232406868836 ) ) ;
#26312 = CARTESIAN_POINT ( 'NONE',  ( -0.4516137999636575251, -26.80967899891524553, 6.867199677474200570 ) ) ;
#26311 = CARTESIAN_POINT ( 'NONE',  ( 81.17805228937325523, 61.98952396227124950, -2.700485128497477572 ) ) ;
#26313 = CARTESIAN_POINT ( 'NONE',  ( -1.250607068061524885, -27.68798963190787532, 6.880828092187095457 ) ) ;
#26314 = CARTESIAN_POINT ( 'NONE',  ( 2.380073834590987758, -26.14911510722517463, 7.782861076432730840 ) ) ;
#26315 = EDGE_LOOP ( 'NONE', ( #22384, #11441, #17664, #5195 ) ) ;
#26316 = B_SPLINE_CURVE_WITH_KNOTS ( 'NONE', 3,
 ( #1934, #21261, #20630, #33217, #30122, #17735, #11355, #36497, #5614, #39988 ),
 .UNSPECIFIED., .F., .F.,
 ( 4, 3, 3, 4 ),
 ( 9.697399036122160616E-19, 3.025570593003156381E-05, 6.051145698344085212E-05, 6.468151674593620168E-05 ),
 .UNSPECIFIED. ) ;
#26317 = DIRECTION ( 'NONE',  ( -0.9848077530122092416, 0.1736481776669241694, -0.000000000000000000 ) ) ;
#26318 = CARTESIAN_POINT ( 'NONE',  ( -8.248748702180632719, -26.64985754041175525, 6.700000000000000178 ) ) ;
#26319 = VERTEX_POINT ( 'NONE', #33325 ) ;
#26320 = DIRECTION ( 'NONE',  ( 0.5000000000000101030, -0.8660254037844328234, -0.000000000000000000 ) ) ;
#26321 = ORIENTED_EDGE ( 'NONE', *, *, #7658, .F. ) ;
#26322 = CARTESIAN_POINT ( 'NONE',  ( 80.65169068708779321, 62.63775009584335152, -3.403428918328328834 ) ) ;
#26323 = LINE ( 'NONE', #29410, #19418 ) ;
#26324 = CARTESIAN_POINT ( 'NONE',  ( 81.01565502672983143, 61.93906859853276359, 2.769656700700043217 ) ) ;
#26325 = CARTESIAN_POINT ( 'NONE',  ( 24.59373887808777681, 0.8454200395481480390, 4.793554178231363316 ) ) ;
#26326 = ORIENTED_EDGE ( 'NONE', *, *, #22523, .T. ) ;
#26327 = EDGE_CURVE ( 'NONE', #23918, #22737, #35546, .T. ) ;
#26328 = EDGE_CURVE ( 'NONE', #27835, #35702, #39468, .T. ) ;
#26330 = EDGE_CURVE ( 'NONE', #36632, #7986, #36599, .T. ) ;
#26329 = CARTESIAN_POINT ( 'NONE',  ( -0.1040043641139408170, -32.45162424111279620, 7.754798119455333705 ) ) ;
#26331 =( BOUNDED_CURVE ( )  B_SPLINE_CURVE ( 3, ( #39197, #14290, #36332, #30572 ),
 .UNSPECIFIED., .F., .T. ) 
 B_SPLINE_CURVE_WITH_KNOTS ( ( 4, 4 ),
 ( 0.7028477130386120431, 1.570796326794896558 ),
 .UNSPECIFIED. ) 
 CURVE ( )  GEOMETRIC_REPRESENTATION_ITEM ( )  RATIONAL_B_SPLINE_CURVE ( ( 1.000000000000000000, 0.9382012019593851671, 0.9382012019593851671, 1.000000000000000000 ) ) 
 REPRESENTATION_ITEM ( '' )  );
#26333 = CARTESIAN_POINT ( 'NONE',  ( 8.290806648384990041, -25.50263309590217276, 2.499999999999998668 ) ) ;
#26332 = CARTESIAN_POINT ( 'NONE',  ( -58.47571659425080526, 29.43362125246419936, -5.129074445220336287 ) ) ;
#26334 = DIRECTION ( 'NONE',  ( 1.000000000000000000, 0.000000000000000000, 0.000000000000000000 ) ) ;
#26335 = B_SPLINE_SURFACE_WITH_KNOTS ( 'NONE', 3, 3, ( 
 ( #28801, #34591, #6159, #9027 ),
 ( #12525, #22016, #25099, #6021 ),
 ( #40582, #34447, #15685, #9500 ),
 ( #18987, #31965, #37498, #12797 ),
 ( #3374, #13006, #16293, #25775 ),
 ( #19187, #18772, #31346, #18558 ),
 ( #257, #28449, #25160, #31143 ),
 ( #15688, #22293, #28661, #28039 ),
 ( #3767, #13207, #15890, #35262 ),
 ( #22086, #38312, #24964, #25570 ),
 ( #25370, #28863, #37908, #31753 ),
 ( #9714, #21873, #22697, #10109 ),
 ( #34864, #19391, #28239, #35061 ),
 ( #2961, #3173, #9917, #6432 ),
 ( #6640, #64, #3565, #34660 ),
 ( #9295, #15477, #670, #40586 ),
 ( #12396, #34450, #6227, #12593 ),
 ( #37695, #9503, #18990, #16095 ),
 ( #31551, #467, #22498, #38114 ),
 ( #6835, #11109, #26781, #35855 ),
 ( #7833, #16680, #23488, #7428 ),
 ( #39116, #35658, #20383, #1278 ) ),
 .UNSPECIFIED., .F., .F., .F.,
 ( 4, 3, 3, 3, 3, 3, 3, 4 ),
 ( 4, 4 ),
 ( 0.004706533420950041041, 0.005436807504379657062, 0.006167081587809273083, 0.007627629754668505992, 0.009088177921527738901, 0.01054872608838697094, 0.01346982242210543676, 0.01639091875582390084 ),
 ( -0.006049311920859260297, 1.000000000000000000 ),
 .UNSPECIFIED. ) ;
#26336 = CARTESIAN_POINT ( 'NONE',  ( -64.08758708074093136, 43.97597776728673580, -1.778916918605509823 ) ) ;
#26337 = DIRECTION ( 'NONE',  ( 0.000000000000000000, 0.000000000000000000, 1.000000000000000000 ) ) ;
#26338 = EDGE_LOOP ( 'NONE', ( #19064, #11369, #6118, #8205 ) ) ;
#26339 = CARTESIAN_POINT ( 'NONE',  ( 23.16337524629349076, 3.871609807089642530, -3.315521066308895204 ) ) ;
#26340 = ORIENTED_EDGE ( 'NONE', *, *, #14908, .T. ) ;
#26341 = CARTESIAN_POINT ( 'NONE',  ( 5.125265918664630327, -30.21784728057895109, 7.785096263473211486 ) ) ;
#26342 = CARTESIAN_POINT ( 'NONE',  ( 23.96136931976388951, 3.582231692328178063, -3.646207630380492226 ) ) ;
#26343 = CIRCLE ( 'NONE', #30295, 0.1000000000000028644 ) ;
#26344 = CARTESIAN_POINT ( 'NONE',  ( 21.46948114135329533, 9.243557392227998548, 3.873122283670993315 ) ) ;
#26345 = CARTESIAN_POINT ( 'NONE',  ( 0.4111392921005667112, -32.71602809928322131, 6.865312560952602894 ) ) ;
#26346 = CARTESIAN_POINT ( 'NONE',  ( 81.65590348734941983, 63.08388229440976858, 2.971291902561975284 ) ) ;
#26347 = CARTESIAN_POINT ( 'NONE',  ( 88.14352194013933683, -1.303227188646099544, -4.271130342077624320 ) ) ;
#26348 = CARTESIAN_POINT ( 'NONE',  ( -1.406165058247869748, -30.96909808796597119, 7.505001789837627335 ) ) ;
#26349 = VERTEX_POINT ( 'NONE', #5105 ) ;
#26350 = ORIENTED_EDGE ( 'NONE', *, *, #12687, .F. ) ;
#26351 = PLANE ( 'NONE',  #9300 ) ;
#26352 = CARTESIAN_POINT ( 'NONE',  ( 32.25525712155970837, -3.777699995816486744, 4.851130129795467205 ) ) ;
#26353 = CARTESIAN_POINT ( 'NONE',  ( 28.89950236053841692, -2.887785649367553553, -4.716864299104555514 ) ) ;
#26354 = CARTESIAN_POINT ( 'NONE',  ( 31.71837165913483148, -0.5603379253444896735, -5.156817027762116368 ) ) ;
#26355 = FACE_OUTER_BOUND ( 'NONE', #374, .T. ) ;
#26356 = DIRECTION ( 'NONE',  ( -0.000000000000000000, -0.000000000000000000, 1.000000000000000000 ) ) ;
#26357 = CARTESIAN_POINT ( 'NONE',  ( 30.28289254991746304, -3.677685065117360264, -4.636463722753257244 ) ) ;
#26358 = ORIENTED_EDGE ( 'NONE', *, *, #10627, .T. ) ;
#26359 = CIRCLE ( 'NONE', #32304, 0.1000000000000028644 ) ;
#26360 = CARTESIAN_POINT ( 'NONE',  ( -1.647019466996949566, -30.16568013038308038, 7.763628509615286610 ) ) ;
#26361 = CARTESIAN_POINT ( 'NONE',  ( 5.013689988518933660, -28.46451312308398229, 7.776484688137385248 ) ) ;
#26362 = ORIENTED_EDGE ( 'NONE', *, *, #11834, .T. ) ;
#26363 = VERTEX_POINT ( 'NONE', #8377 ) ;
#26364 = CARTESIAN_POINT ( 'NONE',  ( 36.71923328895664440, -3.458898378518612038, 5.860548135656104662 ) ) ;
#26365 = CARTESIAN_POINT ( 'NONE',  ( -58.92473026143643722, -52.43948302755219260, 2.500000000000000000 ) ) ;
#26366 = CARTESIAN_POINT ( 'NONE',  ( 3.217454984196751688, -26.40825593670985327, 7.501983001166817822 ) ) ;
#26367 = CARTESIAN_POINT ( 'NONE',  ( 86.41034863701202084, -0.4798547535092105298, 5.807516434511641457 ) ) ;
#26368 = ORIENTED_EDGE ( 'NONE', *, *, #38211, .T. ) ;
#26369 = AXIS2_PLACEMENT_3D ( 'NONE', #36375, #7957, #24002 ) ;
#26370 = CARTESIAN_POINT ( 'NONE',  ( 5.140791489254627145, -28.92678305073006939, 7.697032948437507294 ) ) ;
#26371 = FACE_OUTER_BOUND ( 'NONE', #25296, .T. ) ;
#26372 =( NAMED_UNIT ( * ) SI_UNIT ( $, .STERADIAN. ) SOLID_ANGLE_UNIT ( ) );
#26373 = B_SPLINE_CURVE_WITH_KNOTS ( 'NONE', 3,
 ( #36646, #30270, #5153, #27170, #14807, #21003, #32960, #11711, #33384, #20789, #14003, #1674, #2086, #23678, #14205, #14598, #24287, #39727, #33581, #17896, #4950, #39317, #26574, #27375, #39114 ),
 .UNSPECIFIED., .F., .F.,
 ( 4, 3, 3, 3, 3, 3, 3, 3, 4 ),
 ( 6.468151674593734010E-05, 9.076621574721644293E-05, 0.0001210204262067928165, 0.0001512763324577402313, 0.0001815301820994173645, 0.0002117781465860688896, 0.0002420274594459692445, 0.0002722905548971095544, 0.0002816827545175569448 ),
 .UNSPECIFIED. ) ;
#26374 = CARTESIAN_POINT ( 'NONE',  ( -2.512558355278247557, -30.27627512112215058, 7.695279973900954751 ) ) ;
#26375 = LINE ( 'NONE', #10305, #12027 ) ;
#26376 = EDGE_LOOP ( 'NONE', ( #12584, #40428, #11945, #24051, #31653, #17340 ) ) ;
#26377 = CARTESIAN_POINT ( 'NONE',  ( 21.78882382717254274, 5.524186801048877271, 3.510389251737664473 ) ) ;
#26378 = CARTESIAN_POINT ( 'NONE',  ( 82.35726419014388000, 62.82676667106976254, -1.646077502936215797 ) ) ;
#26380 = EDGE_CURVE ( 'NONE', #5603, #35202, #31384, .T. ) ;
#26379 = FACE_OUTER_BOUND ( 'NONE', #1409, .T. ) ;
#26381 = ORIENTED_EDGE ( 'NONE', *, *, #38211, .F. ) ;
#26383 = CARTESIAN_POINT ( 'NONE',  ( 33.46455515056310759, -3.089188617792877789, 5.429351193206847448 ) ) ;
#26382 = CARTESIAN_POINT ( 'NONE',  ( 2.483678319220730568, -26.15870172506354763, 6.906857269533146493 ) ) ;
#26384 = FACE_OUTER_BOUND ( 'NONE', #18189, .T. ) ;
#26385 = CARTESIAN_POINT ( 'NONE',  ( 76.81217388538114221, 61.66049381551723485, 3.848392762315859361 ) ) ;
#26386 = ORIENTED_EDGE ( 'NONE', *, *, #40387, .T. ) ;
#26387 = CARTESIAN_POINT ( 'NONE',  ( 24.55753766420681217, 2.522355539012570702, -4.006862819802994302 ) ) ;
#26388 = CARTESIAN_POINT ( 'NONE',  ( -18.24874870218063450, -26.64985754041175525, 6.800000000000000711 ) ) ;
#26389 = AXIS2_PLACEMENT_3D ( 'NONE', #24837, #17453, #27911 ) ;
#26390 = CARTESIAN_POINT ( 'NONE',  ( -2.999244243438122126, -27.67182067344772278, 6.954324564059724878 ) ) ;
#26391 = CARTESIAN_POINT ( 'NONE',  ( 24.75065437802840052, 2.392517948343078960, -4.069336231166236217 ) ) ;
#26392 = CARTESIAN_POINT ( 'NONE',  ( -25.07867591359219617, -26.64985754041175525, 6.800000000000000711 ) ) ;
#26393 = CARTESIAN_POINT ( 'NONE',  ( -20.97867591359219475, -24.55319635012989110, 6.700000000000000178 ) ) ;
#26394 = CARTESIAN_POINT ( 'NONE',  ( 82.01669802222870942, 64.37834105533568163, 2.512558077907662391 ) ) ;
#26395 = CARTESIAN_POINT ( 'NONE',  ( -0.1815504582524301025, -32.52092734468801183, 6.880828092187098122 ) ) ;
#26396 = CARTESIAN_POINT ( 'NONE',  ( 33.86666996155606313, -5.260714354287511441, -2.203027216165969637 ) ) ;
#26397 = CARTESIAN_POINT ( 'NONE',  ( 2.388070188599133559, -26.24018815714575581, 7.774064877406527962 ) ) ;
#26398 = DIRECTION ( 'NONE',  ( 0.000000000000000000, 1.000000000000000000, 0.000000000000000000 ) ) ;
#26399 = CARTESIAN_POINT ( 'NONE',  ( -32.97867591359219119, -24.55319635012989110, 6.700000000000000178 ) ) ;
#26400 = LINE ( 'NONE', #38931, #35605 ) ;
#26401 = CARTESIAN_POINT ( 'NONE',  ( 78.20309482563492054, 60.29564352725032705, 2.640401424216431092 ) ) ;
#26402 = CIRCLE ( 'NONE', #39539, 4.357836081054403010 ) ;
#26403 = CARTESIAN_POINT ( 'NONE',  ( 35.47955784773917998, -1.848538386244011900, -5.743841097125561568 ) ) ;
#26404 = DIRECTION ( 'NONE',  ( 0.000000000000000000, 0.000000000000000000, 1.000000000000000000 ) ) ;
#26405 = CARTESIAN_POINT ( 'NONE',  ( 4.983308922979784228, -28.35648716565642857, 7.750000000000000000 ) ) ;
#26406 = CARTESIAN_POINT ( 'NONE',  ( -12.87867591359218977, -26.64985754041175525, 6.700000000000000178 ) ) ;
#26407 = CARTESIAN_POINT ( 'NONE',  ( -1.568403543439855552, -28.35049121020558260, 7.781480525794717273 ) ) ;
#26408 = ADVANCED_FACE ( 'NONE', ( #20951 ), #32912, .T. ) ;
#26409 = DIRECTION ( 'NONE',  ( -0.9267318687906785923, 0.3757233601570932335, 2.607104533349591435E-15 ) ) ;
#26410 = ORIENTED_EDGE ( 'NONE', *, *, #2780, .T. ) ;
#26411 = CARTESIAN_POINT ( 'NONE',  ( 36.17116650710612902, -3.462198426845603638, 5.816222086175844019 ) ) ;
#26412 = CARTESIAN_POINT ( 'NONE',  ( -70.48694192573870509, 0.1213051481704135875, 5.996540489601009050 ) ) ;
#26413 = CARTESIAN_POINT ( 'NONE',  ( 67.65011695904739497, 58.50773134691538502, -3.985511447369839644 ) ) ;
#26414 = CARTESIAN_POINT ( 'NONE',  ( 2.995714826359392902, -26.31843225177813395, 6.863784140767622333 ) ) ;
#26415 = EDGE_CURVE ( 'NONE', #10273, #35786, #14156, .T. ) ;
#26416 = ORIENTED_EDGE ( 'NONE', *, *, #10605, .F. ) ;
#26417 = LINE ( 'NONE', #35691, #22633 ) ;
#26418 = CARTESIAN_POINT ( 'NONE',  ( 3.831455443695943153, -32.21920586904128214, 7.784476445165072533 ) ) ;
#26419 = CARTESIAN_POINT ( 'NONE',  ( 85.37673136558751708, 1.331923910713227466, -5.551005466948024214 ) ) ;
#26420 = CARTESIAN_POINT ( 'NONE',  ( 0.9672887567242401952, -32.88995464571426197, 6.868387053540520704 ) ) ;
#26421 = CARTESIAN_POINT ( 'NONE',  ( 3.614428224949046253, -26.63966429966296090, 6.961115707816239784 ) ) ;
#26422 = CARTESIAN_POINT ( 'NONE',  ( -25.07867591359219617, -24.55319635012989110, 6.800000000000000711 ) ) ;
#26423 = VERTEX_POINT ( 'NONE', #316 ) ;
#26424 = CARTESIAN_POINT ( 'NONE',  ( 24.38923258654877202, 3.155769846838503589, 3.307240130081302798 ) ) ;
#26425 = CARTESIAN_POINT ( 'NONE',  ( -1.742531660465676202, -30.19946305178996226, 7.743886751744254227 ) ) ;
#26426 = CARTESIAN_POINT ( 'NONE',  ( 80.92403995952693663, 62.73960429493249791, 3.332694751021842094 ) ) ;
#26427 = AXIS2_PLACEMENT_3D ( 'NONE', #25723, #13352, #25927 ) ;
#26429 = EDGE_CURVE ( 'NONE', #2006, #31681, #5309, .T. ) ;
#26428 = CARTESIAN_POINT ( 'NONE',  ( 26.00772565174600359, -2.423984237576000123, -4.803821987795020121 ) ) ;
#26430 = ORIENTED_EDGE ( 'NONE', *, *, #26139, .F. ) ;
#26431 = CARTESIAN_POINT ( 'NONE',  ( 78.07232077886961008, 65.35672112437505632, -2.431999527814446171 ) ) ;
#26433 = CARTESIAN_POINT ( 'NONE',  ( -1.707806439853804648, -28.77356564420016838, 6.946906449495744873 ) ) ;
#26432 = CARTESIAN_POINT ( 'NONE',  ( 22.29628800937758015, 0.2617764422785469614, 7.104517024768484568 ) ) ;
#26434 = CARTESIAN_POINT ( 'NONE',  ( 81.42106526724015225, 61.53660244640850863, -1.679744683809659467 ) ) ;
#26435 = CARTESIAN_POINT ( 'NONE',  ( 80.49182418769538572, 61.81278841749719533, 2.961936469198068078 ) ) ;
#26436 = EDGE_LOOP ( 'NONE', ( #39075, #32501, #8138, #29527 ) ) ;
#26437 = LINE ( 'NONE', #22749, #7627 ) ;
#26438 = CARTESIAN_POINT ( 'NONE',  ( 82.09527124944457910, 65.20214329949105547, 1.328060019257126356 ) ) ;
#26439 = CARTESIAN_POINT ( 'NONE',  ( -0.8786759135921904385, -26.64985754041175525, 6.800000000000000711 ) ) ;
#26440 = CARTESIAN_POINT ( 'NONE',  ( 28.70293208761703241, -1.592347763559425200, -5.966126087555218227 ) ) ;
#26441 = CARTESIAN_POINT ( 'NONE',  ( -64.26379470914697833, 34.82012742686825391, -5.122105205699029717 ) ) ;
#26442 = ORIENTED_EDGE ( 'NONE', *, *, #40512, .F. ) ;
#26443 = CARTESIAN_POINT ( 'NONE',  ( -78.50546482259380809, -6.500811299971071655, 6.538465153154030318 ) ) ;
#26444 = CARTESIAN_POINT ( 'NONE',  ( 22.61749032200219034, 0.2966866550508970302, -6.491723916333954847 ) ) ;
#26445 = ADVANCED_FACE ( 'NONE', ( #31402 ), #12854, .F. ) ;
#26446 = CARTESIAN_POINT ( 'NONE',  ( -1.799609906766908907, -29.51351222115033934, 7.139253571461081194 ) ) ;
#26447 = DIRECTION ( 'NONE',  ( -0.000000000000000000, -0.000000000000000000, 1.000000000000000000 ) ) ;
#26448 = CARTESIAN_POINT ( 'NONE',  ( 34.63659524554710600, -0.7829862400395763977, -5.276330072109475466 ) ) ;
#26449 = CARTESIAN_POINT ( 'NONE',  ( 1.700390093233090871, -29.56993018339339940, -6.000000000000000000 ) ) ;
#26450 = DIRECTION ( 'NONE',  ( 0.000000000000000000, 0.000000000000000000, -1.000000000000000000 ) ) ;
#26451 = CARTESIAN_POINT ( 'NONE',  ( -14.34874870218063769, -25.49307895267003587, 6.800000000000000711 ) ) ;
#26452 = CARTESIAN_POINT ( 'NONE',  ( 2.684728112252080301, -32.82432899398588688, 6.895222827070020877 ) ) ;
#26453 = CARTESIAN_POINT ( 'NONE',  ( 2.670542827047279744, -32.83592445859822107, 7.386948897581449458 ) ) ;
#26454 = CARTESIAN_POINT ( 'NONE',  ( 1.300000000000000044, -0.5999999999999994227, -4.030609108440248889 ) ) ;
#26455 = ORIENTED_EDGE ( 'NONE', *, *, #2641, .T. ) ;
#26456 = EDGE_CURVE ( 'NONE', #2282, #6990, #8586, .T. ) ;
#26458 = EDGE_CURVE ( 'NONE', #3311, #30682, #21930, .T. ) ;
#26457 = CARTESIAN_POINT ( 'NONE',  ( 66.27376694608996388, 57.73522568913447373, 4.000000000000000000 ) ) ;
#26459 = CARTESIAN_POINT ( 'NONE',  ( 71.06822368831490166, 59.17031991972731930, -3.954977122261625233 ) ) ;
#26460 = CIRCLE ( 'NONE', #1485, 64.42751648247021024 ) ;
#26461 = EDGE_CURVE ( 'NONE', #38041, #33085, #612, .T. ) ;
#26462 = B_SPLINE_CURVE_WITH_KNOTS ( 'NONE', 3,
 ( #33670, #27473, #5448, #6214, #30575, #23573, #10992, #33046, #30367, #14904, #14291, #2382, #8309, #20672, #24381, #8722, #33474, #33877, #17780, #4836, #26862, #18759, #33256, #5042, #26665, #27069, #17571, #39611, #243, #31949, #7019 ),
 .UNSPECIFIED., .F., .F.,
 ( 4, 3, 3, 3, 3, 3, 3, 3, 3, 3, 4 ),
 ( 2.168404344971008868E-18, 3.077658087705444919E-05, 6.152638666998851537E-05, 9.267501192706007764E-05, 0.0001241882240135153495, 0.0001556618703051646587, 0.0001866161554452198913, 0.0002167966385860966021, 0.0002463805737537766221, 0.0002758761370306538454, 0.0002847094172290106869 ),
 .UNSPECIFIED. ) ;
#26463 = CARTESIAN_POINT ( 'NONE',  ( 84.65562454054800412, 2.508334066475362167, -3.654169056841765517 ) ) ;
#26464 = CARTESIAN_POINT ( 'NONE',  ( -80.04662500899941335, 10.46548227099173900, -6.327377141109288061 ) ) ;
#26465 = SHAPE_DEFINITION_REPRESENTATION ( #17779, #19830 ) ;
#26466 = CARTESIAN_POINT ( 'NONE',  ( -24.24874870218063450, -26.64985754041175525, 6.700000000000000178 ) ) ;
#26467 = FACE_OUTER_BOUND ( 'NONE', #12688, .T. ) ;
#26468 = LINE ( 'NONE', #29355, #28709 ) ;
#26469 = CARTESIAN_POINT ( 'NONE',  ( 1.751251297819361730, -25.49307895267003587, 6.800000000000000711 ) ) ;
#26470 = ORIENTED_EDGE ( 'NONE', *, *, #11187, .F. ) ;
#26471 = ADVANCED_FACE ( 'NONE', ( #9969 ), #3624, .T. ) ;
#26472 = EDGE_LOOP ( 'NONE', ( #39106, #35039, #1358, #18481, #25958, #14251, #550, #35845 ) ) ;
#26473 = CARTESIAN_POINT ( 'NONE',  ( 80.42678074443089997, 62.56544727678156903, -3.449595662144188779 ) ) ;
#26474 = CARTESIAN_POINT ( 'NONE',  ( 33.53294034083837261, -4.003968611202963324, 4.914558353369265831 ) ) ;
#26475 = CARTESIAN_POINT ( 'NONE',  ( 79.03665253560659210, 65.17130141867527016, 3.087291694836687306 ) ) ;
#26477 = VERTEX_POINT ( 'NONE', #11184 ) ;
#26476 = CARTESIAN_POINT ( 'NONE',  ( -70.92837670882107659, 28.72470171467712063, -6.406751979251626317 ) ) ;
#26478 = FACE_OUTER_BOUND ( 'NONE', #40560, .T. ) ;
#26479 = CARTESIAN_POINT ( 'NONE',  ( 3.924847313950914351, -26.99858887786119510, 6.892063359921932530 ) ) ;
#26480 = DIRECTION ( 'NONE',  ( -0.000000000000000000, -1.000000000000000000, -0.000000000000000000 ) ) ;
#26481 = CARTESIAN_POINT ( 'NONE',  ( 21.85643539959780313, -9.021070270546461600, 11.21731785579436291 ) ) ;
#26482 = CARTESIAN_POINT ( 'NONE',  ( 22.38220106028803613, 4.937111810673596501, -3.050830205725867383 ) ) ;
#26483 = ORIENTED_EDGE ( 'NONE', *, *, #30765, .T. ) ;
#26484 = CARTESIAN_POINT ( 'NONE',  ( 70.64516890162954610, 60.54534949351131701, -3.764670254805445371 ) ) ;
#26485 = VECTOR ( 'NONE', #2795, 1000.000000000000000 ) ;
#26486 = ORIENTED_EDGE ( 'NONE', *, *, #29343, .T. ) ;
#26487 = EDGE_CURVE ( 'NONE', #17020, #34298, #23757, .T. ) ;
#26488 = FACE_OUTER_BOUND ( 'NONE', #28175, .T. ) ;
#26489 = CARTESIAN_POINT ( 'NONE',  ( -75.35807269576923773, -3.444886077232420796, -9.005146983506810088 ) ) ;
#26490 = CARTESIAN_POINT ( 'NONE',  ( 5.142755578586930554, -28.93735303436349682, 7.651421919295142260 ) ) ;
#26491 = CYLINDRICAL_SURFACE ( 'NONE', #3087, 6.000000000000002665 ) ;
#26492 = CARTESIAN_POINT ( 'NONE',  ( 81.29039616289740877, 62.30485139745668732, 2.850064543546685591 ) ) ;
#26493 = CARTESIAN_POINT ( 'NONE',  ( -1.482088180267138622, -30.76652202637871625, 7.695279973900954751 ) ) ;
#26494 = DIRECTION ( 'NONE',  ( 0.000000000000000000, 0.000000000000000000, 1.000000000000000000 ) ) ;
#26495 = CARTESIAN_POINT ( 'NONE',  ( -2.395465747220443031, -30.94034030041199657, 6.894806418505347700 ) ) ;
#26496 = CARTESIAN_POINT ( 'NONE',  ( -1.641525177248355893, -30.19571155489859393, 7.693875151218753317 ) ) ;
#26497 = EDGE_CURVE ( 'NONE', #26946, #16350, #32435, .T. ) ;
#26498 = CARTESIAN_POINT ( 'NONE',  ( 4.416683729637440159, -27.36272632311469266, 6.875671892026060661 ) ) ;
#26499 = EDGE_CURVE ( 'NONE', #26146, #23756, #28484, .T. ) ;
#26500 = CARTESIAN_POINT ( 'NONE',  ( -0.3201374542954114055, -26.83543417321557101, 6.959317978105164393 ) ) ;
#26501 = CARTESIAN_POINT ( 'NONE',  ( 4.229935080175720508, -31.84180213379760715, 6.864276522220859711 ) ) ;
#26502 = CARTESIAN_POINT ( 'NONE',  ( 69.37860636825551808, 58.34396603459876474, 3.943722715026767300 ) ) ;
#26503 = CARTESIAN_POINT ( 'NONE',  ( 36.78928159892215177, -3.041397198625128695, 5.948255164286288199 ) ) ;
#26504 = ADVANCED_FACE ( 'NONE', ( #27863 ), #6056, .T. ) ;
#26505 = ORIENTED_EDGE ( 'NONE', *, *, #16777, .T. ) ;
#26506 = CARTESIAN_POINT ( 'NONE',  ( -35.07867591359219972, -24.55319635012989110, 6.700000000000000178 ) ) ;
#26507 = CARTESIAN_POINT ( 'NONE',  ( 87.15505355144220800, 0.4610318193416703680, -5.246243280819175681 ) ) ;
#26509 = CARTESIAN_POINT ( 'NONE',  ( 4.823919574101139141, -30.91291510963706912, 7.006423389747790331 ) ) ;
#26508 = CARTESIAN_POINT ( 'NONE',  ( 80.23319818986581708, 64.21721675003155383, -3.633989118465185353 ) ) ;
#26510 = CARTESIAN_POINT ( 'NONE',  ( 5.113812245512664667, -30.34358980514384285, 7.013842709614101167 ) ) ;
#26511 = CARTESIAN_POINT ( 'NONE',  ( -58.86630245980595788, 29.17574657131979521, 6.015288659391247350 ) ) ;
#26512 = ORIENTED_EDGE ( 'NONE', *, *, #8241, .F. ) ;
#26513 = CARTESIAN_POINT ( 'NONE',  ( -76.51582565984999462, 10.65402114766428987, -8.295614104186167737 ) ) ;
#26514 = CARTESIAN_POINT ( 'NONE',  ( -64.08758708074093136, 43.61223004741322740, -8.800414904976381791 ) ) ;
#26515 = ORIENTED_EDGE ( 'NONE', *, *, #20958, .T. ) ;
#26516 = LINE ( 'NONE', #26908, #22202 ) ;
#26517 = CARTESIAN_POINT ( 'NONE',  ( 78.67172310627755394, 65.99640245491987400, -1.621665796799209636 ) ) ;
#26518 = DIRECTION ( 'NONE',  ( 0.2312332387574689285, 0.9728983447892853853, 0.000000000000000000 ) ) ;
#26519 = CARTESIAN_POINT ( 'NONE',  ( 81.07009230622236373, 61.73904331373560694, 2.506402126386315654 ) ) ;
#26520 = CARTESIAN_POINT ( 'NONE',  ( 23.62669510910421167, 0.5457874777667105493, 5.460871266645791700 ) ) ;
#26521 = ORIENTED_EDGE ( 'NONE', *, *, #33518, .T. ) ;
#26522 = AXIS2_PLACEMENT_3D ( 'NONE', #31881, #34984, #12719 ) ;
#26523 = CARTESIAN_POINT ( 'NONE',  ( 5.002712648450646782, -28.73146642408099183, 7.505001789837627335 ) ) ;
#26525 = LINE ( 'NONE', #17235, #20318 ) ;
#26524 = CARTESIAN_POINT ( 'NONE',  ( 14.69558838330753936, 10.99631180437154399, -6.000000000000000888 ) ) ;
#26526 = PLANE ( 'NONE',  #7999 ) ;
#26527 = CARTESIAN_POINT ( 'NONE',  ( -63.63041988795695403, 43.97068632168673474, -2.480371489381162586 ) ) ;
#26528 = CARTESIAN_POINT ( 'NONE',  ( 4.095104150702293389, -32.13180824307641359, 7.139344958878409919 ) ) ;
#26529 = CARTESIAN_POINT ( 'NONE',  ( 21.76138600010604307, 5.847767184895531933, -3.374880873801382020 ) ) ;
#26530 = CARTESIAN_POINT ( 'NONE',  ( 5.123906412958439738, -30.28506088044589717, 7.766640943994651103 ) ) ;
#26531 = VECTOR ( 'NONE', #21365, 1000.000000000000000 ) ;
#26532 = ADVANCED_FACE ( 'NONE', ( #28274 ), #40624, .F. ) ;
#26533 = CARTESIAN_POINT ( 'NONE',  ( 21.85643539959775694, 4.180186707270823199, 11.06385087694989799 ) ) ;
#26534 = CARTESIAN_POINT ( 'NONE',  ( 21.26333942294113655, 9.593021065649088186, -2.042309770458127893 ) ) ;
#26535 = CARTESIAN_POINT ( 'NONE',  ( 15.67275371359048997, 8.062146741059187605, 3.484635839389762069 ) ) ;
#26536 = CARTESIAN_POINT ( 'NONE',  ( -42.83131703149249603, -29.56993018339339940, 6.000000000000000000 ) ) ;
#26537 = CARTESIAN_POINT ( 'NONE',  ( 79.37811825733636795, 65.99825290327245852, 2.263370276488442911 ) ) ;
#26538 = CARTESIAN_POINT ( 'NONE',  ( 87.00256539079671825, 0.09090593131677454641, 5.889906316148251442 ) ) ;
#26539 = CARTESIAN_POINT ( 'NONE',  ( -0.5125101069461969194, -26.98863734761392053, 7.695279973900954751 ) ) ;
#26540 = ORIENTED_EDGE ( 'NONE', *, *, #30371, .F. ) ;
#26541 = CARTESIAN_POINT ( 'NONE',  ( -76.83900407126830601, -4.548844688613328024, 9.590346143861395944 ) ) ;
#26542 = CARTESIAN_POINT ( 'NONE',  ( 18.24134202378618497, -2.850333121144178694, 3.053400609972546587 ) ) ;
#26543 = CARTESIAN_POINT ( 'NONE',  ( -38.24874870218063450, -26.64985754041175525, 6.700000000000000178 ) ) ;
#26544 = CARTESIAN_POINT ( 'NONE',  ( 14.73497390326914491, -4.430518890905947416, -2.506147062932408520 ) ) ;
#26545 = CARTESIAN_POINT ( 'NONE',  ( 30.51508027424239700, -0.1407365609915100790, -4.969014305437574386 ) ) ;
#26546 = DIRECTION ( 'NONE',  ( 0.000000000000000000, 0.000000000000000000, -1.000000000000000000 ) ) ;
#26547 = CARTESIAN_POINT ( 'NONE',  ( 85.36230419630793165, 1.362237581505277406, 5.546959353559891781 ) ) ;
#26548 = CARTESIAN_POINT ( 'NONE',  ( -34.24874870218063450, -26.64985754041175525, 6.700000000000000178 ) ) ;
#26549 = EDGE_LOOP ( 'NONE', ( #21389, #10690, #40466, #37359 ) ) ;
#26550 = CARTESIAN_POINT ( 'NONE',  ( -51.01549048184568846, -30.38627270959228710, 6.000000000000000000 ) ) ;
#26551 = EDGE_CURVE ( 'NONE', #30676, #31330, #39656, .T. ) ;
#26552 = CARTESIAN_POINT ( 'NONE',  ( 3.412070287718869999, -32.50764203308273181, 7.635761828346577573 ) ) ;
#26553 = VECTOR ( 'NONE', #9222, 1000.000000000000000 ) ;
#26554 = EDGE_CURVE ( 'NONE', #12935, #6584, #14752, .T. ) ;
#26555 = CARTESIAN_POINT ( 'NONE',  ( -1.135370486211617180, -27.69417381966504621, 6.929923840112066635 ) ) ;
#26556 = ORIENTED_EDGE ( 'NONE', *, *, #17506, .F. ) ;
#26557 = VERTEX_POINT ( 'NONE', #30566 ) ;
#26558 = CARTESIAN_POINT ( 'NONE',  ( 33.94626592564545575, -0.4876026740605987619, 5.120945191898142568 ) ) ;
#26559 = CARTESIAN_POINT ( 'NONE',  ( -1.645942781641917430, -30.59564475252808435, 6.998987538705431888 ) ) ;
#26560 = CARTESIAN_POINT ( 'NONE',  ( 66.27376694609004915, 57.73522568913436004, -4.000000000000000000 ) ) ;
#26561 = CARTESIAN_POINT ( 'NONE',  ( 87.85437433257010298, -2.425468598688185207, 1.529927975848801136 ) ) ;
#26562 = AXIS2_PLACEMENT_3D ( 'NONE', #13094, #12273, #22382 ) ;
#26563 = VERTEX_POINT ( 'NONE', #21906 ) ;
#26564 = VERTEX_POINT ( 'NONE', #30777 ) ;
#26565 = LINE ( 'NONE', #36233, #37803 ) ;
#26566 =( BOUNDED_CURVE ( )  B_SPLINE_CURVE ( 3, ( #23309, #36076, #10933, #7853 ),
 .UNSPECIFIED., .F., .T. ) 
 B_SPLINE_CURVE_WITH_KNOTS ( ( 4, 4 ),
 ( 1.570796326794896780, 1.574767692156076260 ),
 .UNSPECIFIED. ) 
 CURVE ( )  GEOMETRIC_REPRESENTATION_ITEM ( )  RATIONAL_B_SPLINE_CURVE ( ( 1.000000000000000000, 0.9999986856885290099, 0.9999986856885290099, 1.000000000000000000 ) ) 
 REPRESENTATION_ITEM ( '' )  );
#26567 = CARTESIAN_POINT ( 'NONE',  ( -57.65239026484333351, 32.60637517809080066, -4.103028154974615482 ) ) ;
#26568 = CARTESIAN_POINT ( 'NONE',  ( 21.91948103535845505, 3.888016741293982115, 2.591533416524685960E-12 ) ) ;
#26569 = VERTEX_POINT ( 'NONE', #2376 ) ;
#26570 = CARTESIAN_POINT ( 'NONE',  ( 24.20056197448974089, 3.097996102763779902, 3.573029051228984621 ) ) ;
#26571 = CARTESIAN_POINT ( 'NONE',  ( 79.65107971589624469, 66.31509156740916922, -1.306649493517272553 ) ) ;
#26572 = CARTESIAN_POINT ( 'NONE',  ( -1.312560436656866392, -31.35097737660188244, 7.695279973900954751 ) ) ;
#26573 = EDGE_LOOP ( 'NONE', ( #21271, #37023, #25666, #202 ) ) ;
#26575 = CARTESIAN_POINT ( 'NONE',  ( 14.89512109076932944, -4.197941490224893712, -2.531141904716178725 ) ) ;
#26574 = CARTESIAN_POINT ( 'NONE',  ( 0.1031518550754170205, -26.56845796774315716, 7.759451378593098525 ) ) ;
#26576 = CARTESIAN_POINT ( 'NONE',  ( -38.34874870218063592, -26.64985754041175525, 6.700000000000000178 ) ) ;
#26577 = CARTESIAN_POINT ( 'NONE',  ( 74.98537949548503434, 62.60475170799649192, 3.615102801931181276 ) ) ;
#26578 = CARTESIAN_POINT ( 'NONE',  ( 22.26754414936907267, 2.303131529692775459, -5.275206787684171950 ) ) ;
#26579 = DIRECTION ( 'NONE',  ( 1.000000000000000000, 0.000000000000000000, 0.000000000000000000 ) ) ;
#26580 = AXIS2_PLACEMENT_3D ( 'NONE', #11951, #27207, #14438 ) ;
#26581 = DIRECTION ( 'NONE',  ( -1.000000000000000000, 0.000000000000000000, 0.000000000000000000 ) ) ;
#26582 = DIRECTION ( 'NONE',  ( 1.000000000000000000, 7.232507224765808510E-18, 0.000000000000000000 ) ) ;
#26583 = CARTESIAN_POINT ( 'NONE',  ( 0.1967285774411879351, -25.49757015976072694, 7.013842709614101167 ) ) ;
#26584 = FACE_OUTER_BOUND ( 'NONE', #3309, .T. ) ;
#26586 = CARTESIAN_POINT ( 'NONE',  ( 81.16771000429746152, 61.30329618601649599, 1.041818241550642954 ) ) ;
#26585 = APPLICATION_CONTEXT ( 'automotive_design' ) ;
#26587 = CARTESIAN_POINT ( 'NONE',  ( 86.00040182524281818, 1.757991441285688961, 4.533237565279400805 ) ) ;
#26588 = CARTESIAN_POINT ( 'NONE',  ( 32.62845853548997610, -2.537451394787784142, 5.899574533259067444 ) ) ;
#26589 = DIRECTION ( 'NONE',  ( 0.000000000000000000, 0.000000000000000000, 1.000000000000000000 ) ) ;
#26590 = CARTESIAN_POINT ( 'NONE',  ( -72.12105268511338352, -46.20207945875944944, 9.928773179615475897 ) ) ;
#26591 = CIRCLE ( 'NONE', #29241, 8.080217238368769372 ) ;
#26592 = CARTESIAN_POINT ( 'NONE',  ( -77.95630793809591808, -5.091041188919200877, -8.764182688739834859 ) ) ;
#26593 = VERTEX_POINT ( 'NONE', #9536 ) ;
#26594 = CARTESIAN_POINT ( 'NONE',  ( -12.87867591359218977, -26.64985754041175525, 6.800000000000000711 ) ) ;
#26595 = CARTESIAN_POINT ( 'NONE',  ( 0.1197244639376408848, -26.44719159565006095, 6.961115707816241560 ) ) ;
#26596 = CARTESIAN_POINT ( 'NONE',  ( 35.33516124645243650, -3.300847515999512094, -5.721304515250182909 ) ) ;
#26597 = FACE_OUTER_BOUND ( 'NONE', #2439, .T. ) ;
#26598 = CARTESIAN_POINT ( 'NONE',  ( 4.980322978310361748, -28.34843557914865286, 7.737115613922532553 ) ) ;
#26599 = CARTESIAN_POINT ( 'NONE',  ( -72.95330471031414277, 33.71485196875532608, 12.49999999999999645 ) ) ;
#26600 = ADVANCED_FACE ( 'NONE', ( #22118, #2998 ), #14895, .T. ) ;
#26601 = CYLINDRICAL_SURFACE ( 'NONE', #17774, 0.1000000000000028644 ) ;
#26602 = EDGE_CURVE ( 'NONE', #32530, #17047, #15516, .T. ) ;
#26603 = DIRECTION ( 'NONE',  ( -0.7126435865141277359, 0.000000000000000000, 0.7015262779114412872 ) ) ;
#26604 = VERTEX_POINT ( 'NONE', #11790 ) ;
#26605 = CARTESIAN_POINT ( 'NONE',  ( 31.93464789591948261, 0.01672602609938712154, 5.060956730290721239 ) ) ;
#26606 = CARTESIAN_POINT ( 'NONE',  ( -69.94741522153590552, -0.5593530815884721896, 5.931425411825930638 ) ) ;
#26607 = CARTESIAN_POINT ( 'NONE',  ( 67.40765644887963504, 58.26613713413648554, -3.996173465816880377 ) ) ;
#26608 = CARTESIAN_POINT ( 'NONE',  ( 4.721744115977328349, -27.80317613450962355, 7.643192810543820492 ) ) ;
#26609 = CIRCLE ( 'NONE', #34544, 0.1000000000000028644 ) ;
#26610 = VERTEX_POINT ( 'NONE', #18393 ) ;
#26611 = VECTOR ( 'NONE', #8793, 1000.000000000000000 ) ;
#26612 = B_SPLINE_CURVE_WITH_KNOTS ( 'NONE', 3,
 ( #10424, #26289, #29170, #26484, #13516, #7934, #20285, #23000, #39011, #23592, #1575, #32465, #23190, #14107, #4264, #4656, #10614, #35565, #4470, #13723, #29369, #26685 ),
 .UNSPECIFIED., .F., .F.,
 ( 4, 2, 2, 2, 2, 2, 2, 2, 2, 2, 4 ),
 ( -7.124770226877074144E-05, 0.003831421772206580582, 0.007734091246681932055, 0.009685425983919597817, 0.01163676072115726184, 0.01261242808977608952, 0.01358809545839491720, 0.01456376282701374487, 0.01505159651132314397, 0.01529551335347784438, 0.01553943019563254133 ),
 .UNSPECIFIED. ) ;
#26613 = DIRECTION ( 'NONE',  ( 0.9848077530122081313, 0.1736481776669300814, 0.000000000000000000 ) ) ;
#26614 = CARTESIAN_POINT ( 'NONE',  ( 3.913290293412392096, -32.15122301917286762, 7.703977250142849620 ) ) ;
#26615 = CARTESIAN_POINT ( 'NONE',  ( 85.95116560976015307, 0.3509943572283380497, -5.999998676670047715 ) ) ;
#26616 = CARTESIAN_POINT ( 'NONE',  ( -42.24874870218063450, -26.64985754041175525, 6.700000000000000178 ) ) ;
#26617 = CARTESIAN_POINT ( 'NONE',  ( 3.596532054354828922, -26.62805159003958266, 7.011627023500182965 ) ) ;
#26618 = CARTESIAN_POINT ( 'NONE',  ( 1.263793096374429492, -26.09726748785000083, 7.009310105710487626 ) ) ;
#26619 = ORIENTED_EDGE ( 'NONE', *, *, #40387, .F. ) ;
#26620 = CARTESIAN_POINT ( 'NONE',  ( 22.61872426168702077, 4.601640665309255418, 3.069969487110096207 ) ) ;
#26621 = CARTESIAN_POINT ( 'NONE',  ( 1.664433243520589967, -33.27093018339341768, 7.695279973900954751 ) ) ;
#26622 = CARTESIAN_POINT ( 'NONE',  ( 80.20683918224330000, 64.20264744734686246, 3.640670270625568694 ) ) ;
#26623 = MANIFOLD_SOLID_BREP ( 'Boss-Extrude4', #26230 ) ;
#26624 = CARTESIAN_POINT ( 'NONE',  ( 6.107923577950775673, -31.97397320985677993, 7.754798119455333705 ) ) ;
#26625 = ORIENTED_EDGE ( 'NONE', *, *, #7037, .T. ) ;
#26626 = CARTESIAN_POINT ( 'NONE',  ( 79.50866325991145800, 61.15032965923182218, -2.842954625922232026 ) ) ;
#26628 = CARTESIAN_POINT ( 'NONE',  ( -1.725425523115296622, -28.85306876528290942, 6.864293497989290671 ) ) ;
#26627 = CARTESIAN_POINT ( 'NONE',  ( 24.73536326808030950, 0.6125365926123585991, 4.779974774574727192 ) ) ;
#26629 = CARTESIAN_POINT ( 'NONE',  ( 81.50569694087069195, 63.36683741555938809, -3.125353918834852696 ) ) ;
#26630 = EDGE_CURVE ( 'NONE', #9389, #21810, #12219, .T. ) ;
#26631 = CARTESIAN_POINT ( 'NONE',  ( 79.89463791284350691, 61.88150425735624083, 3.258123098320697686 ) ) ;
#26632 = EDGE_LOOP ( 'NONE', ( #39310, #9461, #31230, #25566 ) ) ;
#26633 = CARTESIAN_POINT ( 'NONE',  ( -0.8583414810284668572, -27.33095856289763859, 7.784476445165075198 ) ) ;
#26634 = CARTESIAN_POINT ( 'NONE',  ( 81.74417899799371412, 61.69322615925147346, 1.090531591958330937 ) ) ;
#26636 = ORIENTED_EDGE ( 'NONE', *, *, #30031, .F. ) ;
#26635 = CARTESIAN_POINT ( 'NONE',  ( -12.24874870218063627, -25.49307895267003587, 6.800000000000000711 ) ) ;
#26637 = B_SPLINE_CURVE_WITH_KNOTS ( 'NONE', 3,
 ( #40439, #9359, #31821, #37974, #21942, #34723, #24609, #6704, #6503, #19252, #37365, #326, #24821, #12030, #8949, #31615, #18620, #9160, #12866, #3438, #21735, #9778, #34316, #15133, #31209 ),
 .UNSPECIFIED., .F., .F.,
 ( 4, 3, 3, 3, 3, 3, 3, 3, 4 ),
 ( 6.468151674593626945E-05, 9.076621574721905857E-05, 0.0001210204262067960963, 0.0001512763324577423183, 0.0001815301820994208069, 0.0002117781465860700822, 0.0002420274594459736626, 0.0002722905548971149212, 0.0002816827545175583543 ),
 .UNSPECIFIED. ) ;
#26638 = CARTESIAN_POINT ( 'NONE',  ( 24.33259761278756272, 0.1721304915443387373, 6.926443425830641765 ) ) ;
#26639 = CARTESIAN_POINT ( 'NONE',  ( -64.85784325972053921, 34.81586596186942018, -6.466735817496056526 ) ) ;
#26640 = ORIENTED_EDGE ( 'NONE', *, *, #13331, .T. ) ;
#26641 = CARTESIAN_POINT ( 'NONE',  ( -80.93415443611787907, -6.594512348378300359, 0.2227253658375672740 ) ) ;
#26642 = CARTESIAN_POINT ( 'NONE',  ( 26.04620955633046009, 0.8112080387504423395, -4.422430910127713055 ) ) ;
#26643 = EDGE_CURVE ( 'NONE', #5611, #34412, #9132, .T. ) ;
#26644 = ORIENTED_EDGE ( 'NONE', *, *, #33705, .T. ) ;
#26645 = AXIS2_PLACEMENT_3D ( 'NONE', #35583, #38432, #9841 ) ;
#26646 = CIRCLE ( 'NONE', #38468, 6.000000000000002665 ) ;
#26647 = CARTESIAN_POINT ( 'NONE',  ( 5.165377781178596805, -29.07610802675595707, 6.865482280155369210 ) ) ;
#26648 = CARTESIAN_POINT ( 'NONE',  ( 34.13626153038629951, -3.787416908594791742, -5.295464026636712340 ) ) ;
#26649 = B_SPLINE_CURVE_WITH_KNOTS ( 'NONE', 3,
 ( #37656, #9054, #12967, #6796, #9458, #3730, #21631, #34212, #18521, #19146 ),
 .UNSPECIFIED., .F., .F.,
 ( 4, 2, 2, 2, 4 ),
 ( 0.000000000000000000, 0.0003392619605000338277, 0.0005088929407500506060, 0.0005937084308750540350, 0.0006785239210000574639 ),
 .UNSPECIFIED. ) ;
#26650 = CARTESIAN_POINT ( 'NONE',  ( 3.791157483716739218, -32.25110375459131973, 7.754798119455333705 ) ) ;
#26651 = CARTESIAN_POINT ( 'NONE',  ( 5.117081926811264836, -30.32907536032250206, 6.880828092187096345 ) ) ;
#26652 = DIRECTION ( 'NONE',  ( 1.000000000000000000, 0.000000000000000000, 0.000000000000000000 ) ) ;
#26653 = CARTESIAN_POINT ( 'NONE',  ( 2.765119862722436928, -32.79893335921538977, 6.864651958020304257 ) ) ;
#26654 = AXIS2_PLACEMENT_3D ( 'NONE', #26864, #11197, #27073 ) ;
#26655 = CARTESIAN_POINT ( 'NONE',  ( 1.892167102583406146, -26.07518817540235645, 6.941203072598474577 ) ) ;
#26656 = CARTESIAN_POINT ( 'NONE',  ( 21.99236933195925658, 1.173799028591102189, -6.729090458912794226 ) ) ;
#26657 = EDGE_CURVE ( 'NONE', #2179, #19731, #7058, .T. ) ;
#26658 = EDGE_LOOP ( 'NONE', ( #33673, #28843, #31223, #20367, #4796 ) ) ;
#26659 = CARTESIAN_POINT ( 'NONE',  ( 66.57179245706689130, 57.82874523672322908, 3.999903336035371293 ) ) ;
#26660 = CARTESIAN_POINT ( 'NONE',  ( 71.95566904218743787, 60.28642714153433957, -3.942504219403032639 ) ) ;
#26661 = ORIENTED_EDGE ( 'NONE', *, *, #24167, .T. ) ;
#26662 = CARTESIAN_POINT ( 'NONE',  ( 86.79384979562775015, -0.7021008148363506729, 5.624057257660853182 ) ) ;
#26663 = FACE_OUTER_BOUND ( 'NONE', #13340, .T. ) ;
#26664 = CARTESIAN_POINT ( 'NONE',  ( -2.348748702180637693, -26.64985754041175525, 6.800000000000000711 ) ) ;
#26665 = CARTESIAN_POINT ( 'NONE',  ( -0.8559337256230342694, -27.17927995110327188, 6.980586498568965403 ) ) ;
#26666 = DIRECTION ( 'NONE',  ( 0.000000000000000000, 1.000000000000000000, 0.000000000000000000 ) ) ;
#26667 = DIRECTION ( 'NONE',  ( -1.000000000000000000, 0.000000000000000000, 0.000000000000000000 ) ) ;
#26668 = CARTESIAN_POINT ( 'NONE',  ( 2.431875535358183793, -26.14722233025152676, 7.750000000000000888 ) ) ;
#26669 = VECTOR ( 'NONE', #18900, 1000.000000000000000 ) ;
#26670 = AXIS2_PLACEMENT_3D ( 'NONE', #34033, #30309, #34239 ) ;
#26671 = ORIENTED_EDGE ( 'NONE', *, *, #24636, .F. ) ;
#26672 = VERTEX_POINT ( 'NONE', #16126 ) ;
#26673 = CARTESIAN_POINT ( 'NONE',  ( 80.58270521159307975, 62.07868998654234360, -3.101774481621347945 ) ) ;
#26674 = CARTESIAN_POINT ( 'NONE',  ( 33.88293910487175964, -5.368702826017877960, 1.511118951966003987 ) ) ;
#26675 = EDGE_CURVE ( 'NONE', #24927, #14959, #12635, .T. ) ;
#26676 = CARTESIAN_POINT ( 'NONE',  ( 78.47952394835844814, 65.90892955575914414, 1.487544896895793389 ) ) ;
#26677 = PLANE ( 'NONE',  #26929 ) ;
#26678 = VECTOR ( 'NONE', #2209, 1000.000000000000000 ) ;
#26679 = FACE_OUTER_BOUND ( 'NONE', #19090, .T. ) ;
#26680 = CARTESIAN_POINT ( 'NONE',  ( 19.75425538659450453, 11.81160871140306767, 2.500000000000000444 ) ) ;
#26681 = EDGE_CURVE ( 'NONE', #12108, #28243, #30289, .T. ) ;
#26682 = CARTESIAN_POINT ( 'NONE',  ( 21.85643539959776049, -13.25144142801168634, -1.676981927294508345 ) ) ;
#26683 = DIRECTION ( 'NONE',  ( -1.000000000000000000, 0.000000000000000000, 0.000000000000000000 ) ) ;
#26684 = ORIENTED_EDGE ( 'NONE', *, *, #3834, .F. ) ;
#26685 = CARTESIAN_POINT ( 'NONE',  ( 78.69038500580363404, 66.05859403932464602, -1.000000000000000000 ) ) ;
#26686 = ADVANCED_FACE ( 'NONE', ( #32200 ), #19220, .F. ) ;
#26687 = ORIENTED_EDGE ( 'NONE', *, *, #1494, .F. ) ;
#26688 = CARTESIAN_POINT ( 'NONE',  ( 14.73615518778700029, -5.027433023050646099, 2.500473092695826072 ) ) ;
#26689 = CARTESIAN_POINT ( 'NONE',  ( -79.06668015796786619, 10.34652177153921926, -5.823291136487683595 ) ) ;
#26690 = CARTESIAN_POINT ( 'NONE',  ( 0.1649012726517564975, -26.53640515764040231, 7.013842709614101167 ) ) ;
#26691 = CARTESIAN_POINT ( 'NONE',  ( 2.372793067090987584, -26.23708241598081514, 6.870716933885664623 ) ) ;
#26692 = CARTESIAN_POINT ( 'NONE',  ( 78.66788830423078593, 66.04261347698269446, 1.159471704397124547 ) ) ;
#26693 = CARTESIAN_POINT ( 'NONE',  ( -32.34874870218063592, -26.64985754041175525, 6.800000000000000711 ) ) ;
#26694 = CARTESIAN_POINT ( 'NONE',  ( -2.978675913592195190, -26.64985754041175525, 6.700000000000000178 ) ) ;
#26695 = LINE ( 'NONE', #10824, #35244 ) ;
#26696 = CARTESIAN_POINT ( 'NONE',  ( 31.02880894190926142, -0.3131658439163265695, 5.049194088601750785 ) ) ;
#26697 = CIRCLE ( 'NONE', #14195, 2.500000000000000000 ) ;
#26698 = CARTESIAN_POINT ( 'NONE',  ( -64.19126555651345711, 34.97929361893064026, 4.821066086844552068 ) ) ;
#26699 = CARTESIAN_POINT ( 'NONE',  ( 87.35326390485820980, 0.2383925427539270170, 4.560928763750174753 ) ) ;
#26700 = CARTESIAN_POINT ( 'NONE',  ( 4.167347423248069838, -31.90961425007534658, 6.929923840112069300 ) ) ;
#26701 = EDGE_CURVE ( 'NONE', #28895, #6408, #29297, .T. ) ;
#26702 = DIRECTION ( 'NONE',  ( 1.000000000000000000, 0.000000000000000000, 0.000000000000000000 ) ) ;
#26703 = CARTESIAN_POINT ( 'NONE',  ( 67.68985761519660116, 58.40038676363953840, 3.993918888840239934 ) ) ;
#26704 = CARTESIAN_POINT ( 'NONE',  ( 36.79824929224523089, -3.072007531421248494, 5.949654789713833658 ) ) ;
#26705 = AXIS2_PLACEMENT_3D ( 'NONE', #20396, #5168, #2097 ) ;
#26706 = CARTESIAN_POINT ( 'NONE',  ( 1.158056475448751454, -26.21346265829786049, 6.894806418505346812 ) ) ;
#26707 = CARTESIAN_POINT ( 'NONE',  ( 85.43834401013396018, 2.333645700298356829, -4.102255839672300120 ) ) ;
#26709 = DIRECTION ( 'NONE',  ( -0.9848077530122149037, 0.1736481776668921395, 0.000000000000000000 ) ) ;
#26708 = CARTESIAN_POINT ( 'NONE',  ( 79.55838722571232324, 65.27247487857083286, -3.155412080370053385 ) ) ;
#26710 = CARTESIAN_POINT ( 'NONE',  ( 5.162074113069795800, -30.13065620592465876, 7.255881584735161205 ) ) ;
#26711 = CARTESIAN_POINT ( 'NONE',  ( -57.26775771055920217, 29.21795897888089755, 2.148764163877427968 ) ) ;
#26712 = ORIENTED_EDGE ( 'NONE', *, *, #3155, .T. ) ;
#26713 = DIRECTION ( 'NONE',  ( -1.000000000000000000, 0.000000000000000000, 0.000000000000000000 ) ) ;
#26714 = CARTESIAN_POINT ( 'NONE',  ( 4.870584666682655772, -30.79873755356147669, 7.784476445165072533 ) ) ;
#26715 = ORIENTED_EDGE ( 'NONE', *, *, #2692, .F. ) ;
#26716 = LINE ( 'NONE', #1222, #2483 ) ;
#26717 = ORIENTED_EDGE ( 'NONE', *, *, #34724, .T. ) ;
#26718 = CARTESIAN_POINT ( 'NONE',  ( 78.74908976354470269, 65.92676629176580150, -1.950029235564220809 ) ) ;
#26719 = CARTESIAN_POINT ( 'NONE',  ( 24.97416265246179634, 3.401756802687047720, -1.620313636369559829 ) ) ;
#26720 = CARTESIAN_POINT ( 'NONE',  ( 79.27128227901764035, 65.37053819277495847, 2.988136994358710385 ) ) ;
#26721 = CARTESIAN_POINT ( 'NONE',  ( 23.18800229536432767, 0.6779291438705001838, 5.705356198791737832 ) ) ;
#26723 = ORIENTED_EDGE ( 'NONE', *, *, #22914, .T. ) ;
#26722 = CARTESIAN_POINT ( 'NONE',  ( -0.9894248136993964993, -27.33053388830764874, 7.635761828346571356 ) ) ;
#26724 = EDGE_CURVE ( 'NONE', #19656, #6556, #28482, .T. ) ;
#26725 = CARTESIAN_POINT ( 'NONE',  ( -0.08465666289843364056, -32.46366374979973557, 7.774064877406527962 ) ) ;
#26727 = DIRECTION ( 'NONE',  ( 1.000000000000000000, 0.000000000000000000, 0.000000000000000000 ) ) ;
#26726 = DIRECTION ( 'NONE',  ( -1.000000000000000000, 0.000000000000000000, -2.891205793294675861E-16 ) ) ;
#26728 = DIRECTION ( 'NONE',  ( 0.000000000000000000, 0.000000000000000000, 1.000000000000000000 ) ) ;
#26729 = EDGE_CURVE ( 'NONE', #28383, #27482, #13432, .T. ) ;
#26730 = CARTESIAN_POINT ( 'NONE',  ( -23.07867591359219617, -26.64985754041175525, 6.700000000000000178 ) ) ;
#26731 = CARTESIAN_POINT ( 'NONE',  ( 24.60713993353984463, 2.981604336055061477, -3.554838876931238012 ) ) ;
#26732 = ORIENTED_EDGE ( 'NONE', *, *, #32002, .T. ) ;
#26733 = CARTESIAN_POINT ( 'NONE',  ( 5.135438731485244546, -30.19400213985234060, 7.778495531946297170 ) ) ;
#26734 = AXIS2_PLACEMENT_3D ( 'NONE', #23097, #35664, #26190 ) ;
#26735 = ADVANCED_FACE ( 'NONE', ( #13236 ), #35092, .F. ) ;
#26736 = CARTESIAN_POINT ( 'NONE',  ( 21.85643539959774273, 9.255709152629782110, 0.01215589129642568461 ) ) ;
#26737 = CARTESIAN_POINT ( 'NONE',  ( 15.87703778079246852, 7.971370532067864723, 3.484773800359326490 ) ) ;
#26738 = LINE ( 'NONE', #17648, #25467 ) ;
#26739 = AXIS2_PLACEMENT_3D ( 'NONE', #15537, #12022, #6076 ) ;
#26740 = CARTESIAN_POINT ( 'NONE',  ( 79.79491195507890211, 65.71105728010107327, 2.731335034814814211 ) ) ;
#26741 = CARTESIAN_POINT ( 'NONE',  ( 84.76444386024292044, 2.549623173165235457, -3.635552437183829699 ) ) ;
#26742 = LINE ( 'NONE', #39281, #6900 ) ;
#26743 = EDGE_LOOP ( 'NONE', ( #801, #39985, #28182, #33162 ) ) ;
#26744 = CARTESIAN_POINT ( 'NONE',  ( 0.5713750229309367823, -32.77700439067807281, 7.695279973900954751 ) ) ;
#26745 = ORIENTED_EDGE ( 'NONE', *, *, #32427, .F. ) ;
#26746 = DIRECTION ( 'NONE',  ( -0.000000000000000000, -1.000000000000000000, -0.000000000000000000 ) ) ;
#26747 = CARTESIAN_POINT ( 'NONE',  ( 19.67387626504557119, -2.726682240971237903, -3.276982224292623425 ) ) ;
#26748 = CARTESIAN_POINT ( 'NONE',  ( 36.97888601131364794, -2.955670041283646743, -5.977847518440031038 ) ) ;
#26749 = DIRECTION ( 'NONE',  ( 0.000000000000000000, 0.000000000000000000, 1.000000000000000000 ) ) ;
#26750 = CARTESIAN_POINT ( 'NONE',  ( 22.09089903963538504, 0.3679612555529369611, -7.362811209300283544 ) ) ;
#26751 = FACE_OUTER_BOUND ( 'NONE', #27390, .T. ) ;
#26752 = EDGE_LOOP ( 'NONE', ( #21998, #1176, #16186, #10864 ) ) ;
#26753 = CARTESIAN_POINT ( 'NONE',  ( 36.90998175379526458, -2.640409580673696244, 5.967093342598490224 ) ) ;
#26754 = FACE_OUTER_BOUND ( 'NONE', #40537, .T. ) ;
#26755 = AXIS2_PLACEMENT_3D ( 'NONE', #13172, #25732, #40541 ) ;
#26756 = CARTESIAN_POINT ( 'NONE',  ( 5.007838232645942078, -28.45671592495904179, 7.780491323090172884 ) ) ;
#26757 = VERTEX_POINT ( 'NONE', #288 ) ;
#26758 = VERTEX_POINT ( 'NONE', #4000 ) ;
#26759 = CARTESIAN_POINT ( 'NONE',  ( 35.83237527962609903, -3.728971877112755795, 5.623842631175056006 ) ) ;
#26760 = CARTESIAN_POINT ( 'NONE',  ( -1.623020518067741502, -30.66767645291113453, 6.863784140767622333 ) ) ;
#26761 = CIRCLE ( 'NONE', #8994, 7.744449365083023729 ) ;
#26762 = CARTESIAN_POINT ( 'NONE',  ( 66.27376694609004915, 57.73522568913436004, -4.000000000000000000 ) ) ;
#26763 = VECTOR ( 'NONE', #29969, 1000.000000000000000 ) ;
#26764 = CARTESIAN_POINT ( 'NONE',  ( 86.31797065848635953, -0.3216205983069810870, 5.878345525829285378 ) ) ;
#26765 = AXIS2_PLACEMENT_3D ( 'NONE', #36556, #26885, #5265 ) ;
#26766 = EDGE_LOOP ( 'NONE', ( #18515, #14577, #765, #31235 ) ) ;
#26767 = EDGE_LOOP ( 'NONE', ( #4100, #30148, #7057, #19553 ) ) ;
#26768 = DIRECTION ( 'NONE',  ( -0.1736481776669340227, 0.9848077530122073542, -0.000000000000000000 ) ) ;
#26769 = ORIENTED_EDGE ( 'NONE', *, *, #17986, .F. ) ;
#26770 = DIRECTION ( 'NONE',  ( -1.000000000000000000, 0.000000000000000000, 0.000000000000000000 ) ) ;
#26771 = CARTESIAN_POINT ( 'NONE',  ( 4.819850852585312317, -27.98280284135210749, 6.989977667959443863 ) ) ;
#26772 = ORIENTED_EDGE ( 'NONE', *, *, #992, .F. ) ;
#26773 = ADVANCED_FACE ( 'NONE', ( #25801 ), #26214, .F. ) ;
#26774 = CARTESIAN_POINT ( 'NONE',  ( 22.36021236311070837, 4.293190201525941774, 3.667803422475389930 ) ) ;
#26775 = CARTESIAN_POINT ( 'NONE',  ( 78.68971998042104588, 66.05812159354535140, -1.027726681410898957 ) ) ;
#26776 = ADVANCED_FACE ( 'NONE', ( #38142 ), #7258, .F. ) ;
#26777 = CARTESIAN_POINT ( 'NONE',  ( -1.312638530291446948, -31.35084526104921920, 7.700536657684216024 ) ) ;
#26778 = ORIENTED_EDGE ( 'NONE', *, *, #25078, .T. ) ;
#26780 = CARTESIAN_POINT ( 'NONE',  ( 23.66263933634246541, -2.671893037885467947, -3.899525170167924770 ) ) ;
#26779 = CARTESIAN_POINT ( 'NONE',  ( 0.000000000000000000, -0.5999999999999994227, -3.730072921939604047 ) ) ;
#26781 = CARTESIAN_POINT ( 'NONE',  ( 20.61566240124719229, 6.034574563953731818, -3.423970728030660826 ) ) ;
#26782 = CARTESIAN_POINT ( 'NONE',  ( 74.67253486855700828, 63.25418332940030552, 3.074209570828856819 ) ) ;
#26783 = CARTESIAN_POINT ( 'NONE',  ( 21.84425409567527865, 2.562565029795382809, -5.509240067314594924 ) ) ;
#26784 = CARTESIAN_POINT ( 'NONE',  ( -64.08758708074093136, 36.14363715547679590, 3.800414904976366692 ) ) ;
#26785 = EDGE_CURVE ( 'NONE', #29308, #23344, #35034, .T. ) ;
#26786 = DIRECTION ( 'NONE',  ( 0.5000000000000072164, -0.8660254037844344888, 0.000000000000000000 ) ) ;
#26787 = EDGE_CURVE ( 'NONE', #5350, #6564, #3407, .T. ) ;
#26788 = FACE_OUTER_BOUND ( 'NONE', #27483, .T. ) ;
#26789 = CARTESIAN_POINT ( 'NONE',  ( -1.256819626896593656, -27.89215637338188714, 7.652160403243381204 ) ) ;
#26790 = CARTESIAN_POINT ( 'NONE',  ( -8.348748702180635917, -26.64985754041175525, 6.700000000000000178 ) ) ;
#26791 = CARTESIAN_POINT ( 'NONE',  ( 82.02157412789779301, 62.93630067300351527, 2.502189764415794215 ) ) ;
#26792 = CARTESIAN_POINT ( 'NONE',  ( 85.19528866922426857, 2.662332751101227579, -1.941753459690362726 ) ) ;
#26793 = CARTESIAN_POINT ( 'NONE',  ( 30.63785892209476458, -0.4682215140425676214, 5.751446082446129537 ) ) ;
#26794 = CIRCLE ( 'NONE', #29411, 31.02204673211315011 ) ;
#26795 = CARTESIAN_POINT ( 'NONE',  ( 4.660834209608292866, -31.24198599401081111, 7.721096864323899744 ) ) ;
#26796 = CARTESIAN_POINT ( 'NONE',  ( -79.07517032757485254, -5.439101939624123361, -7.647829796408795566 ) ) ;
#26797 = ORIENTED_EDGE ( 'NONE', *, *, #5966, .T. ) ;
#26798 = CARTESIAN_POINT ( 'NONE',  ( 14.93018881926248120, -5.919497445998742613, 2.519022926048594346 ) ) ;
#26799 = DIRECTION ( 'NONE',  ( -0.4582725098355734938, 0.8888117386314180468, -0.000000000000000000 ) ) ;
#26800 = CARTESIAN_POINT ( 'NONE',  ( 36.66731919220198677, -2.423882815175043337, -5.929219981045500631 ) ) ;
#26801 = CARTESIAN_POINT ( 'NONE',  ( -51.21549048184568420, -30.38627270959228710, 4.000000000000000000 ) ) ;
#26802 = CARTESIAN_POINT ( 'NONE',  ( 6.349790915967283844, -30.58285303640981212, 6.894806418505347700 ) ) ;
#26803 = CARTESIAN_POINT ( 'NONE',  ( -24.34874870218063592, -25.49307895267003587, 6.700000000000000178 ) ) ;
#26804 = DIRECTION ( 'NONE',  ( -0.000000000000000000, -0.000000000000000000, 1.000000000000000000 ) ) ;
#26805 = VERTEX_POINT ( 'NONE', #25597 ) ;
#26806 = CARTESIAN_POINT ( 'NONE',  ( 37.12958521530237022, -2.935469131982732183, 5.998845046471068976 ) ) ;
#26807 = CARTESIAN_POINT ( 'NONE',  ( -69.98383490720681266, -0.4546002296310912572, 5.937231121521810095 ) ) ;
#26808 = CARTESIAN_POINT ( 'NONE',  ( 67.08924564209870312, 58.23032185317626386, -3.992323350375290403 ) ) ;
#26809 = CARTESIAN_POINT ( 'NONE',  ( 3.014835793218893389, -26.32611455060292727, 6.867199677474200570 ) ) ;
#26810 = EDGE_LOOP ( 'NONE', ( #33865, #36427, #8265, #3363, #28806, #12880, #18968, #26772, #17673, #29837, #17071, #34145, #16915, #21849, #32508, #34312, #3217, #19294 ) ) ;
#26811 = B_SPLINE_CURVE_WITH_KNOTS ( 'NONE', 3,
 ( #8225, #27381, #20795, #4564, #20189, #32775 ),
 .UNSPECIFIED., .F., .F.,
 ( 4, 2, 4 ),
 ( 0.000000000000000000, 0.5000000000000000000, 1.000000000000000000 ),
 .UNSPECIFIED. ) ;
#26812 = EDGE_CURVE ( 'NONE', #5710, #30983, #29094, .T. ) ;
#26813 = FACE_OUTER_BOUND ( 'NONE', #3873, .T. ) ;
#26814 = CARTESIAN_POINT ( 'NONE',  ( 86.09291566217842728, 0.07834183196763176704, -5.989438611547945435 ) ) ;
#26815 = CARTESIAN_POINT ( 'NONE',  ( 85.14718662316111875, 1.669408076102861349, -5.191970801932679791 ) ) ;
#26816 = CARTESIAN_POINT ( 'NONE',  ( 5.011198270955363299, -30.34358980514384285, 7.013842709614101167 ) ) ;
#26817 = CARTESIAN_POINT ( 'NONE',  ( 0.3366481700427572665, -32.79331784342181066, 6.906857269533146493 ) ) ;
#26818 = CARTESIAN_POINT ( 'NONE',  ( -28.34874870218063947, -25.49307895267003587, 6.700000000000000178 ) ) ;
#26819 = VERTEX_POINT ( 'NONE', #22326 ) ;
#26820 = CARTESIAN_POINT ( 'NONE',  ( 22.87852314092918604, 4.327528820093371920, 3.073438435473089481 ) ) ;
#26821 = CARTESIAN_POINT ( 'NONE',  ( 80.71579011337402676, 63.33293116964227920, 3.563857694938810106 ) ) ;
#26822 = CARTESIAN_POINT ( 'NONE',  ( -63.45510661405219821, 43.01213780119760344, 3.461531625003003487 ) ) ;
#26823 = VERTEX_POINT ( 'NONE', #6669 ) ;
#26824 = CARTESIAN_POINT ( 'NONE',  ( 79.13122682291697174, 61.20693062157209852, -3.102003663616897278 ) ) ;
#26826 = CARTESIAN_POINT ( 'NONE',  ( 14.78205480818345130, -5.168698993129799746, -2.499999999988669508 ) ) ;
#26825 = CARTESIAN_POINT ( 'NONE',  ( 27.44649324819909353, 0.9063735473286961275, 4.490087085965837943 ) ) ;
#26827 = CARTESIAN_POINT ( 'NONE',  ( 79.22754343384272602, 66.08014515008352419, -1.953285432042054293 ) ) ;
#26828 = CARTESIAN_POINT ( 'NONE',  ( 79.32744125533960755, 63.05206431288016944, 3.774260586041107146 ) ) ;
#26829 = EDGE_CURVE ( 'NONE', #35977, #2740, #20525, .T. ) ;
#26830 = EDGE_CURVE ( 'NONE', #32857, #10365, #28893, .T. ) ;
#26831 = CARTESIAN_POINT ( 'NONE',  ( 36.34168992152566346, -3.603234009378773806, -5.757187825781041823 ) ) ;
#26832 = ADVANCED_FACE ( 'NONE', ( #7663 ), #29687, .F. ) ;
#26833 = CARTESIAN_POINT ( 'NONE',  ( 81.95295003160661906, 61.95651309483399416, 1.189854999565118421 ) ) ;
#26834 = CARTESIAN_POINT ( 'NONE',  ( -20.97867591359219475, -26.64985754041175525, 6.700000000000000178 ) ) ;
#26835 = CARTESIAN_POINT ( 'NONE',  ( 23.91855504425362255, 4.211737807167565961, 0.007810489111244203406 ) ) ;
#26836 = CARTESIAN_POINT ( 'NONE',  ( -62.77932549131168116, 36.45562188509678236, -4.736925958236502865 ) ) ;
#26837 = EDGE_LOOP ( 'NONE', ( #9298, #7795, #21841, #23176 ) ) ;
#26838 = CARTESIAN_POINT ( 'NONE',  ( -80.33671669984387620, -5.680595701363414740, 3.413160419656412259 ) ) ;
#26839 = CARTESIAN_POINT ( 'NONE',  ( 22.29352313805566155, 0.2601191645372996630, -7.110266727710765622 ) ) ;
#26840 = CARTESIAN_POINT ( 'NONE',  ( 25.11437021580303863, 164.7550792202006562, 4.000000000000000000 ) ) ;
#26841 = CARTESIAN_POINT ( 'NONE',  ( 5.175382819553307812, -29.15228733116008186, 6.951256099901594432 ) ) ;
#26842 = ORIENTED_EDGE ( 'NONE', *, *, #36402, .T. ) ;
#26843 = CARTESIAN_POINT ( 'NONE',  ( 33.11223012084407458, -0.1537037112411065998, -4.945624661800740007 ) ) ;
#26844 = LINE ( 'NONE', #20655, #15432 ) ;
#26845 = FACE_OUTER_BOUND ( 'NONE', #30700, .T. ) ;
#26846 = CARTESIAN_POINT ( 'NONE',  ( -1.077356027815240758, -31.69929886267264862, 6.880828092187099010 ) ) ;
#26847 = CARTESIAN_POINT ( 'NONE',  ( -64.08758708074093136, 41.04287353446839148, 3.000000000000000000 ) ) ;
#26848 = DIRECTION ( 'NONE',  ( -1.000000000000000000, 0.000000000000000000, 0.000000000000000000 ) ) ;
#26849 = CARTESIAN_POINT ( 'NONE',  ( 5.093870946763709995, -29.78037735622890736, 6.949473656533221799 ) ) ;
#26850 = AXIS2_PLACEMENT_3D ( 'NONE', #40442, #24612, #36966 ) ;
#26851 = CARTESIAN_POINT ( 'NONE',  ( 1.764561002481344731, -26.07050696156566971, 6.870737987065012931 ) ) ;
#26852 = CARTESIAN_POINT ( 'NONE',  ( 22.24669285715049938, 1.156305209326864425, -6.358976223308567377 ) ) ;
#26853 = VERTEX_POINT ( 'NONE', #36471 ) ;
#26854 = CARTESIAN_POINT ( 'NONE',  ( 66.43484696874301676, 57.75462747860474622, 4.000000000000002665 ) ) ;
#26855 = CARTESIAN_POINT ( 'NONE',  ( 73.82474952339838126, 59.08733682254641195, -3.476886323308218785 ) ) ;
#26856 = ORIENTED_EDGE ( 'NONE', *, *, #27061, .F. ) ;
#26857 = CARTESIAN_POINT ( 'NONE',  ( 85.39947451146549895, 1.536583868559685762, 5.410284084896357371 ) ) ;
#26858 = CLOSED_SHELL ( 'NONE', ( #9063, #18448, #16738, #32611, #17858, #18261, #1701, #6589, #641, #14151, #39791, #9047, #17003, #9528, #18314, #13679, #32447, #27103, #1625, #554, #8285, #34618, #23607, #40383, #39025, #19494, #30255, #23029, #29164, #14120, #25953, #30500, #19310, #779, #35032, #4102, #38722, #18028, #13118, #6203, #10543, #29978, #21759, #857, #34434, #22242, #17504, #38096, #3362, #18965, #39005, #16802, #25261, #9956, #2762, #2399, #10182, #19266, #15867, #38388, #10314, #17695, #6675, #11299, #342, #12648, #13137, #34906, #40160, #35292, #172, #9629, #34075, #25712, #39481, #17795, #12615, #2634, #4031, #5922, #31253, #5223, #682, #23012, #12536, #33492, #7313, #25863, #34259, #17873, #27711, #30844, #17874, #14840, #39312, #24728, #29745, #9254, #18715, #29520, #21379, #16365, #1891, #34764, #8554, #30088, #9960, #5911, #23620, #5454, #40326, #32690, #7620, #4620, #5280, #10087, #23018, #21674, #40340, #21123, #23427, #25142, #36020, #34952, #29823, #1646, #21473, #32953, #13856, #15017, #2927, #23875, #37822, #2066, #13434, #37147, #12114, #2914, #25815, #33767, #37258, #33634, #26735, #33995, #36823, #36573, #30244, #7802, #23080, #32339, #9431, #10349, #25380, #28371, #11537, #38439, #35076, #38017, #16502, #25695, #32840, #5300, #29695, #26269, #8798, #30206, #39936, #26235, #33588, #2981, #33967, #5819, #29012, #19970, #39591, #7806, #34387, #33796, #38262, #19396, #37545, #6789, #33538, #27794, #23577, #31631, #1066, #33638, #6391, #5566, #15179, #39026, #14313, #1546, #17547, #10283, #7441, #37676, #24019, #22885, #31353, #4882, #11408, #7515, #34244, #20395, #30155, #19942, #20348, #39602, #39645, #20711, #27513, #18366, #20488, #33920, #36440, #7863, #26896, #17879, #24260, #24448, #8996, #9909, #19104, #26504, #14497, #1000, #23922, #5028, #20426, #9814, #16150, #33355, #32268, #17580, #15902, #13539, #38002, #17186, #6571, #28840, #20608, #18164, #29056, #14087, #29618, #14537, #9676, #7856, #13439, #9377, #33106, #36585, #32829, #35503, #27275, #12927, #2311, #17397, #14272, #1776, #40566, #39066, #4932, #12881, #31470 ) ) ;
#26859 = DIRECTION ( 'NONE',  ( 0.9396926207859126468, -0.3420201433256568890, -0.000000000000000000 ) ) ;
#26860 = VECTOR ( 'NONE', #35712, 1000.000000000000000 ) ;
#26861 = ORIENTED_EDGE ( 'NONE', *, *, #28244, .F. ) ;
#26862 = CARTESIAN_POINT ( 'NONE',  ( -0.8534657166897973157, -27.17664360927492950, 6.941203072598472801 ) ) ;
#26863 = DIRECTION ( 'NONE',  ( -1.000000000000000000, 0.000000000000000000, 0.000000000000000000 ) ) ;
#26864 = CARTESIAN_POINT ( 'NONE',  ( -20.34874870218063947, -26.64985754041175525, 6.700000000000000178 ) ) ;
#26865 = CARTESIAN_POINT ( 'NONE',  ( 5.051054751933684805, -30.14703185982037681, 7.635761828346577573 ) ) ;
#26866 = ORIENTED_EDGE ( 'NONE', *, *, #36631, .F. ) ;
#26867 = CARTESIAN_POINT ( 'NONE',  ( 80.44079772350292501, 62.04115482339160792, -3.140153738741080058 ) ) ;
#26868 = CARTESIAN_POINT ( 'NONE',  ( 80.44027647058022978, 62.28541378099806280, 3.311815948186458858 ) ) ;
#26870 = EDGE_LOOP ( 'NONE', ( #11646, #40164, #38652, #22670 ) ) ;
#26869 = CARTESIAN_POINT ( 'NONE',  ( 0.5568522185922281098, -26.36799081952789692, 7.779495906702013741 ) ) ;
#26871 = VECTOR ( 'NONE', #6516, 1000.000000000000000 ) ;
#26872 = DIRECTION ( 'NONE',  ( -0.6662082868431843385, 0.000000000000000000, 0.7457657263118689928 ) ) ;
#26873 = EDGE_CURVE ( 'NONE', #24258, #22465, #15318, .T. ) ;
#26874 = CARTESIAN_POINT ( 'NONE',  ( 4.021359916180923477, -27.08534488404830043, 6.887945620086120435 ) ) ;
#26875 = CARTESIAN_POINT ( 'NONE',  ( -28.87867591359218977, -26.64985754041175525, 6.700000000000000178 ) ) ;
#26876 = CARTESIAN_POINT ( 'NONE',  ( 21.85643539959772497, -13.01485165473748573, 3.478087416278500932 ) ) ;
#26877 = FACE_OUTER_BOUND ( 'NONE', #22543, .T. ) ;
#26878 = ORIENTED_EDGE ( 'NONE', *, *, #33802, .F. ) ;
#26879 = CARTESIAN_POINT ( 'NONE',  ( -77.23777935285242791, 9.655128411724760440, 7.769674086704672966 ) ) ;
#26880 = CARTESIAN_POINT ( 'NONE',  ( 14.77590839487426777, -5.162981251534658256, 2.500001664204352547 ) ) ;
#26881 = B_SPLINE_CURVE_WITH_KNOTS ( 'NONE', 3,
 ( #39999, #11769, #24349, #26291, #36913, #11979, #23192, #2559, #15081, #35568, #7336, #19896, #33225, #36706 ),
 .UNSPECIFIED., .F., .F.,
 ( 4, 2, 2, 2, 2, 2, 4 ),
 ( 0.000000000000000000, 0.0003684622442568309176, 0.0005526933663852468372, 0.0006448089274494569383, 0.0006908667079815606878, 0.0007138955982476137552, 0.0007369244885136669310 ),
 .UNSPECIFIED. ) ;
#26882 = CARTESIAN_POINT ( 'NONE',  ( -79.20124688682111014, 10.32858273165098595, -7.499809273847732882 ) ) ;
#26883 = AXIS2_PLACEMENT_3D ( 'NONE', #5767, #24493, #40333 ) ;
#26884 = DIRECTION ( 'NONE',  ( 0.000000000000000000, 0.000000000000000000, 1.000000000000000000 ) ) ;
#26885 = DIRECTION ( 'NONE',  ( 0.000000000000000000, 0.000000000000000000, 1.000000000000000000 ) ) ;
#26886 = CARTESIAN_POINT ( 'NONE',  ( 81.29933375999361544, 61.48586111389077757, 1.777114115212626189 ) ) ;
#26887 = CARTESIAN_POINT ( 'NONE',  ( -1.482088180267139066, -30.76652202637871625, 7.703977250142849620 ) ) ;
#26888 = DIRECTION ( 'NONE',  ( 0.000000000000000000, 0.000000000000000000, -1.000000000000000000 ) ) ;
#26889 = CARTESIAN_POINT ( 'NONE',  ( -0.07765682019414094084, -26.55520811102057621, 7.670465701733746755 ) ) ;
#26890 = CARTESIAN_POINT ( 'NONE',  ( -70.05488178572183244, -0.2788347306335496323, 9.961904852117910991 ) ) ;
#26891 = CARTESIAN_POINT ( 'NONE',  ( -64.52565643081008773, 34.68665887112012314, 5.852036696963947904 ) ) ;
#26892 = CARTESIAN_POINT ( 'NONE',  ( 4.180804271322692500, -31.89534315857266122, 7.013842709614101167 ) ) ;
#26893 = DIRECTION ( 'NONE',  ( 1.000000000000000000, 0.000000000000000000, 0.000000000000000000 ) ) ;
#26894 = CARTESIAN_POINT ( 'NONE',  ( 67.41558015167861129, 58.24452080056473591, 3.997009152755513384 ) ) ;
#26895 = CARTESIAN_POINT ( 'NONE',  ( 36.46939072216235189, -2.309382896708789268, 5.898328456377949003 ) ) ;
#26896 = ADVANCED_FACE ( 'NONE', ( #20214 ), #7862, .F. ) ;
#26897 = AXIS2_PLACEMENT_3D ( 'NONE', #4623, #8495, #11172 ) ;
#26898 = EDGE_LOOP ( 'NONE', ( #15529, #16516, #21648, #2302 ) ) ;
#26899 = LINE ( 'NONE', #2632, #8914 ) ;
#26900 = CARTESIAN_POINT ( 'NONE',  ( 87.85599567641696694, -0.3262996441500809475, -4.386575958041428080 ) ) ;
#26902 = CARTESIAN_POINT ( 'NONE',  ( 33.61667494505991982, -1.223710831992580239, -5.453093166169209915 ) ) ;
#26901 = CARTESIAN_POINT ( 'NONE',  ( 81.19396390929411211, 61.77420168221062369, -2.442092683901112782 ) ) ;
#26903 = CARTESIAN_POINT ( 'NONE',  ( -70.92837670882107659, -31.30579396504363388, -4.357836081054403010 ) ) ;
#26904 = CARTESIAN_POINT ( 'NONE',  ( -58.56870219631061758, 27.89510117891460439, 3.538387446898187072 ) ) ;
#26905 = VERTEX_POINT ( 'NONE', #20817 ) ;
#26906 = CARTESIAN_POINT ( 'NONE',  ( -0.6934048292311358885, -32.12330951052082639, 6.961115707816235343 ) ) ;
#26907 = ORIENTED_EDGE ( 'NONE', *, *, #11639, .F. ) ;
#26908 = CARTESIAN_POINT ( 'NONE',  ( -19.07867591359219972, -26.64985754041175525, 6.800000000000000711 ) ) ;
#26909 = EDGE_CURVE ( 'NONE', #22985, #3507, #28980, .T. ) ;
#26910 = ORIENTED_EDGE ( 'NONE', *, *, #33189, .T. ) ;
#26911 = CARTESIAN_POINT ( 'NONE',  ( 80.98641699598172750, 61.40056178693503597, -2.031354376635674086 ) ) ;
#26912 =( BOUNDED_CURVE ( )  B_SPLINE_CURVE ( 3, ( #10917, #33589, #2289, #14816 ),
 .UNSPECIFIED., .F., .F. ) 
 B_SPLINE_CURVE_WITH_KNOTS ( ( 4, 4 ),
 ( 4.708531083176466403, 4.895802057644187855 ),
 .UNSPECIFIED. ) 
 CURVE ( )  GEOMETRIC_REPRESENTATION_ITEM ( )  RATIONAL_B_SPLINE_CURVE ( ( 1.000000000000000000, 0.9970795998553221295, 0.9970795998553221295, 1.000000000000000000 ) ) 
 REPRESENTATION_ITEM ( '' )  );
#26913 = CARTESIAN_POINT ( 'NONE',  ( -73.45070404594234503, 38.65432087843067421, -8.800414904976364028 ) ) ;
#26914 = CARTESIAN_POINT ( 'NONE',  ( 79.95665241583073168, 64.06168528317471100, 3.692178340560209548 ) ) ;
#26915 = CARTESIAN_POINT ( 'NONE',  ( 25.51906755988597553, 1.283014276674031340, 4.421375708069085420 ) ) ;
#26917 = ORIENTED_EDGE ( 'NONE', *, *, #13587, .F. ) ;
#26916 = CARTESIAN_POINT ( 'NONE',  ( -59.93345510331042902, 24.73247967741478703, -46.17089178453873188 ) ) ;
#26918 = CARTESIAN_POINT ( 'NONE',  ( 76.61572510735733488, 60.58450557137939541, -3.562065002338889119 ) ) ;
#26919 = CARTESIAN_POINT ( 'NONE',  ( -70.31445380653427435, -21.58328887519855854, 5.969244343896258798 ) ) ;
#26920 = ADVANCED_FACE ( 'NONE', ( #13843 ), #7460, .F. ) ;
#26922 = CARTESIAN_POINT ( 'NONE',  ( -3.078675913592197944, -26.64985754041175525, 6.700000000000000178 ) ) ;
#26921 = DIRECTION ( 'NONE',  ( 0.000000000000000000, 0.000000000000000000, -1.000000000000000000 ) ) ;
#26923 = CARTESIAN_POINT ( 'NONE',  ( -1.208261940723883932, -27.80929264776421306, 7.784476445165072533 ) ) ;
#26924 = DIRECTION ( 'NONE',  ( 0.000000000000000000, 0.000000000000000000, 1.000000000000000000 ) ) ;
#26925 = CARTESIAN_POINT ( 'NONE',  ( 4.662690227536057996, -31.23869556963216354, 7.695279973900954751 ) ) ;
#26926 = CARTESIAN_POINT ( 'NONE',  ( 24.26931705048690446, 3.117373144333289936, -3.494565216830213927 ) ) ;
#26927 = ORIENTED_EDGE ( 'NONE', *, *, #12630, .T. ) ;
#26928 = CARTESIAN_POINT ( 'NONE',  ( 9.703489126596460679, 56.50623631086180154, 4.000000000000000000 ) ) ;
#26929 = AXIS2_PLACEMENT_3D ( 'NONE', #7730, #20277, #23770 ) ;
#26930 = CARTESIAN_POINT ( 'NONE',  ( 22.37440129197860728, 3.331413251109061058, -7.657642981191555620 ) ) ;
#26931 = DIRECTION ( 'NONE',  ( -0.000000000000000000, -1.000000000000000000, -0.000000000000000000 ) ) ;
#26932 = CARTESIAN_POINT ( 'NONE',  ( 81.29424054903499552, 63.61798189665044134, 3.316380171285405076 ) ) ;
#26933 = CARTESIAN_POINT ( 'NONE',  ( 85.11033487576473533, 2.122656363318763173, 4.626068480629312418 ) ) ;
#26934 = DIRECTION ( 'NONE',  ( 0.000000000000000000, 0.000000000000000000, -1.000000000000000000 ) ) ;
#26935 = VERTEX_POINT ( 'NONE', #5184 ) ;
#26936 = CARTESIAN_POINT ( 'NONE',  ( -1.624655799086301533, -28.85995144147929992, 7.754798119455333705 ) ) ;
#26937 = CARTESIAN_POINT ( 'NONE',  ( -79.28861043050481783, -5.487522343443236750, 7.393227751528659297 ) ) ;
#26938 = EDGE_CURVE ( 'NONE', #16289, #38679, #35885, .T. ) ;
#26939 = CARTESIAN_POINT ( 'NONE',  ( 21.58863023475808873, 7.202558683720228672, -2.923977588977705544 ) ) ;
#26940 = VECTOR ( 'NONE', #2603, 1000.000000000000000 ) ;
#26941 = CARTESIAN_POINT ( 'NONE',  ( 23.83525155650060867, -3.101377793311910658, -3.828427711158430835 ) ) ;
#26942 = CARTESIAN_POINT ( 'NONE',  ( 33.46291576196824025, -3.080929388775397015, -5.429095326967858348 ) ) ;
#26943 = DIRECTION ( 'NONE',  ( 0.000000000000000000, 0.000000000000000000, 1.000000000000000000 ) ) ;
#26944 = CARTESIAN_POINT ( 'NONE',  ( 24.12374896606528552, 0.5377693420488547371, -5.092152185932238062 ) ) ;
#26945 = DIRECTION ( 'NONE',  ( 1.000000000000000000, 0.000000000000000000, 0.000000000000000000 ) ) ;
#26946 = VERTEX_POINT ( 'NONE', #32991 ) ;
#26947 = FACE_OUTER_BOUND ( 'NONE', #29407, .T. ) ;
#26948 = CARTESIAN_POINT ( 'NONE',  ( -1.142479071211579544, -27.70495301360842078, 7.006423389747789443 ) ) ;
#26949 = ORIENTED_EDGE ( 'NONE', *, *, #4214, .T. ) ;
#26950 = EDGE_LOOP ( 'NONE', ( #6693, #7062, #11855, #34512 ) ) ;
#26951 = CARTESIAN_POINT ( 'NONE',  ( 37.17729982316707549, -2.564139253649980521, 5.980890902488024352 ) ) ;
#26952 = DIRECTION ( 'NONE',  ( -0.6427876096865328126, -0.7660444431189835646, -0.000000000000000000 ) ) ;
#26953 = ADVANCED_FACE ( 'NONE', ( #20412 ), #16917, .T. ) ;
#26954 = ADVANCED_FACE ( 'NONE', ( #8049 ), #18343, .T. ) ;
#26955 = CARTESIAN_POINT ( 'NONE',  ( 20.13561717962239328, -3.050796925077462696, -3.278976415860665572 ) ) ;
#26956 = CARTESIAN_POINT ( 'NONE',  ( -75.45330471031414277, 33.71485196875532608, -9.800414904976365804 ) ) ;
#26957 = ORIENTED_EDGE ( 'NONE', *, *, #5581, .F. ) ;
#26958 = EDGE_CURVE ( 'NONE', #11154, #18734, #26460, .T. ) ;
#26959 = CARTESIAN_POINT ( 'NONE',  ( -8.448748702180639114, -25.49307895267003587, 6.700000000000000178 ) ) ;
#26960 = ORIENTED_EDGE ( 'NONE', *, *, #14347, .F. ) ;
#26961 = ORIENTED_EDGE ( 'NONE', *, *, #40033, .F. ) ;
#26962 = CARTESIAN_POINT ( 'NONE',  ( 4.912497208772558466, -28.45531190136118127, 6.892063359921931642 ) ) ;
#26963 = CYLINDRICAL_SURFACE ( 'NONE', #27464, 0.1000000000000028644 ) ;
#26964 = EDGE_LOOP ( 'NONE', ( #3319, #8525, #22233, #34286 ) ) ;
#26965 = CARTESIAN_POINT ( 'NONE',  ( -58.97431419818038734, 27.59684639285645247, -7.041158924856742551 ) ) ;
#26966 = ORIENTED_EDGE ( 'NONE', *, *, #17621, .T. ) ;
#26968 = CARTESIAN_POINT ( 'NONE',  ( 21.90912465240509732, 3.662607847369724556, 2.128491611106550607 ) ) ;
#26967 = CARTESIAN_POINT ( 'NONE',  ( 4.815108193535243331, -27.97351822038067226, 7.006908160621411419 ) ) ;
#26969 = ORIENTED_EDGE ( 'NONE', *, *, #28721, .T. ) ;
#26970 = CARTESIAN_POINT ( 'NONE',  ( 23.87850738558080366, 3.138038174018865423, 3.674020033097090909 ) ) ;
#26971 = CARTESIAN_POINT ( 'NONE',  ( 81.43190433112079063, 61.44807093728562819, -1.203271478923240601 ) ) ;
#26972 = AXIS2_PLACEMENT_3D ( 'NONE', #28009, #15451, #12368 ) ;
#26973 = DIRECTION ( 'NONE',  ( -1.000000000000000000, 0.000000000000000000, 0.000000000000000000 ) ) ;
#26974 = ORIENTED_EDGE ( 'NONE', *, *, #36581, .T. ) ;
#26976 = CARTESIAN_POINT ( 'NONE',  ( 25.88797439567527903, -2.749903636904698967, -4.246842526108601135 ) ) ;
#26975 = CARTESIAN_POINT ( 'NONE',  ( -34.34874870218063592, -26.64985754041175525, 6.700000000000000178 ) ) ;
#26977 = CARTESIAN_POINT ( 'NONE',  ( -1.794547911424669184, -29.38175913461375188, 6.980586498568969844 ) ) ;
#26978 = CARTESIAN_POINT ( 'NONE',  ( 75.21236926079949114, 60.63031288236823002, 3.833662259905124436 ) ) ;
#26979 = ORIENTED_EDGE ( 'NONE', *, *, #29665, .T. ) ;
#26980 = CARTESIAN_POINT ( 'NONE',  ( 22.46204726948479546, 2.974089873731441624, -4.569747218150055801 ) ) ;
#26981 = PLANE ( 'NONE',  #18828 ) ;
#26982 = CYLINDRICAL_SURFACE ( 'NONE', #20142, 0.09010775117052972905 ) ;
#26983 = DIRECTION ( 'NONE',  ( 0.000000000000000000, 0.000000000000000000, -1.000000000000000000 ) ) ;
#26984 = CARTESIAN_POINT ( 'NONE',  ( -63.05329786184842078, 35.53802554122869850, 6.297540867206088855 ) ) ;
#26985 = CARTESIAN_POINT ( 'NONE',  ( 1.822194502883781375, -26.17211269480022295, 7.754798119455333705 ) ) ;
#26986 = CARTESIAN_POINT ( 'NONE',  ( 79.14825301983928796, 66.20254961713405351, 1.551099981298356134 ) ) ;
#26987 = CARTESIAN_POINT ( 'NONE',  ( 85.88709644997106807, 1.885261416588465799, 4.127327262050844325 ) ) ;
#26988 = CARTESIAN_POINT ( 'NONE',  ( 32.93308485139972674, -2.920656968542761245, -5.757540729513444866 ) ) ;
#26989 = CIRCLE ( 'NONE', #28999, 0.9999999999999998890 ) ;
#26990 = CARTESIAN_POINT ( 'NONE',  ( -76.13539268176610619, -4.086280762280473766, -9.992012468020183391 ) ) ;
#26991 = CARTESIAN_POINT ( 'NONE',  ( 16.27325576391341500, -3.466558749124218686, 2.727822142381055137 ) ) ;
#26992 = CARTESIAN_POINT ( 'NONE',  ( 0.1104740917191936872, -26.45188886312317322, 6.912143950357348743 ) ) ;
#26993 = CARTESIAN_POINT ( 'NONE',  ( 21.35934244005222737, 3.587024235528914584, -3.540039984054675681 ) ) ;
#26994 = DIRECTION ( 'NONE',  ( -0.6427876096865430267, 0.7660444431189749048, -0.000000000000000000 ) ) ;
#26995 = DIRECTION ( 'NONE',  ( -0.000000000000000000, 0.000000000000000000, 1.000000000000000000 ) ) ;
#26996 = DIRECTION ( 'NONE',  ( 0.000000000000000000, 0.000000000000000000, -1.000000000000000000 ) ) ;
#26997 = ADVANCED_FACE ( 'NONE', ( #12157 ), #36971, .T. ) ;
#26998 = CARTESIAN_POINT ( 'NONE',  ( -63.08379346057684245, 18.80112958435945458, -12.49999999999999645 ) ) ;
#26999 = CARTESIAN_POINT ( 'NONE',  ( -22.34874870218063947, -26.64985754041175525, 6.800000000000000711 ) ) ;
#27000 = EDGE_CURVE ( 'NONE', #153, #8362, #13955, .T. ) ;
#27001 = AXIS2_PLACEMENT_3D ( 'NONE', #36323, #20256, #35929 ) ;
#27002 = ORIENTED_EDGE ( 'NONE', *, *, #27188, .F. ) ;
#27003 = CARTESIAN_POINT ( 'NONE',  ( 29.45347667344336884, 1.169340884980286877, 4.331142282593965831 ) ) ;
#27004 = CARTESIAN_POINT ( 'NONE',  ( -70.07498307583588826, -0.2501102476861906676, 5.951446729975970129 ) ) ;
#27005 = CARTESIAN_POINT ( 'NONE',  ( 67.39973655466486946, 58.28774108029888623, -3.995059460290581121 ) ) ;
#27006 = CARTESIAN_POINT ( 'NONE',  ( -71.72747510529796955, -0.1678074918106684243, 9.968450010350146329 ) ) ;
#27007 = ADVANCED_FACE ( 'NONE', ( #6207 ), #18750, .F. ) ;
#27008 = DIRECTION ( 'NONE',  ( 1.000000000000000000, -9.912705577010326536E-16, 0.000000000000000000 ) ) ;
#27009 = EDGE_LOOP ( 'NONE', ( #27589, #3262, #23270, #33169, #22888, #24555, #26778, #24749, #4120 ) ) ;
#27010 = CARTESIAN_POINT ( 'NONE',  ( -0.4574210171174859507, -32.19744825413003753, 7.695279973900954751 ) ) ;
#27011 = CARTESIAN_POINT ( 'NONE',  ( 86.00533037392021640, 0.2452800639758652423, -6.000000104874900764 ) ) ;
#27012 = CARTESIAN_POINT ( 'NONE',  ( 84.97881024039070041, 1.902655756596536518, -4.858038791751294383 ) ) ;
#27013 = CARTESIAN_POINT ( 'NONE',  ( -18.48280404870591553, -63.98126818465317456, 2.500000000000000000 ) ) ;
#27014 = CARTESIAN_POINT ( 'NONE',  ( 0.4108041967164411945, -32.82370865775250479, 6.863654226668487901 ) ) ;
#27015 = CARTESIAN_POINT ( 'NONE',  ( -1.699601713409903292, -29.55877364174393307, 7.775108481317161591 ) ) ;
#27016 = ORIENTED_EDGE ( 'NONE', *, *, #29566, .F. ) ;
#27017 = CARTESIAN_POINT ( 'NONE',  ( 23.14039851168018558, 4.035316712620898194, 3.101781372617715249 ) ) ;
#27018 = CIRCLE ( 'NONE', #10586, 3.778021175560965172 ) ;
#27019 = CARTESIAN_POINT ( 'NONE',  ( 82.34614708994676846, 62.54074552962156019, -1.204231967108631007 ) ) ;
#27020 = CARTESIAN_POINT ( 'NONE',  ( 80.26353224374042838, 64.23390916343181800, 3.625945587094182798 ) ) ;
#27021 = CARTESIAN_POINT ( 'NONE',  ( 1.717829174068238984, -33.06988673718940674, 7.750000000000000888 ) ) ;
#27022 = ORIENTED_EDGE ( 'NONE', *, *, #39351, .F. ) ;
#27023 = CARTESIAN_POINT ( 'NONE',  ( 77.48714025262371763, 64.49898405264993073, -3.102003663616890172 ) ) ;
#27024 = VECTOR ( 'NONE', #1475, 1000.000000000000000 ) ;
#27026 = CARTESIAN_POINT ( 'NONE',  ( 14.77498549067719935, -5.165673680530092682, -2.500001149280607571 ) ) ;
#27025 = CARTESIAN_POINT ( 'NONE',  ( 23.04469232822262725, 0.3231521739056994469, 5.972309192691233726 ) ) ;
#27027 = CARTESIAN_POINT ( 'NONE',  ( 79.79491195508184376, 65.71105728010222435, -2.731335034813057394 ) ) ;
#27028 = CARTESIAN_POINT ( 'NONE',  ( -0.9542785570400912354, -31.86130625091119484, 7.255881584735162981 ) ) ;
#27029 = CARTESIAN_POINT ( 'NONE',  ( 78.38159772055728070, 63.47233311668939848, 3.766285651913923171 ) ) ;
#27030 = ORIENTED_EDGE ( 'NONE', *, *, #36633, .F. ) ;
#27031 = CARTESIAN_POINT ( 'NONE',  ( 34.20739662544301041, -3.854094502681030932, -5.250102797243501485 ) ) ;
#27032 = VECTOR ( 'NONE', #9425, 1000.000000000000000 ) ;
#27033 = CARTESIAN_POINT ( 'NONE',  ( 79.98571111508546494, 66.33520038980110201, 1.398807481800126595 ) ) ;
#27036 = ORIENTED_EDGE ( 'NONE', *, *, #27961, .T. ) ;
#27035 = CYLINDRICAL_SURFACE ( 'NONE', #17608, 0.1000000000000028644 ) ;
#27034 = CARTESIAN_POINT ( 'NONE',  ( 4.339855541068658340, -31.86847383987311133, 6.870737987065013819 ) ) ;
#27037 = CARTESIAN_POINT ( 'NONE',  ( 30.11529565287584020, -4.511537616843412479, 1.859944388213511157 ) ) ;
#27038 = CARTESIAN_POINT ( 'NONE',  ( -1.772272602310306366, -30.00652718025207122, 7.009310105710486738 ) ) ;
#27039 = CARTESIAN_POINT ( 'NONE',  ( -7.890026461918812295, -8.913725925455491250, 6.000000000000000000 ) ) ;
#27040 = ORIENTED_EDGE ( 'NONE', *, *, #11139, .T. ) ;
#27041 = CARTESIAN_POINT ( 'NONE',  ( -81.77390411455343155, -5.606086203577094196, 1.137401704552885251 ) ) ;
#27042 = CARTESIAN_POINT ( 'NONE',  ( 26.06502655271711433, 0.7650683268001282622, -4.421515112517789170 ) ) ;
#27043 = CARTESIAN_POINT ( 'NONE',  ( 4.996814229376580485, -30.74619960369405547, 7.743886751744252450 ) ) ;
#27044 = B_SPLINE_CURVE_WITH_KNOTS ( 'NONE', 3,
 ( #40374, #27624, #17942, #36691, #21257, #39780 ),
 .UNSPECIFIED., .F., .F.,
 ( 4, 2, 4 ),
 ( 0.000000000000000000, 0.5000000000000001110, 1.000000000000000000 ),
 .UNSPECIFIED. ) ;
#27045 = CARTESIAN_POINT ( 'NONE',  ( -1.699609906766908818, -29.56993018339339940, 7.222147233343546802 ) ) ;
#27046 = CYLINDRICAL_SURFACE ( 'NONE', #23570, 7.999999999999986677 ) ;
#27047 = CARTESIAN_POINT ( 'NONE',  ( 27.81486881904474018, 1.842726162330621476, -3.911115716677233678 ) ) ;
#27048 = CARTESIAN_POINT ( 'NONE',  ( 3.405524546634664418, -32.61001036001269426, 7.785096263473211486 ) ) ;
#27049 = PLANE ( 'NONE',  #24222 ) ;
#27050 = DIRECTION ( 'NONE',  ( 0.1736481776669273336, 0.9848077530122085754, -0.000000000000000000 ) ) ;
#27051 =( BOUNDED_CURVE ( )  B_SPLINE_CURVE ( 3, ( #37116, #34679, #31367, #27648 ),
 .UNSPECIFIED., .F., .T. ) 
 B_SPLINE_CURVE_WITH_KNOTS ( ( 4, 4 ),
 ( 1.396263401595463360, 1.534781240595298968 ),
 .UNSPECIFIED. ) 
 CURVE ( )  GEOMETRIC_REPRESENTATION_ITEM ( )  RATIONAL_B_SPLINE_CURVE ( ( 1.000000000000000000, 0.9984017064007810749, 0.9984017064007810749, 1.000000000000000000 ) ) 
 REPRESENTATION_ITEM ( '' )  );
#27052 = CARTESIAN_POINT ( 'NONE',  ( -70.92837670882106238, -48.61702805680358352, 6.000000000000002665 ) ) ;
#27053 = DIRECTION ( 'NONE',  ( 0.7660444431189857850, -0.6427876096865300370, -0.000000000000000000 ) ) ;
#27054 = CARTESIAN_POINT ( 'NONE',  ( 5.097704832850760148, -29.70540078745077039, 6.865312560952604670 ) ) ;
#27055 = CARTESIAN_POINT ( 'NONE',  ( 1.891502090683779613, -26.07515052243017806, 6.971170733404099984 ) ) ;
#27056 = EDGE_LOOP ( 'NONE', ( #27509, #12324, #15671, #9699, #21356, #184 ) ) ;
#27057 = CARTESIAN_POINT ( 'NONE',  ( -70.17127749215180188, -48.42661992061006515, 5.954803573902830216 ) ) ;
#27058 = CARTESIAN_POINT ( 'NONE',  ( 66.42099604079459141, 57.79375748135252877, 4.000000000000015099 ) ) ;
#27059 = CARTESIAN_POINT ( 'NONE',  ( 72.08456622119051360, 59.97905947476213839, -3.962431611483851146 ) ) ;
#27060 = EDGE_CURVE ( 'NONE', #12640, #32941, #8863, .T. ) ;
#27061 = EDGE_CURVE ( 'NONE', #26423, #31406, #35672, .T. ) ;
#27062 = ORIENTED_EDGE ( 'NONE', *, *, #36209, .T. ) ;
#27063 = CARTESIAN_POINT ( 'NONE',  ( 87.78960583812504126, -2.347739977990699778, 2.116702103816012759 ) ) ;
#27064 = AXIS2_PLACEMENT_3D ( 'NONE', #24093, #30092, #11727 ) ;
#27065 = EDGE_CURVE ( 'NONE', #38045, #17923, #5795, .T. ) ;
#27066 = CARTESIAN_POINT ( 'NONE',  ( 6.921324086407803833, -24.55319635012989110, 6.700000000000000178 ) ) ;
#27067 = CARTESIAN_POINT ( 'NONE',  ( 4.890732190868795293, -28.37407357224292070, 7.257242401810564125 ) ) ;
#27068 = CARTESIAN_POINT ( 'NONE',  ( -1.420942960651109033, -28.22185930593809999, 6.997764925645181933 ) ) ;
#27069 = CARTESIAN_POINT ( 'NONE',  ( -0.8579401743431254168, -27.18142544799997751, 6.989977667959442975 ) ) ;
#27070 = PRODUCT_CONTEXT ( 'NONE', #13950, 'mechanical' ) ;
#27071 = DIRECTION ( 'NONE',  ( 0.000000000000000000, 0.6662082868431850047, -0.7457657263118682156 ) ) ;
#27072 = ORIENTED_EDGE ( 'NONE', *, *, #38845, .T. ) ;
#27073 = DIRECTION ( 'NONE',  ( 1.000000000000000000, 0.000000000000000000, 0.000000000000000000 ) ) ;
#27074 = DIRECTION ( 'NONE',  ( -0.000000000000000000, -0.000000000000000000, 1.000000000000000000 ) ) ;
#27075 = ORIENTED_EDGE ( 'NONE', *, *, #39253, .F. ) ;
#27076 = CARTESIAN_POINT ( 'NONE',  ( 79.93741260258519787, 63.33597468792986973, -3.730195463674648604 ) ) ;
#27077 = CARTESIAN_POINT ( 'NONE',  ( 16.91049444498251120, 9.757949283939643337, -2.500000000000007105 ) ) ;
#27078 = CARTESIAN_POINT ( 'NONE',  ( 79.70081467235786477, 66.18075109116946919, -1.965143080302318879 ) ) ;
#27079 = CARTESIAN_POINT ( 'NONE',  ( 80.83613523452670790, 61.24682340193511010, 1.855758959884430181 ) ) ;
#27080 = CARTESIAN_POINT ( 'NONE',  ( -9.741734729663692249, 54.65020406074287251, 4.000000000000000000 ) ) ;
#27081 = CARTESIAN_POINT ( 'NONE',  ( 3.980030838668743520, -27.04736262030031213, 6.863904403958576594 ) ) ;
#27082 = CARTESIAN_POINT ( 'NONE',  ( -80.92837670882107659, 2.429809908903242555, 12.50000000000000000 ) ) ;
#27083 = CARTESIAN_POINT ( 'NONE',  ( 21.85643539959773207, -9.550271554086487313, -10.69920392963802769 ) ) ;
#27084 = ORIENTED_EDGE ( 'NONE', *, *, #37553, .T. ) ;
#27085 = CARTESIAN_POINT ( 'NONE',  ( -79.28028571780328093, 10.39372739289916758, 5.513573824196321027 ) ) ;
#27086 = CARTESIAN_POINT ( 'NONE',  ( 14.78293163467730587, -5.166176174648792419, 2.500000000038486547 ) ) ;
#27087 = CARTESIAN_POINT ( 'NONE',  ( -73.24681673169105522, 4.967639606635550820, -10.91583103658519960 ) ) ;
#27088 = DIRECTION ( 'NONE',  ( 0.9396926207859080948, 0.3420201433256694901, -0.000000000000000000 ) ) ;
#27089 = CARTESIAN_POINT ( 'NONE',  ( 2.496365493979189498, -26.26441612936079295, 6.959317978105167057 ) ) ;
#27090 = CARTESIAN_POINT ( 'NONE',  ( -1.533527784978453878, -30.61958705502705769, 7.757178535559535959 ) ) ;
#27091 = CARTESIAN_POINT ( 'NONE',  ( 3.916367062334308535, -26.99125986761471907, 7.784838882742138644 ) ) ;
#27092 = CARTESIAN_POINT ( 'NONE',  ( -28.34874870218063947, -25.49307895267003587, 6.700000000000000178 ) ) ;
#27093 = CARTESIAN_POINT ( 'NONE',  ( 0.6690963371203834109, -26.22531762158553903, 7.006908160621413195 ) ) ;
#27094 = CARTESIAN_POINT ( 'NONE',  ( -64.36803618090942791, 34.71695719680190706, 5.457112545582705643 ) ) ;
#27095 = CARTESIAN_POINT ( 'NONE',  ( -0.4352988304694859756, -26.92438771328325586, 6.880147297696980857 ) ) ;
#27096 = CARTESIAN_POINT ( 'NONE',  ( -34.97867591359219830, -24.55319635012989110, 6.700000000000000178 ) ) ;
#27097 = ORIENTED_EDGE ( 'NONE', *, *, #1751, .F. ) ;
#27098 = CARTESIAN_POINT ( 'NONE',  ( 68.79143787039059532, 58.12720587843082853, 3.950303728398663949 ) ) ;
#27099 = CARTESIAN_POINT ( 'NONE',  ( 36.42112393931954273, -3.116698823254151041, 5.890795257578658628 ) ) ;
#27100 = ORIENTED_EDGE ( 'NONE', *, *, #20331, .F. ) ;
#27101 = FACE_OUTER_BOUND ( 'NONE', #1915, .T. ) ;
#27102 = CARTESIAN_POINT ( 'NONE',  ( 88.18839210903504977, -0.8832026502337909646, 4.329116466421397469 ) ) ;
#27103 = ADVANCED_FACE ( 'NONE', ( #6002 ), #18539, .F. ) ;
#27105 = CARTESIAN_POINT ( 'NONE',  ( -71.92837670882107659, 28.72470171467712063, 5.916079783099620570 ) ) ;
#27104 = CARTESIAN_POINT ( 'NONE',  ( -71.43230626105646763, -21.65663085445836344, 5.980032331837192849 ) ) ;
#27106 = PLANE ( 'NONE',  #33361 ) ;
#27107 = CARTESIAN_POINT ( 'NONE',  ( -57.13133194381639868, 29.70675091384940814, 4.151468609674973109 ) ) ;
#27108 = CARTESIAN_POINT ( 'NONE',  ( -0.3282911018737336706, -26.83271124052131640, 7.386948897581451234 ) ) ;
#27109 = EDGE_LOOP ( 'NONE', ( #18541, #29255, #32947, #8202 ) ) ;
#27110 = CARTESIAN_POINT ( 'NONE',  ( -71.55887904216392315, -21.56717086459383026, 5.979574859000726939 ) ) ;
#27111 =( REPRESENTATION_RELATIONSHIP ('NONE','NONE', #24012, #29798 ) REPRESENTATION_RELATIONSHIP_WITH_TRANSFORMATION ( #2593 )SHAPE_REPRESENTATION_RELATIONSHIP( ) );
#27112 = CARTESIAN_POINT ( 'NONE',  ( 79.30978077413506355, 65.08723789429433282, -3.243225924683098338 ) ) ;
#27113 = CARTESIAN_POINT ( 'NONE',  ( 3.751251297819363728, -25.49307895267003587, 6.700000000000000178 ) ) ;
#27114 = CARTESIAN_POINT ( 'NONE',  ( 80.93223178899255288, 61.91756539228708789, 2.804471013201325746 ) ) ;
#27115 = CARTESIAN_POINT ( 'NONE',  ( 21.89417189222532301, 0.4921803897989117105, 7.737752117221773140 ) ) ;
#27118 = ORIENTED_EDGE ( 'NONE', *, *, #5073, .T. ) ;
#27117 = CARTESIAN_POINT ( 'NONE',  ( -58.99872204295122913, 28.54795728317057169, 6.891578894883348738 ) ) ;
#27116 = AXIS2_PLACEMENT_3D ( 'NONE', #2594, #27476, #5044 ) ;
#27119 = CARTESIAN_POINT ( 'NONE',  ( -38.97867591359219119, -26.64985754041175525, 6.700000000000000178 ) ) ;
#27120 = CARTESIAN_POINT ( 'NONE',  ( 73.45088770829859470, 61.50831400533110127, -3.795548882783541522 ) ) ;
#27121 = CARTESIAN_POINT ( 'NONE',  ( -70.12836265542944147, -21.39718080098120012, 5.947163767836362247 ) ) ;
#27123 = FACE_OUTER_BOUND ( 'NONE', #13880, .T. ) ;
#27122 = CARTESIAN_POINT ( 'NONE',  ( 87.04213330793392345, 0.5878691963682337596, -6.000000000000000000 ) ) ;
#27124 = CARTESIAN_POINT ( 'NONE',  ( 14.61802081865033642, -4.461995682952384357, -2.500000000000000000 ) ) ;
#27125 = FACE_OUTER_BOUND ( 'NONE', #16202, .T. ) ;
#27126 = EDGE_CURVE ( 'NONE', #30074, #2141, #18533, .T. ) ;
#27127 = CARTESIAN_POINT ( 'NONE',  ( 23.67152737812504526, 3.427402071259508354, -3.470193783917488783 ) ) ;
#27128 = ORIENTED_EDGE ( 'NONE', *, *, #24443, .T. ) ;
#27129 = FACE_OUTER_BOUND ( 'NONE', #34231, .T. ) ;
#27130 = CARTESIAN_POINT ( 'NONE',  ( 22.63837051618441620, -3.414681707391253429, 8.302592004085083133 ) ) ;
#27131 = DIRECTION ( 'NONE',  ( 1.000000000000000000, 0.000000000000000000, 0.000000000000000000 ) ) ;
#27132 = DIRECTION ( 'NONE',  ( -1.000000000000000000, -1.241493069327139093E-16, 0.000000000000000000 ) ) ;
#27133 = CARTESIAN_POINT ( 'NONE',  ( 78.83208086995101382, 66.11806168415743912, 1.392093260605097971 ) ) ;
#27134 = CARTESIAN_POINT ( 'NONE',  ( 87.83080901603209156, -0.9320485544948414747, 4.955211484752597428 ) ) ;
#27135 = CARTESIAN_POINT ( 'NONE',  ( 1.700390093233090871, -29.56993018339339940, 7.800000000000000711 ) ) ;
#27136 = ORIENTED_EDGE ( 'NONE', *, *, #21355, .T. ) ;
#27137 = FACE_OUTER_BOUND ( 'NONE', #30614, .T. ) ;
#27138 = CARTESIAN_POINT ( 'NONE',  ( 1.700390093233090871, -29.56993018339339940, 7.800000000000000711 ) ) ;
#27139 = CARTESIAN_POINT ( 'NONE',  ( 14.92610986758655045, -6.101699263985318922, -2.531194043802452942 ) ) ;
#27140 = CARTESIAN_POINT ( 'NONE',  ( 36.91003892329680980, -2.640456672357779144, -5.967102265281861051 ) ) ;
#27141 = DIRECTION ( 'NONE',  ( 0.000000000000000000, 1.000000000000000000, 0.000000000000000000 ) ) ;
#27142 = CARTESIAN_POINT ( 'NONE',  ( 25.90788401527250429, 0.9445445186425489581, -4.431966072703408699 ) ) ;
#27143 = CARTESIAN_POINT ( 'NONE',  ( 33.46397865298071395, -3.088978469517898340, -5.429261216816389179 ) ) ;
#27144 = ORIENTED_EDGE ( 'NONE', *, *, #5773, .F. ) ;
#27145 = CARTESIAN_POINT ( 'NONE',  ( 34.13642104789413878, -3.131480944053012028, 5.534212115622173300 ) ) ;
#27146 = AXIS2_PLACEMENT_3D ( 'NONE', #37292, #34650, #11956 ) ;
#27147 = CARTESIAN_POINT ( 'NONE',  ( 4.986456615447258933, -28.37449729532158926, 7.767720160662274331 ) ) ;
#27148 = EDGE_CURVE ( 'NONE', #6701, #12553, #3547, .T. ) ;
#27149 = ORIENTED_EDGE ( 'NONE', *, *, #8779, .T. ) ;
#27150 = EDGE_LOOP ( 'NONE', ( #34592, #26910, #22652, #28480, #21974, #7977, #9856, #17068, #20045 ) ) ;
#27151 = CARTESIAN_POINT ( 'NONE',  ( 34.79267513315475924, -3.836925689216892366, 5.375550132972651163 ) ) ;
#27152 =( BOUNDED_CURVE ( )  B_SPLINE_CURVE ( 3, ( #3883, #12911, #13307, #25478 ),
 .UNSPECIFIED., .F., .F. ) 
 B_SPLINE_CURVE_WITH_KNOTS ( ( 4, 4 ),
 ( 4.708531083176467291, 4.895802057644188743 ),
 .UNSPECIFIED. ) 
 CURVE ( )  GEOMETRIC_REPRESENTATION_ITEM ( )  RATIONAL_B_SPLINE_CURVE ( ( 1.000000000000000000, 0.9970795998553221295, 0.9970795998553221295, 1.000000000000000000 ) ) 
 REPRESENTATION_ITEM ( '' )  );
#27153 = CARTESIAN_POINT ( 'NONE',  ( 3.480418331975892343, -32.58348369386324350, 7.678495282201404315 ) ) ;
#27154 = CARTESIAN_POINT ( 'NONE',  ( -0.3487487021806359722, -25.49307895267003587, 6.700000000000000178 ) ) ;
#27155 = EDGE_LOOP ( 'NONE', ( #20244, #13701 ) ) ;
#27156 = CARTESIAN_POINT ( 'NONE',  ( -4.348748702180639469, -25.49307895267003587, 6.800000000000000711 ) ) ;
#27157 = EDGE_LOOP ( 'NONE', ( #10451, #11401, #27538, #5777 ) ) ;
#27159 = ORIENTED_EDGE ( 'NONE', *, *, #38294, .T. ) ;
#27158 = ORIENTED_EDGE ( 'NONE', *, *, #29433, .F. ) ;
#27160 = CYLINDRICAL_SURFACE ( 'NONE', #15442, 0.09010775117053118621 ) ;
#27161 = CARTESIAN_POINT ( 'NONE',  ( 78.64144163184205638, 66.02383098553904972, -1.235082213173780419 ) ) ;
#27162 = CARTESIAN_POINT ( 'NONE',  ( -58.66072975137505807, 29.93711237438063222, -5.396324374907178978 ) ) ;
#27163 = EDGE_LOOP ( 'NONE', ( #11199, #16851, #3915, #18157, #8577 ) ) ;
#27164 = CARTESIAN_POINT ( 'NONE',  ( 4.782688990442776955, -27.91175695004079316, 6.863784140767622333 ) ) ;
#27165 = VERTEX_POINT ( 'NONE', #31528 ) ;
#27166 = CARTESIAN_POINT ( 'NONE',  ( 24.11084648476953873, 3.002081633687809337, 3.727765853929763118 ) ) ;
#27167 = CARTESIAN_POINT ( 'NONE',  ( 80.13359286145576732, 66.18419574793094284, -1.944145319385670589 ) ) ;
#27168 = EDGE_CURVE ( 'NONE', #35794, #11093, #167, .T. ) ;
#27169 = LINE ( 'NONE', #20787, #27867 ) ;
#27171 = CARTESIAN_POINT ( 'NONE',  ( 19.65961218291280233, -2.698309273198196134, -3.274755969297673097 ) ) ;
#27170 = CARTESIAN_POINT ( 'NONE',  ( -0.02740181272327065973, -26.64166531666571558, 7.721096864323898856 ) ) ;
#27172 = DIRECTION ( 'NONE',  ( 1.000000000000000000, 0.000000000000000000, -0.000000000000000000 ) ) ;
#27173 = CARTESIAN_POINT ( 'NONE',  ( 76.92031397606373844, 59.90536750123394683, 2.950589020716061661 ) ) ;
#27174 = AXIS2_PLACEMENT_3D ( 'NONE', #5649, #18186, #31177 ) ;
#27175 = CARTESIAN_POINT ( 'NONE',  ( 23.22712546262786049, 2.410586217767674899, -4.514815941842217129 ) ) ;
#27176 = ORIENTED_EDGE ( 'NONE', *, *, #766, .T. ) ;
#27177 = CYLINDRICAL_SURFACE ( 'NONE', #745, 0.1000000000000028644 ) ;
#27178 = CARTESIAN_POINT ( 'NONE',  ( 17.49770824240842870, -6.259500660934115501, 2.499999999999995115 ) ) ;
#27179 = CARTESIAN_POINT ( 'NONE',  ( 1.731470216958145070, -26.07006818241261215, 6.894806418505347700 ) ) ;
#27180 = CARTESIAN_POINT ( 'NONE',  ( 1.300000000000000044, -0.5999999999999994227, -4.030609108440248889 ) ) ;
#27181 = CARTESIAN_POINT ( 'NONE',  ( 3.729071288339932622, -32.30714912626547886, 7.386948897581449458 ) ) ;
#27182 = CARTESIAN_POINT ( 'NONE',  ( 81.80618415539490229, 63.87961589575515120, 2.903340743335354190 ) ) ;
#27183 = CARTESIAN_POINT ( 'NONE',  ( 85.49511565994269802, 2.325552844478905090, -3.343772400554256397 ) ) ;
#27184 = PLANE ( 'NONE',  #8965 ) ;
#27185 = EDGE_CURVE ( 'NONE', #11338, #31323, #34362, .T. ) ;
#27186 = EDGE_CURVE ( 'NONE', #7892, #17923, #6617, .T. ) ;
#27187 = CARTESIAN_POINT ( 'NONE',  ( -1.510909903798922427, -30.68686900403765705, 6.894806418505348589 ) ) ;
#27188 = EDGE_CURVE ( 'NONE', #18928, #25767, #24269, .T. ) ;
#27189 = CARTESIAN_POINT ( 'NONE',  ( -0.9229550489645098610, -27.40704778601062941, 7.661510568013089717 ) ) ;
#27190 = DIRECTION ( 'NONE',  ( 0.000000000000000000, -0.000000000000000000, -1.000000000000000000 ) ) ;
#27191 = AXIS2_PLACEMENT_3D ( 'NONE', #13250, #18818, #31391 ) ;
#27192 = DIRECTION ( 'NONE',  ( -0.1736481776669174526, -0.9848077530122102408, 0.000000000000000000 ) ) ;
#27193 = CARTESIAN_POINT ( 'NONE',  ( 33.44985200980665496, -3.250795928539166102, -5.427056412495004700 ) ) ;
#27194 = CYLINDRICAL_SURFACE ( 'NONE', #29890, 2.000000000000000000 ) ;
#27195 = DIRECTION ( 'NONE',  ( -0.9396926207859057634, -0.3420201433256757073, -0.000000000000000000 ) ) ;
#27196 = DIRECTION ( 'NONE',  ( 0.000000000000000000, 0.000000000000000000, 1.000000000000000000 ) ) ;
#27197 = FACE_OUTER_BOUND ( 'NONE', #13379, .T. ) ;
#27198 = AXIS2_PLACEMENT_3D ( 'NONE', #34343, #31437, #3057 ) ;
#27199 = CYLINDRICAL_SURFACE ( 'NONE', #34256, 0.1000000000000028644 ) ;
#27200 = EDGE_CURVE ( 'NONE', #28666, #5954, #37673, .T. ) ;
#27201 = ORIENTED_EDGE ( 'NONE', *, *, #38118, .T. ) ;
#27202 = CARTESIAN_POINT ( 'NONE',  ( 35.67313104109378230, -1.412451363119313852, 5.626408984427851756 ) ) ;
#27203 = DIRECTION ( 'NONE',  ( -0.5000000000000036637, 0.8660254037844367092, 0.000000000000000000 ) ) ;
#27204 = CARTESIAN_POINT ( 'NONE',  ( 66.74110339505794798, 57.81860698948682398, -3.998609561963397674 ) ) ;
#27205 = CARTESIAN_POINT ( 'NONE',  ( -72.84815947045233031, 2.429809908903064919, -10.96147798754375202 ) ) ;
#27206 = EDGE_LOOP ( 'NONE', ( #20942, #14748, #24773 ) ) ;
#27207 = DIRECTION ( 'NONE',  ( 1.000000000000000000, 8.398074759113475787E-17, -0.000000000000000000 ) ) ;
#27208 = CARTESIAN_POINT ( 'NONE',  ( 86.00134810727946899, 0.2530519298808260320, -5.999722280616810899 ) ) ;
#27209 = DIRECTION ( 'NONE',  ( -0.8660254037844399289, 0.000000000000000000, -0.4999999999999976685 ) ) ;
#27210 = LINE ( 'NONE', #24324, #24829 ) ;
#27211 = DIRECTION ( 'NONE',  ( 0.000000000000000000, 1.000000000000000000, 0.000000000000000000 ) ) ;
#27212 = CARTESIAN_POINT ( 'NONE',  ( 1.271343038760671451, -26.09632215832020208, 6.998987538705438105 ) ) ;
#27213 = ORIENTED_EDGE ( 'NONE', *, *, #27775, .T. ) ;
#27214 = CARTESIAN_POINT ( 'NONE',  ( 24.72551563480591241, 3.007151916241646017, 3.409849726662557590 ) ) ;
#27215 = CARTESIAN_POINT ( 'NONE',  ( 79.00097698949592484, 66.21430696267364624, -1.000000000000000000 ) ) ;
#27216 = EDGE_CURVE ( 'NONE', #32660, #40343, #19270, .T. ) ;
#27217 = CARTESIAN_POINT ( 'NONE',  ( 79.72815809223409644, 65.03555043453914664, 3.332694751021850976 ) ) ;
#27218 = CARTESIAN_POINT ( 'NONE',  ( -0.1786029313623582471, -32.40354722338927473, 6.949473656533215582 ) ) ;
#27219 = ORIENTED_EDGE ( 'NONE', *, *, #31064, .T. ) ;
#27220 = CARTESIAN_POINT ( 'NONE',  ( 77.20018789615933485, 65.00686241173515612, -2.285396881590235019 ) ) ;
#27222 = CARTESIAN_POINT ( 'NONE',  ( 14.67750890824153487, -4.951417047788147840, -2.499999999999853895 ) ) ;
#27221 = CARTESIAN_POINT ( 'NONE',  ( 23.58969270755171976, 0.4216153867694091839, 5.525703236370836713 ) ) ;
#27223 = CARTESIAN_POINT ( 'NONE',  ( 79.61430779865581542, 65.89704723538382325, -2.499697124808075710 ) ) ;
#27224 = CARTESIAN_POINT ( 'NONE',  ( 78.26672476572065307, 63.69414582742362541, 3.691425412862291644 ) ) ;
#27225 = VECTOR ( 'NONE', #34947, 1000.000000000000000 ) ;
#27226 = CARTESIAN_POINT ( 'NONE',  ( 36.01029390836630029, -3.690187617478303483, -5.670464297519259844 ) ) ;
#27227 = ADVANCED_FACE ( 'NONE', ( #6411 ), #19776, .F. ) ;
#27228 = CARTESIAN_POINT ( 'NONE',  ( 80.67264098608451661, 66.18930038384924330, 1.451695327222104703 ) ) ;
#27231 = ORIENTED_EDGE ( 'NONE', *, *, #15249, .F. ) ;
#27230 = LINE ( 'NONE', #39796, #33444 ) ;
#27229 = CARTESIAN_POINT ( 'NONE',  ( 3.370276098127634068, -26.60826056296400210, 7.712764235869109974 ) ) ;
#27232 = CARTESIAN_POINT ( 'NONE',  ( 26.98641761431236930, 1.293889648236598022, -5.140668381306381818 ) ) ;
#27233 = CARTESIAN_POINT ( 'NONE',  ( -30.97867591359219119, -26.64985754041175525, 6.700000000000000178 ) ) ;
#27234 = ORIENTED_EDGE ( 'NONE', *, *, #23474, .F. ) ;
#27235 = CARTESIAN_POINT ( 'NONE',  ( 1.605929549753502217, -33.06867024173331515, 6.863805608295730387 ) ) ;
#27236 = CARTESIAN_POINT ( 'NONE',  ( 26.74579300571716800, 0.9069395800068310587, -4.382589997453513853 ) ) ;
#27237 = EDGE_CURVE ( 'NONE', #35883, #19738, #15870, .T. ) ;
#27238 = CARTESIAN_POINT ( 'NONE',  ( -4.444218661349752963, -35.94265729135299381, 6.000000000000000000 ) ) ;
#27239 = DIRECTION ( 'NONE',  ( -0.000000000000000000, -1.000000000000000000, -0.000000000000000000 ) ) ;
#27240 = CARTESIAN_POINT ( 'NONE',  ( 5.175340845672220524, -29.15193808794737862, 6.941203072598479018 ) ) ;
#27241 = CARTESIAN_POINT ( 'NONE',  ( 5.149847078580999771, -30.16259136557591702, 7.637894019485641728 ) ) ;
#27242 = CARTESIAN_POINT ( 'NONE',  ( 35.72977957149858241, -1.305545292155645187, -5.539037271891777969 ) ) ;
#27243 = LINE ( 'NONE', #11579, #17378 ) ;
#27244 = CARTESIAN_POINT ( 'NONE',  ( 27.43879703630890887, 0.9604363013853572939, -4.488885905966782275 ) ) ;
#27245 = CARTESIAN_POINT ( 'NONE',  ( 4.995276389714080167, -30.75049260218879965, 7.640616322432101093 ) ) ;
#27246 = PRODUCT_DEFINITION_SHAPE ( 'NONE', 'NONE',  #40721 ) ;
#27247 = CARTESIAN_POINT ( 'NONE',  ( 2.809903756998512137, -32.78380314757816905, 6.887041543973316138 ) ) ;
#27248 = CARTESIAN_POINT ( 'NONE',  ( 5.096413826755827436, -29.73452413738529287, 6.876076431790007604 ) ) ;
#27249 = FACE_OUTER_BOUND ( 'NONE', #8350, .T. ) ;
#27250 = CARTESIAN_POINT ( 'NONE',  ( -10.87867591359219155, -26.64985754041175525, 6.700000000000000178 ) ) ;
#27251 = AXIS2_PLACEMENT_3D ( 'NONE', #6698, #37756, #22354 ) ;
#27252 = CARTESIAN_POINT ( 'NONE',  ( 24.93942215624759484, 2.519938839411334897, -3.978906813874826920 ) ) ;
#27253 = CARTESIAN_POINT ( 'NONE',  ( 66.41802798480563297, 57.80214248194133830, 4.000000000000018652 ) ) ;
#27254 = CARTESIAN_POINT ( 'NONE',  ( 69.87460780774588898, 58.79389746341001199, -3.972683913566375402 ) ) ;
#27255 = VECTOR ( 'NONE', #19570, 1000.000000000000000 ) ;
#27256 = ORIENTED_EDGE ( 'NONE', *, *, #16275, .F. ) ;
#27257 = CARTESIAN_POINT ( 'NONE',  ( -40.24874870218063450, -26.64985754041175525, 6.800000000000000711 ) ) ;
#27258 = CARTESIAN_POINT ( 'NONE',  ( 0.1658859576577136064, -26.53590150653912261, 6.895222827070022653 ) ) ;
#27259 = CARTESIAN_POINT ( 'NONE',  ( 2.911245606938221098, -26.39285055561105153, 6.892063359921934307 ) ) ;
#27260 = DIRECTION ( 'NONE',  ( 0.9396926207859126468, -0.3420201433256568335, -0.000000000000000000 ) ) ;
#27261 = CARTESIAN_POINT ( 'NONE',  ( 2.427704393887406109, -26.14656945195773119, 7.754798119455333705 ) ) ;
#27262 = ORIENTED_EDGE ( 'NONE', *, *, #9010, .T. ) ;
#27263 = CARTESIAN_POINT ( 'NONE',  ( 22.88299028827532666, 4.349279440556175658, 3.031013114583645418 ) ) ;
#27264 = CARTESIAN_POINT ( 'NONE',  ( -52.01549048184568846, -38.28842912540938670, 4.800000000000000711 ) ) ;
#27265 = EDGE_CURVE ( 'NONE', #39495, #35525, #6743, .T. ) ;
#27266 = ORIENTED_EDGE ( 'NONE', *, *, #5038, .F. ) ;
#27267 = CARTESIAN_POINT ( 'NONE',  ( 78.59965762292412705, 65.58148208812491475, -2.436540443961504820 ) ) ;
#27268 = CARTESIAN_POINT ( 'NONE',  ( 18.79220261045992046, 6.725182846677081550, -3.484773916742352817 ) ) ;
#27269 = CARTESIAN_POINT ( 'NONE',  ( 81.88543442889042012, 63.19940289366422803, -2.771525467262165421 ) ) ;
#27270 = CARTESIAN_POINT ( 'NONE',  ( 78.50817655541952433, 65.71198414996337078, 2.174061886842030944 ) ) ;
#27271 = EDGE_CURVE ( 'NONE', #15871, #23038, #32707, .T. ) ;
#27272 = AXIS2_PLACEMENT_3D ( 'NONE', #3193, #12816, #12207 ) ;
#27273 = VECTOR ( 'NONE', #31265, 1000.000000000000000 ) ;
#27274 = CARTESIAN_POINT ( 'NONE',  ( -30.34874870218063947, -25.49307895267003587, 6.700000000000000178 ) ) ;
#27275 = ADVANCED_FACE ( 'NONE', ( #3749 ), #22274, .F. ) ;
#27276 = CARTESIAN_POINT ( 'NONE',  ( -64.08758708074091714, 24.84364830758654108, -3.800414904976364028 ) ) ;
#27277 = CARTESIAN_POINT ( 'NONE',  ( 2.277491769660097365, -26.21926552469281191, 7.635761828346577573 ) ) ;
#27278 = CARTESIAN_POINT ( 'NONE',  ( 21.85643539959778181, 11.38078789530947788, 4.862784767728865809 ) ) ;
#27279 = ORIENTED_EDGE ( 'NONE', *, *, #4709, .F. ) ;
#27280 = DIRECTION ( 'NONE',  ( -1.000000000000000000, 0.000000000000000000, 0.000000000000000000 ) ) ;
#27281 = EDGE_CURVE ( 'NONE', #5311, #12672, #23167, .T. ) ;
#27282 = VECTOR ( 'NONE', #32655, 1000.000000000000000 ) ;
#27283 = CARTESIAN_POINT ( 'NONE',  ( 14.77222812468941449, -4.461849342347315783, 2.511961485181791520 ) ) ;
#27284 = EDGE_CURVE ( 'NONE', #1864, #7, #38898, .T. ) ;
#27285 = CARTESIAN_POINT ( 'NONE',  ( -74.09550586375644343, 6.760974547859217587, -10.75457049036731938 ) ) ;
#27286 = CARTESIAN_POINT ( 'NONE',  ( 1.575559142037938454, -32.96765387319566543, 6.863904403958575706 ) ) ;
#27287 = CARTESIAN_POINT ( 'NONE',  ( 2.443030458780631076, -26.25201205342539268, 6.871394612369935651 ) ) ;
#27288 = CARTESIAN_POINT ( 'NONE',  ( -1.743365991543899485, -30.19486540288534826, 7.750000000000001776 ) ) ;
#27289 = CARTESIAN_POINT ( 'NONE',  ( 14.71123721502443082, 12.78438965696137863, 2.502442378657849353 ) ) ;
#27290 = CARTESIAN_POINT ( 'NONE',  ( -0.8885437841551658833, -31.78482907790084511, 7.257242401810562349 ) ) ;
#27291 = CARTESIAN_POINT ( 'NONE',  ( 0.6575462507011821112, -26.22889365144838791, 6.887547729233689076 ) ) ;
#27292 = PLANE ( 'NONE',  #30236 ) ;
#27293 = CARTESIAN_POINT ( 'NONE',  ( 4.851634552394991751, -30.84651091276440482, 7.754798119455333705 ) ) ;
#27294 = CARTESIAN_POINT ( 'NONE',  ( -88.78960668556791802, 4.298224710795182091, 12.50000000000000000 ) ) ;
#27295 = DIRECTION ( 'NONE',  ( -1.000000000000000000, 0.000000000000000000, 0.000000000000000000 ) ) ;
#27296 = ORIENTED_EDGE ( 'NONE', *, *, #24774, .F. ) ;
#27297 = CARTESIAN_POINT ( 'NONE',  ( 67.88769211468458309, 58.75904380331535037, 3.964697573200772762 ) ) ;
#27298 = CARTESIAN_POINT ( 'NONE',  ( 31.72026365724324393, -0.5546405064503883153, 5.157112319825081670 ) ) ;
#27299 = ORIENTED_EDGE ( 'NONE', *, *, #12683, .F. ) ;
#27300 = VECTOR ( 'NONE', #27141, 1000.000000000000000 ) ;
#27301 = LINE ( 'NONE', #5695, #38474 ) ;
#27302 = VECTOR ( 'NONE', #30002, 1000.000000000000000 ) ;
#27303 = CARTESIAN_POINT ( 'NONE',  ( 87.06807637922989329, 0.009568187950425697044, -5.830412620327568796 ) ) ;
#27305 = CARTESIAN_POINT ( 'NONE',  ( 4.835314087903390678, -30.88610643146232704, 6.876076431790003163 ) ) ;
#27304 = CARTESIAN_POINT ( 'NONE',  ( 8.290806648384990041, 0.000000000000000000, 2.500000000000000000 ) ) ;
#27306 = CARTESIAN_POINT ( 'NONE',  ( -1.630517953187181401, -28.88791274465361525, 6.866852738645442322 ) ) ;
#27307 = FACE_OUTER_BOUND ( 'NONE', #28990, .T. ) ;
#27308 = VECTOR ( 'NONE', #8351, 1000.000000000000000 ) ;
#27309 = CARTESIAN_POINT ( 'NONE',  ( -70.05507390326904726, -21.28749960934529639, 5.936322957303396208 ) ) ;
#27310 = VERTEX_POINT ( 'NONE', #30249 ) ;
#27311 = CARTESIAN_POINT ( 'NONE',  ( -17.69482985384421880, -42.37473357531882101, 6.000000000000000000 ) ) ;
#27312 = EDGE_LOOP ( 'NONE', ( #24791, #1021 ) ) ;
#27313 = CARTESIAN_POINT ( 'NONE',  ( 78.55684871931622126, 65.96378271911972035, -1.386845825021860490 ) ) ;
#27314 = LINE ( 'NONE', #26913, #11508 ) ;
#27315 = PRODUCT_DEFINITION ( 'UNKNOWN', '', #36025, #2845 ) ;
#27316 = CARTESIAN_POINT ( 'NONE',  ( 79.53095237740791390, 64.90064992126237087, 3.392181771880189434 ) ) ;
#27317 = CARTESIAN_POINT ( 'NONE',  ( 23.13594544608132964, 0.4166732799763251949, 5.866887071280732613 ) ) ;
#27319 = ORIENTED_EDGE ( 'NONE', *, *, #11270, .T. ) ;
#27318 = CARTESIAN_POINT ( 'NONE',  ( -0.7716361497966220950, -27.23559914909565904, 6.997764925645183709 ) ) ;
#27320 = CARTESIAN_POINT ( 'NONE',  ( 74.19779514372055473, 59.81543539827580958, -3.749455561448977736 ) ) ;
#27321 = CARTESIAN_POINT ( 'NONE',  ( 3.218352612218526421, -32.61226313541482114, 6.929923840112066635 ) ) ;
#27323 = CARTESIAN_POINT ( 'NONE',  ( -0.9606818258635283492, -27.29645349747919170, 6.894806418505347700 ) ) ;
#27322 = CARTESIAN_POINT ( 'NONE',  ( 66.41194937274630661, -13.65448019739280028, -6.000000000000000000 ) ) ;
#27324 = DIRECTION ( 'NONE',  ( -1.000000000000000000, 0.000000000000000000, 0.000000000000000000 ) ) ;
#27325 = FACE_OUTER_BOUND ( 'NONE', #28492, .T. ) ;
#27326 = CARTESIAN_POINT ( 'NONE',  ( -2.466074105205459333, -31.90971050668977327, 7.013842709614101167 ) ) ;
#27327 = CARTESIAN_POINT ( 'NONE',  ( 22.41749760006145209, 4.809556558396148596, -3.145958556896370606 ) ) ;
#27328 = ORIENTED_EDGE ( 'NONE', *, *, #17278, .F. ) ;
#27329 = DIRECTION ( 'NONE',  ( 1.000000000000000000, 0.000000000000000000, -0.000000000000000000 ) ) ;
#27330 = EDGE_CURVE ( 'NONE', #1874, #30074, #4543, .T. ) ;
#27331 = VECTOR ( 'NONE', #13133, 1000.000000000000000 ) ;
#27332 = CARTESIAN_POINT ( 'NONE',  ( 25.51676067120702740, -4.685157242005201006, -0.9133679171623337867 ) ) ;
#27333 = CIRCLE ( 'NONE', #17434, 3.499999999999999556 ) ;
#27334 = EDGE_CURVE ( 'NONE', #32411, #24028, #28601, .T. ) ;
#27335 = CARTESIAN_POINT ( 'NONE',  ( 3.273005465665050906, -32.70437678528606540, 7.387053503561888057 ) ) ;
#27336 = CARTESIAN_POINT ( 'NONE',  ( 1.036786817713226450, -32.99129474682166574, 7.785593909369612931 ) ) ;
#27337 = CARTESIAN_POINT ( 'NONE',  ( 81.53866496494931937, 61.91358381440762315, 2.246767365023751406 ) ) ;
#27338 = CARTESIAN_POINT ( 'NONE',  ( 85.61743365444765175, 1.218782235343771836, 5.694237175320765232 ) ) ;
#27339 = CARTESIAN_POINT ( 'NONE',  ( -17.27251170661583402, 3.729367930467589076, 2.500000000000000000 ) ) ;
#27340 = ORIENTED_EDGE ( 'NONE', *, *, #6152, .F. ) ;
#27341 = CARTESIAN_POINT ( 'NONE',  ( -0.01048567703486024197, -32.63106951773389852, 7.255881584735165646 ) ) ;
#27342 = VECTOR ( 'NONE', #6029, 1000.000000000000000 ) ;
#27343 = ORIENTED_EDGE ( 'NONE', *, *, #18609, .F. ) ;
#27344 = CARTESIAN_POINT ( 'NONE',  ( 5.057249517591178467, -29.03002200468333527, 6.892063359921931642 ) ) ;
#27345 = CARTESIAN_POINT ( 'NONE',  ( 16.06814633003477510, -3.505435886482454411, -2.701413578244389324 ) ) ;
#27346 = CARTESIAN_POINT ( 'NONE',  ( -64.36865852185155745, 34.97220226750604866, -7.506047544094577084 ) ) ;
#27347 = CARTESIAN_POINT ( 'NONE',  ( -4.448748702180642667, -25.49307895267003587, 6.700000000000000178 ) ) ;
#27348 = CARTESIAN_POINT ( 'NONE',  ( -62.81463675898083210, 36.67811266762162603, 4.600311178732273021 ) ) ;
#27349 = EDGE_LOOP ( 'NONE', ( #40220, #24181, #37547, #11248 ) ) ;
#27350 = CARTESIAN_POINT ( 'NONE',  ( 2.798682367290367345, -32.88823465369409860, 7.771081512783694301 ) ) ;
#27351 = FACE_OUTER_BOUND ( 'NONE', #17421, .T. ) ;
#27352 = CARTESIAN_POINT ( 'NONE',  ( 87.93559242015480493, -0.4157064846058496355, 3.292354338654781998 ) ) ;
#27353 = ORIENTED_EDGE ( 'NONE', *, *, #14302, .T. ) ;
#27354 = ORIENTED_EDGE ( 'NONE', *, *, #14385, .T. ) ;
#27356 = CARTESIAN_POINT ( 'NONE',  ( 30.88427062897021713, 0.7007091440377163361, 4.489139483277927667 ) ) ;
#27355 = CARTESIAN_POINT ( 'NONE',  ( 81.28781607649123941, 61.48165154268892252, -1.786209778413326621 ) ) ;
#27357 = CARTESIAN_POINT ( 'NONE',  ( 20.92499718081190352, -2.659581275971057757, 3.472249901671649042 ) ) ;
#27358 = CARTESIAN_POINT ( 'NONE',  ( 17.83173683073222549, -3.184001612988465624, -2.948685647352225825 ) ) ;
#27359 = CARTESIAN_POINT ( 'NONE',  ( -45.33131703149249603, -29.56993018339339940, 6.800000000000000711 ) ) ;
#27360 = ORIENTED_EDGE ( 'NONE', *, *, #3388, .F. ) ;
#27361 = FACE_OUTER_BOUND ( 'NONE', #36299, .T. ) ;
#27362 = ORIENTED_EDGE ( 'NONE', *, *, #14827, .F. ) ;
#27363 = ORIENTED_EDGE ( 'NONE', *, *, #17175, .F. ) ;
#27364 = CARTESIAN_POINT ( 'NONE',  ( 0.6783104270758654186, -48.60743831809499227, 2.500000000000000000 ) ) ;
#27365 = CARTESIAN_POINT ( 'NONE',  ( 80.68955802291256418, 62.97990070207239199, -3.482375488376182382 ) ) ;
#27366 = MECHANICAL_DESIGN_GEOMETRIC_PRESENTATION_REPRESENTATION (  '', ( #2423 ), #26159 ) ;
#27367 = CARTESIAN_POINT ( 'NONE',  ( -59.61240458878659609, 26.78407864000503835, -6.268956829791695995 ) ) ;
#27368 = VERTEX_POINT ( 'NONE', #10492 ) ;
#27369 = CARTESIAN_POINT ( 'NONE',  ( 22.86800780692831481, 3.053438318512094352, 4.223698497200296664 ) ) ;
#27370 = VECTOR ( 'NONE', #6840, 1000.000000000000000 ) ;
#27371 = CARTESIAN_POINT ( 'NONE',  ( 82.15073535245149117, 63.33429545135105343, -2.460680857249039732 ) ) ;
#27372 = CARTESIAN_POINT ( 'NONE',  ( -19.07867591359219972, -24.55319635012989110, 6.700000000000000178 ) ) ;
#27373 = VERTEX_POINT ( 'NONE', #5134 ) ;
#27374 = B_SPLINE_CURVE_WITH_KNOTS ( 'NONE', 3,
 ( #9501, #37906, #3372, #2750, #34862, #15686, #3171, #37098, #40377, #28237 ),
 .UNSPECIFIED., .F., .F.,
 ( 4, 3, 3, 4 ),
 ( 0.0002170292169044764612, 0.0002420761345915976642, 0.0002723302478207013412, 0.0002816811360866761506 ),
 .UNSPECIFIED. ) ;
#27376 = CARTESIAN_POINT ( 'NONE',  ( 26.16633878416043757, -2.761556949326915866, -4.290288021199886614 ) ) ;
#27375 = CARTESIAN_POINT ( 'NONE',  ( 0.1051159217697939657, -26.56741378726063019, 7.757178535559535959 ) ) ;
#27377 = CARTESIAN_POINT ( 'NONE',  ( -1.795830882100833747, -29.40718105334054044, 6.887547729233689964 ) ) ;
#27378 = CARTESIAN_POINT ( 'NONE',  ( 73.98866219012947454, 61.81968298976576648, 3.762445401688966573 ) ) ;
#27379 = CARTESIAN_POINT ( 'NONE',  ( 22.63225339419747328, 3.325388178310765941, -4.169375494914318914 ) ) ;
#27380 = CARTESIAN_POINT ( 'NONE',  ( 4.595043951338862342, -27.59037241275625263, 7.501983001166816933 ) ) ;
#27381 = CARTESIAN_POINT ( 'NONE',  ( 16.13270506554978923, 15.26110145415460195, 1.497002735631780768 ) ) ;
#27383 = EDGE_CURVE ( 'NONE', #33469, #6532, #13591, .T. ) ;
#27382 = CARTESIAN_POINT ( 'NONE',  ( -16.24874870218063450, -26.64985754041175525, 6.800000000000000711 ) ) ;
#27384 = ORIENTED_EDGE ( 'NONE', *, *, #15147, .F. ) ;
#27385 = CARTESIAN_POINT ( 'NONE',  ( -1.650274565467498622, -28.99282850696639713, 7.635761828346577573 ) ) ;
#27386 = CARTESIAN_POINT ( 'NONE',  ( 80.77640933968173442, 65.62578451531319956, 2.636331425444717436 ) ) ;
#27387 = CARTESIAN_POINT ( 'NONE',  ( 87.11756278340992310, 0.5031432294147388795, -4.836983121871330837 ) ) ;
#27388 = CARTESIAN_POINT ( 'NONE',  ( 29.20166386951125048, 2.268204792580242213, 0.006282727923920283265 ) ) ;
#27389 = CARTESIAN_POINT ( 'NONE',  ( 3.554700302571109916, -26.60177950712765593, 7.754798119455333705 ) ) ;
#27390 = EDGE_LOOP ( 'NONE', ( #27817, #3366, #22617, #26038 ) ) ;
#27391 = CARTESIAN_POINT ( 'NONE',  ( 15.00253043624129212, -6.083877922989610276, 2.528644475646949275 ) ) ;
#27392 = CARTESIAN_POINT ( 'NONE',  ( 1.057242960569752199, -26.12952878737186424, 7.695279973900954751 ) ) ;
#27393 = CARTESIAN_POINT ( 'NONE',  ( 35.78605622417325804, -3.164553250030355258, -5.791677581459363289 ) ) ;
#27394 = CARTESIAN_POINT ( 'NONE',  ( 4.640282458258592868, -31.46914920237587410, 7.006908160621408754 ) ) ;
#27395 =( BOUNDED_CURVE ( )  B_SPLINE_CURVE ( 3, ( #19435, #15931, #25612, #108 ),
 .UNSPECIFIED., .F., .F. ) 
 B_SPLINE_CURVE_WITH_KNOTS ( ( 4, 4 ),
 ( 4.748221474220560623, 4.941946782021394924 ),
 .UNSPECIFIED. ) 
 CURVE ( )  GEOMETRIC_REPRESENTATION_ITEM ( )  RATIONAL_B_SPLINE_CURVE ( ( 1.000000000000000000, 0.9968749865767494445, 0.9968749865767494445, 1.000000000000000000 ) ) 
 REPRESENTATION_ITEM ( '' )  );
#27396 = AXIS2_PLACEMENT_3D ( 'NONE', #9227, #38246, #6365 ) ;
#27397 = DIRECTION ( 'NONE',  ( 0.000000000000000000, 0.000000000000000000, 1.000000000000000000 ) ) ;
#27398 = AXIS2_PLACEMENT_3D ( 'NONE', #26292, #3884, #32278 ) ;
#27399 = AXIS2_PLACEMENT_3D ( 'NONE', #24044, #11479, #30442 ) ;
#27400 = CARTESIAN_POINT ( 'NONE',  ( 0.05821587971655942800, -26.47918129880799043, 7.753200566781599079 ) ) ;
#27401 = CARTESIAN_POINT ( 'NONE',  ( 1.734342869981767121, -33.06976549508323160, 7.714178352335856026 ) ) ;
#27402 = EDGE_LOOP ( 'NONE', ( #28771, #6380, #35598, #6703 ) ) ;
#27403 = CARTESIAN_POINT ( 'NONE',  ( 36.20067509515345705, -3.648475481699166689, 5.719151051457621371 ) ) ;
#27404 = CARTESIAN_POINT ( 'NONE',  ( -71.92837670882107659, -0.7434385580723641418, 5.928123921495646265 ) ) ;
#27405 = EDGE_CURVE ( 'NONE', #20092, #28513, #29117, .T. ) ;
#27406 = CARTESIAN_POINT ( 'NONE',  ( 66.96854123855969476, 58.10689591609776983, -3.996990690923976519 ) ) ;
#27407 = CARTESIAN_POINT ( 'NONE',  ( -60.14275962559869981, 24.84364830758654108, 9.154021781743367114 ) ) ;
#27408 = ORIENTED_EDGE ( 'NONE', *, *, #25074, .F. ) ;
#27409 = CARTESIAN_POINT ( 'NONE',  ( -83.92837670882109080, 2.429809908903242555, 12.50000000000000000 ) ) ;
#27410 = CARTESIAN_POINT ( 'NONE',  ( -71.75878675104897297, 2.184363218556831132, -9.965500343853747722 ) ) ;
#27411 = CARTESIAN_POINT ( 'NONE',  ( 17.27299901063489074, 8.731752785486881052, 2.902267263306012701 ) ) ;
#27412 = CARTESIAN_POINT ( 'NONE',  ( 25.11437021580303863, 164.7550792202006562, 4.000000000000000000 ) ) ;
#27413 = EDGE_CURVE ( 'NONE', #4341, #13546, #35969, .T. ) ;
#27414 = CARTESIAN_POINT ( 'NONE',  ( -30.44874870218064089, -25.49307895267003587, 6.700000000000000178 ) ) ;
#27415 = CARTESIAN_POINT ( 'NONE',  ( -63.08758708074093136, 41.04287353446839859, -3.000000000000000000 ) ) ;
#27416 = ORIENTED_EDGE ( 'NONE', *, *, #24551, .T. ) ;
#27417 = CARTESIAN_POINT ( 'NONE',  ( 21.85364604960087220, 5.828349873347765886, 3.192828959171670533 ) ) ;
#27418 = CARTESIAN_POINT ( 'NONE',  ( 79.34209122208885390, 66.30884595491197331, -1.045691535380374182 ) ) ;
#27419 = CARTESIAN_POINT ( 'NONE',  ( 14.77500745536057813, -5.175466302041957789, 2.500000552286355759 ) ) ;
#27420 = EDGE_CURVE ( 'NONE', #23344, #7366, #7373, .T. ) ;
#27421 = CARTESIAN_POINT ( 'NONE',  ( 80.11713744326790732, 64.15277314745162585, 3.661914029440277218 ) ) ;
#27422 = AXIS2_PLACEMENT_3D ( 'NONE', #36577, #17616, #20929 ) ;
#27423 = DIRECTION ( 'NONE',  ( -0.000000000000000000, -0.000000000000000000, -1.000000000000000000 ) ) ;
#27424 = ORIENTED_EDGE ( 'NONE', *, *, #37090, .F. ) ;
#27425 = CARTESIAN_POINT ( 'NONE',  ( 78.58187568275401702, 60.86241699943117567, -3.054665556626412926 ) ) ;
#27426 = B_SPLINE_CURVE_WITH_KNOTS ( 'NONE', 3,
 ( #5950, #14384, #22225, #28591, #9849, #37627, #25304, #12320, #6158, #19118, #3704, #31685, #22627, #602, #22424, #31078 ),
 .UNSPECIFIED., .F., .F.,
 ( 4, 2, 2, 2, 2, 2, 2, 4 ),
 ( 0.002348712775360395008, 0.002642162077394872178, 0.002935611379429349348, 0.003522509983498256850, 0.003815959285532717973, 0.004109408587567179097, 0.004402857889601640221, 0.004696307191636101344 ),
 .UNSPECIFIED. ) ;
#27428 = CARTESIAN_POINT ( 'NONE',  ( 14.78228770234103351, -5.167964840227161183, -2.500001186442457168 ) ) ;
#27427 = CARTESIAN_POINT ( 'NONE',  ( 26.76647894427393837, 0.8302801056813566838, 4.383954407630289651 ) ) ;
#27429 =( GEOMETRIC_REPRESENTATION_CONTEXT ( 3 ) GLOBAL_UNCERTAINTY_ASSIGNED_CONTEXT ( ( #8569 ) ) GLOBAL_UNIT_ASSIGNED_CONTEXT ( ( #1067, #13093, #35148 ) ) REPRESENTATION_CONTEXT ( 'NONE', 'WORKASPACE' ) );
#27430 = CARTESIAN_POINT ( 'NONE',  ( 81.15786166771449928, 61.29969053694480152, -1.104694797982636256 ) ) ;
#27431 = CARTESIAN_POINT ( 'NONE',  ( 80.24754081275330009, 61.06584331557482415, 2.177161688561031649 ) ) ;
#27432 = VECTOR ( 'NONE', #6242, 1000.000000000000000 ) ;
#27433 = EDGE_LOOP ( 'NONE', ( #25444, #34409, #30459, #4998, #7414, #27363, #19123, #39321 ) ) ;
#27434 = ORIENTED_EDGE ( 'NONE', *, *, #33054, .T. ) ;
#27435 = AXIS2_PLACEMENT_3D ( 'NONE', #22779, #7513, #16567 ) ;
#27436 = CARTESIAN_POINT ( 'NONE',  ( -0.9023186554178064256, -27.38225855133887876, 7.769368695748482878 ) ) ;
#27437 = ADVANCED_FACE ( 'NONE', ( #21805 ), #2065, .T. ) ;
#27438 = CARTESIAN_POINT ( 'NONE',  ( 82.42900007550694852, 62.86339166853763061, 1.342843868341103697 ) ) ;
#27441 = ORIENTED_EDGE ( 'NONE', *, *, #36581, .F. ) ;
#27440 = PLANE ( 'NONE',  #5143 ) ;
#27439 = CARTESIAN_POINT ( 'NONE',  ( 4.357018571862512069, -31.84860785277257733, 6.887161170156905321 ) ) ;
#27442 = CARTESIAN_POINT ( 'NONE',  ( 27.87477497239535396, 2.606304449749688779, 1.085873857364543671 ) ) ;
#27443 = CARTESIAN_POINT ( 'NONE',  ( -1.771850874358142480, -30.00986502286520974, 6.895394898881670009 ) ) ;
#27444 = DIRECTION ( 'NONE',  ( -0.000000000000000000, -0.000000000000000000, -1.000000000000000000 ) ) ;
#27445 = FACE_OUTER_BOUND ( 'NONE', #12772, .T. ) ;
#27446 = CARTESIAN_POINT ( 'NONE',  ( 23.07038014192270126, 0.3568886247812357304, -5.941770054002118329 ) ) ;
#27447 = DIRECTION ( 'NONE',  ( -0.000000000000000000, -0.000000000000000000, 1.000000000000000000 ) ) ;
#27448 = CARTESIAN_POINT ( 'NONE',  ( 4.999117453304829262, -30.73971554999452493, 7.730015791551950066 ) ) ;
#27449 = CARTESIAN_POINT ( 'NONE',  ( 5.166839686415635846, -29.08636573508110246, 6.867199677474203234 ) ) ;
#27450 = CARTESIAN_POINT ( 'NONE',  ( -1.799609906766908685, -29.55956997194928704, 6.917973428066297004 ) ) ;
#27451 = CARTESIAN_POINT ( 'NONE',  ( 36.13184693646208956, -1.532129719049094119, -5.644433108115570974 ) ) ;
#27452 = CARTESIAN_POINT ( 'NONE',  ( 3.420591031575084262, -32.60521468080220586, 7.781480525794718162 ) ) ;
#27453 = CARTESIAN_POINT ( 'NONE',  ( 27.35387344454971270, 1.116497774337839477, -4.475331455587648222 ) ) ;
#27454 = DIRECTION ( 'NONE',  ( -0.000000000000000000, -0.000000000000000000, -1.000000000000000000 ) ) ;
#27455 = CARTESIAN_POINT ( 'NONE',  ( 0.4447534508558593225, -32.82201345496964251, 7.784725160561910329 ) ) ;
#27456 = DIRECTION ( 'NONE',  ( -0.000000000000000000, -0.000000000000000000, -1.000000000000000000 ) ) ;
#27457 = CARTESIAN_POINT ( 'NONE',  ( -72.84815947045163398, 2.833900941398741047, 10.96147798754381064 ) ) ;
#27458 = EDGE_CURVE ( 'NONE', #12570, #23904, #10435, .T. ) ;
#27459 = AXIS2_PLACEMENT_3D ( 'NONE', #17852, #21171, #27542 ) ;
#27460 = CARTESIAN_POINT ( 'NONE',  ( 7.021324086407807030, -24.55319635012989110, 6.700000000000000178 ) ) ;
#27461 = CARTESIAN_POINT ( 'NONE',  ( 25.25242209220571254, 2.014110669997101422, -4.189051521245521492 ) ) ;
#27462 = ORIENTED_EDGE ( 'NONE', *, *, #25439, .T. ) ;
#27463 = CARTESIAN_POINT ( 'NONE',  ( -36.34874870218064302, -26.64985754041175525, 6.700000000000000178 ) ) ;
#27464 = AXIS2_PLACEMENT_3D ( 'NONE', #36042, #39926, #30058 ) ;
#27465 = CARTESIAN_POINT ( 'NONE',  ( 70.86714415968630476, 59.66805877367134769, -3.971832046809243622 ) ) ;
#27466 = PRESENTATION_LAYER_ASSIGNMENT (  '', '', ( #31327 ) ) ;
#27467 = ORIENTED_EDGE ( 'NONE', *, *, #15247, .T. ) ;
#27468 = CARTESIAN_POINT ( 'NONE',  ( 87.12371845299759343, -1.516527252418922833, -4.675789953527256237 ) ) ;
#27469 = LINE ( 'NONE', #27066, #12047 ) ;
#27470 = CARTESIAN_POINT ( 'NONE',  ( 21.67762503442624222, 6.625004204850643674, 3.088539990067460828 ) ) ;
#27471 = ADVANCED_FACE ( 'NONE', ( #23957 ), #35591, .F. ) ;
#27472 = EDGE_CURVE ( 'NONE', #11154, #28588, #22171, .T. ) ;
#27474 = CARTESIAN_POINT ( 'NONE',  ( 4.854127076346722802, -30.84034076322234696, 7.761597726988851420 ) ) ;
#27473 = CARTESIAN_POINT ( 'NONE',  ( -0.9562383853963228875, -27.29125251401421082, 6.887161170156905321 ) ) ;
#27475 = ITEM_DEFINED_TRANSFORMATION ( 'NONE', 'NONE', #544,  #30744 ) ;
#27476 = DIRECTION ( 'NONE',  ( 0.000000000000000000, 0.000000000000000000, 1.000000000000000000 ) ) ;
#27477 = ORIENTED_EDGE ( 'NONE', *, *, #15336, .F. ) ;
#27478 = EDGE_CURVE ( 'NONE', #4150, #23269, #28737, .T. ) ;
#27479 = CARTESIAN_POINT ( 'NONE',  ( 21.71040439744254513, 6.342537115183759511, 3.188214735634443908 ) ) ;
#27480 =( NAMED_UNIT ( * ) PLANE_ANGLE_UNIT ( ) SI_UNIT ( $, .RADIAN. ) );
#27481 = B_SPLINE_CURVE_WITH_KNOTS ( 'NONE', 3,
 ( #11509, #24073, #36644, #8423, #21001, #3517, #38064, #9867, #40529, #31700, #22642, #21820, #31907, #616, #22440, #31093, #3718, #31298, #19134, #204, #12744, #16040, #25518, #16243, #38261, #12337, #34811, #34402, #37642, #35008, #18508 ),
 .UNSPECIFIED., .F., .F.,
 ( 4, 3, 3, 3, 3, 3, 3, 3, 3, 3, 4 ),
 ( 0.000000000000000000, 2.999644130997738061E-05, 6.002588995695006208E-05, 8.960886084588186925E-05, 0.0001190604700446505160, 0.0001489538463052745123, 0.0001796139255494018936, 0.0002109707048517112527, 0.0002426195318110425665, 0.0002740640997890109003, 0.0002849778069099932016 ),
 .UNSPECIFIED. ) ;
#27482 = VERTEX_POINT ( 'NONE', #39805 ) ;
#27483 = EDGE_LOOP ( 'NONE', ( #930, #1056, #36044, #36988 ) ) ;
#27484 = CARTESIAN_POINT ( 'NONE',  ( 79.32339967214609544, 64.38349706316869003, -3.578491385641962896 ) ) ;
#27485 = AXIS2_PLACEMENT_3D ( 'NONE', #12075, #27937, #3073 ) ;
#27486 = CARTESIAN_POINT ( 'NONE',  ( 21.04004256178996002, 8.045166779822325864, -2.500000000010173640 ) ) ;
#27487 = CARTESIAN_POINT ( 'NONE',  ( 81.36794360107698765, 64.82106189941457330, -2.952528780688971288 ) ) ;
#27488 = CARTESIAN_POINT ( 'NONE',  ( 79.54992950373221561, 64.18601594420306355, 3.671038198312437384 ) ) ;
#27489 = B_SPLINE_CURVE_WITH_KNOTS ( 'NONE', 3,
 ( #159, #25268, #6536, #19083, #31651, #5709, #21571, #18251, #34149, #5917, #31043, #2851, #15371, #27929, #40473, #9194, #29161, #38815, #4064, #28758, #10208, #35358, #7525, #22790, #7130, #3871, #16985, #22991, #35751, #4256, #969 ),
 .UNSPECIFIED., .F., .F.,
 ( 4, 3, 3, 3, 3, 3, 3, 3, 3, 3, 4 ),
 ( 8.940560153363745023E-19, 2.999644130997779397E-05, 6.002588995694919472E-05, 8.960886084588147622E-05, 0.0001190604700446495673, 0.0001489538463052725878, 0.0001796139255493967707, 0.0002109707048517091385, 0.0002426195318110357089, 0.0002740640997890029856, 0.0002849778069099823054 ),
 .UNSPECIFIED. ) ;
#27490 = VECTOR ( 'NONE', #36156, 1000.000000000000000 ) ;
#27491 = CARTESIAN_POINT ( 'NONE',  ( 0.9453370993353911178, -33.77429008742427641, 7.635761828346577573 ) ) ;
#27492 = CARTESIAN_POINT ( 'NONE',  ( 17.39327739772060255, 14.24814301257567273, 2.500000000000000444 ) ) ;
#27493 = CARTESIAN_POINT ( 'NONE',  ( 22.40835304001176098, 2.012838380346585243, -8.570566085397546274 ) ) ;
#27494 = VERTEX_POINT ( 'NONE', #11575 ) ;
#27495 = CARTESIAN_POINT ( 'NONE',  ( -77.90426910868221455, 9.924495015397090114, 8.801360606586941415 ) ) ;
#27496 = CARTESIAN_POINT ( 'NONE',  ( 37.06374037821629486, -3.173191448149650373, 5.964198512422226983 ) ) ;
#27497 = CARTESIAN_POINT ( 'NONE',  ( -0.1564234597993582332, -32.53678801801031284, 7.751599049952197618 ) ) ;
#27498 = CARTESIAN_POINT ( 'NONE',  ( -78.36759592796440188, 10.14500944777191371, -6.694231243261347331 ) ) ;
#27499 = FACE_OUTER_BOUND ( 'NONE', #37236, .T. ) ;
#27500 = CARTESIAN_POINT ( 'NONE',  ( 2.452196827863095674, -26.25408112137242611, 6.876076431790005827 ) ) ;
#27501 = DIRECTION ( 'NONE',  ( -0.000000000000000000, -0.000000000000000000, 1.000000000000000000 ) ) ;
#27502 = DIRECTION ( 'NONE',  ( -0.000000000000000000, -1.000000000000000000, -0.000000000000000000 ) ) ;
#27503 = CARTESIAN_POINT ( 'NONE',  ( 2.884763386751913572, -26.27641232226080703, 7.635761828346579350 ) ) ;
#27504 = DIRECTION ( 'NONE',  ( 0.4690749385695657803, 0.8831583674551003460, 0.000000000000000000 ) ) ;
#27505 = DIRECTION ( 'NONE',  ( -0.8660254037844381525, 0.000000000000000000, 0.5000000000000008882 ) ) ;
#27506 = PLANE ( 'NONE',  #6611 ) ;
#27507 = DIRECTION ( 'NONE',  ( 0.000000000000000000, 1.000000000000000000, 0.000000000000000000 ) ) ;
#27508 = CARTESIAN_POINT ( 'NONE',  ( 24.37979543224318846, 2.943268363220738149, -3.716964114009788656 ) ) ;
#27509 = ORIENTED_EDGE ( 'NONE', *, *, #13335, .T. ) ;
#27510 = CARTESIAN_POINT ( 'NONE',  ( 67.38390057489351648, 58.33093658501181267, 3.992553130659727056 ) ) ;
#27511 = CARTESIAN_POINT ( 'NONE',  ( 34.93082455767837757, -1.706425845107903960, 5.658197996046836487 ) ) ;
#27512 = CARTESIAN_POINT ( 'NONE',  ( 4.957641325759844619, -30.81012851192526014, 7.785344483711591934 ) ) ;
#27513 = ADVANCED_FACE ( 'NONE', ( #2769 ), #40607, .F. ) ;
#27514 = DIRECTION ( 'NONE',  ( 1.000000000000000000, 0.000000000000000000, 0.000000000000000000 ) ) ;
#27516 = EDGE_CURVE ( 'NONE', #36422, #21009, #18857, .T. ) ;
#27515 = CARTESIAN_POINT ( 'NONE',  ( 86.38515361113813640, 1.239318396469950123, 5.566871328843018496 ) ) ;
#27518 = CARTESIAN_POINT ( 'NONE',  ( 32.07397980944352156, -0.6787160600116808329, -5.212318280033424678 ) ) ;
#27517 = CARTESIAN_POINT ( 'NONE',  ( 30.63785892209476458, -0.4682215140425676214, 5.751446082446129537 ) ) ;
#27519 = ORIENTED_EDGE ( 'NONE', *, *, #28296, .F. ) ;
#27520 = CARTESIAN_POINT ( 'NONE',  ( -1.607555503064097113, -28.78410073912801437, 6.911401339314956260 ) ) ;
#27521 = CARTESIAN_POINT ( 'NONE',  ( -0.6817374880303864737, -32.13420688251338220, 6.903112506833889661 ) ) ;
#27522 = EDGE_CURVE ( 'NONE', #35485, #4455, #24517, .T. ) ;
#27523 = VECTOR ( 'NONE', #18580, 999.9999999999998863 ) ;
#27524 = ORIENTED_EDGE ( 'NONE', *, *, #32997, .T. ) ;
#27525 = CARTESIAN_POINT ( 'NONE',  ( -69.92837670882107659, -20.82254431570259001, 3.916079783099620126 ) ) ;
#27526 = ORIENTED_EDGE ( 'NONE', *, *, #9592, .T. ) ;
#27527 = CARTESIAN_POINT ( 'NONE',  ( 80.03595747215288725, 63.73611138703243029, -3.702313260098204939 ) ) ;
#27528 = DIRECTION ( 'NONE',  ( -0.9267318687906771491, 0.3757233601570964532, 0.000000000000000000 ) ) ;
#27529 = CARTESIAN_POINT ( 'NONE',  ( 81.06392658325412981, 61.26538850743066433, 1.312782405654757678 ) ) ;
#27531 = ORIENTED_EDGE ( 'NONE', *, *, #7153, .F. ) ;
#27530 = CARTESIAN_POINT ( 'NONE',  ( 4.782632897257695248, -27.91715820809518789, 7.766640943994648438 ) ) ;
#27532 = CARTESIAN_POINT ( 'NONE',  ( 74.52260502535293085, 62.13706486897681458, -3.724166978290282426 ) ) ;
#27533 = CIRCLE ( 'NONE', #9790, 0.1000000000000028644 ) ;
#27535 = CARTESIAN_POINT ( 'NONE',  ( -18.97867591359219475, -26.64985754041175525, 6.700000000000000178 ) ) ;
#27534 = FACE_OUTER_BOUND ( 'NONE', #848, .T. ) ;
#27536 = CARTESIAN_POINT ( 'NONE',  ( -1.193343473173243074, -27.78488342726187099, 7.774064877406527962 ) ) ;
#27537 = CARTESIAN_POINT ( 'NONE',  ( 21.86457316608978019, 5.764392919207080190, -3.219569754713741183 ) ) ;
#27538 = ORIENTED_EDGE ( 'NONE', *, *, #17362, .F. ) ;
#27539 = CARTESIAN_POINT ( 'NONE',  ( 5.024341273715212886, -30.28507763625619020, 6.864216812889196717 ) ) ;
#27540 = CARTESIAN_POINT ( 'NONE',  ( 24.06190720129734473, 2.407014782553678955, 5.659300396313236448 ) ) ;
#27541 = PLANE ( 'NONE',  #11702 ) ;
#27542 = DIRECTION ( 'NONE',  ( 1.000000000000000000, 0.000000000000000000, 0.000000000000000000 ) ) ;
#27543 = CARTESIAN_POINT ( 'NONE',  ( 81.15786166771449928, 61.29969053694482994, 1.104694797982963328 ) ) ;
#27544 = CARTESIAN_POINT ( 'NONE',  ( 87.87138265328074738, -2.102315541244656583, 2.954904511526853295 ) ) ;
#27545 = DIRECTION ( 'NONE',  ( 0.000000000000000000, 0.000000000000000000, 1.000000000000000000 ) ) ;
#27546 = ORIENTED_EDGE ( 'NONE', *, *, #23077, .T. ) ;
#27547 = FACE_OUTER_BOUND ( 'NONE', #12261, .T. ) ;
#27548 = CARTESIAN_POINT ( 'NONE',  ( 3.444544078574621970, -26.65138038738905735, 6.892063359921931642 ) ) ;
#27549 = CARTESIAN_POINT ( 'NONE',  ( -2.248748702180634940, -25.49307895267003587, 6.700000000000000178 ) ) ;
#27550 = CARTESIAN_POINT ( 'NONE',  ( 19.69399097454885705, -2.982692120004300840, -3.239409980100296238 ) ) ;
#27551 = CARTESIAN_POINT ( 'NONE',  ( 0.9213240864078056092, -26.64985754041175525, 6.700000000000000178 ) ) ;
#27552 = B_SPLINE_SURFACE_WITH_KNOTS ( 'NONE', 3, 3, ( 
 ( #22357, #38574, #4030, #25628, #25835, #31816, #13466, #16156, #3435, #7291, #38173, #29129, #38780 ),
 ( #22556, #38370, #13678, #19453, #3832, #19658, #15948, #28512, #10167, #35119, #322, #25428, #16352 ),
 ( #37969, #26040, #7094, #35326, #6700, #16548, #19249, #3631, #28720, #23938, #39802, #2147, #14268 ),
 ( #11169, #36311, #27042, #29920, #1341, #30134, #1949, #8082, #23740, #5015, #33450, #39586, #38971 ),
 ( #20648, #39379, #32632, #35918, #33229, #1531, #7697, #17546, #30340, #26839, #11371, #36510, #8283 ),
 ( #5218, #36117, #14467, #4427, #20246, #35717, #20858, #17753, #29721, #14065, #20446, #17342, #23552 ),
 ( #14665, #27236, #11572, #13877, #16951, #7493, #20053, #29529, #26444, #10770, #4619, #1737, #23346 ),
 ( #32828, #17149, #26642, #39176, #10972, #7894, #33025, #4815, #6241, #18785, #37515, #37316, #8696 ),
 ( #33646, #9310, #24560, #2355, #5626, #14874, #28254, #27446, #40397, #40002, #2562, #31159, #8491 ),
 ( #21689, #11772, #24770, #34466, #9114, #21072, #34267, #5421, #6038, #34061, #8900, #24352, #15291 ),
 ( #2766, #27844, #36916, #21276, #15084, #12199, #21483, #24978, #27645, #40603, #5834, #30961, #18573 ),
 ( #2975, #15494, #18374, #28054, #12409, #39076, #17863, #5328, #39289, #1852, #31018, #8186, #14374 ),
 ( #37573, #33553, #18634, #6097, #34326, #26944, #12470, #2055, #12257, #11077, #39486, #1642, #31219 ),
 ( #36414, #20758, #27142, #24046, #30240, #17447, #2827, #27904, #20973, #20550, #23647, #37376, #24831 ),
 ( #36615, #15348, #9370, #7994, #23839, #36214, #40448, #21744, #3039, #33134, #9172, #6301, #4917 ),
 ( #25040, #15557, #14180, #28114, #11276, #40666, #8399, #21954, #30037, #34528, #26750, #18850, #33349 ),
 ( #5125, #17658, #14568, #39694, #11482, #7306, #25643, #15766, #28733, #25848, #29140, #38587, #25244 ),
 ( #31624, #3450, #31423, #28322, #947, #3644, #37774, #3247, #26056, #12877, #35136, #741, #137 ),
 ( #13276, #22162, #38186, #15965, #38383, #37987, #12669, #7109, #9788, #10186, #22968, #13482, #19264 ),
 ( #10393, #13081, #9988, #3849, #9583, #35532, #22568, #34936, #34735, #6513, #19468, #19061, #32041 ),
 ( #16367, #28938, #22772, #35339, #19670, #32248, #33036, #39601, #1160, #4440, #26852, #26656, #39392 ),
 ( #29541, #27461, #33863, #24577, #30356, #8505, #30976, #8711, #21089, #2579, #2373, #18184, #2161 ),
 ( #27859, #12216, #5436, #15307, #9130, #8298, #30775, #37129, #2782, #14891, #40016, #40410, #24788 ),
 ( #5645, #24369, #20874, #5233, #15100, #17769, #14682, #39820, #11588, #24165, #8917, #27660, #40214 ),
 ( #27252, #17976, #30563, #18390, #11997, #21501, #34078, #5852, #39732, #10710, #26578, #1281, #30073 ),
 ( #36447, #26387, #17481, #8429, #7636, #17694, #27175, #8222, #16888, #30274, #17088, #4955, #26783 ),
 ( #13817, #2090, #29470, #39322, #23288, #4562, #20187, #7835, #1885, #14603, #29661, #21008, #11111 ),
 ( #29864, #39524, #11514, #24081, #33168, #1679, #5158, #14008, #20793, #4751, #23682, #11307, #38917 ),
 ( #14410, #36650, #33388, #32772, #4368, #20582, #8025, #35858, #1474, #26980, #10914, #39118, #23872 ),
 ( #36249, #23491, #36057, #20385, #32965, #17286, #14210, #2910, #2287, #33785, #33586, #9250, #9048 ),
 ( #11922, #18309, #15229, #21421, #8637, #37256, #18514, #12130, #11716, #30482, #27990, #15429, #19 ),
 ( #21625, #28190, #39942, #15025, #14812, #31100, #12345, #24918, #27379, #5974, #37651, #36853, #6180 ),
 ( #37453, #5362, #18722, #5562, #34206, #27783, #40337, #24291, #31304, #17901, #24708, #21213, #18103 ),
 ( #37051, #40536, #3128, #30694, #9453, #21828, #2501, #30900, #34408, #15643, #12549, #27588, #25119 ),
 ( #40140, #24497, #8837, #33996, #5771, #2709, #22037, #16634, #19140, #25726, #32131, #31504, #13563 ),
 ( #12751, #9665, #22650, #7185, #35216, #4121, #6987, #29218, #19554, #31913, #6791, #37862, #13166 ),
 ( #622, #38269, #25328, #26135, #10064, #211, #38668, #1028, #34613, #16046, #32323, #6390, #18939 ),
 ( #16445, #22845, #12960, #25525, #19746, #3328, #3724, #28819, #38070, #15846, #28403, #28614, #22252 ),
 ( #34819, #6595, #31707, #3929, #9872, #22447, #3523, #25929, #29020, #35418, #421, #824, #35015 ),
 ( #13355, #19343, #16249, #38463, #10265, #36197, #30016, #1834, #32518, #23631, #14552, #13768, #23821 ),
 ( #14356, #23046, #36397, #23241, #11060, #32913, #4703, #19939, #8170, #35611, #17238, #16838, #10662 ),
 ( #7976, #20739, #35809, #27127, #29811, #7382, #36005, #4897, #33327, #17640, #4316, #20530, #7584 ),
 ( #10466, #29422, #5106, #23439, #1236, #26339, #30220, #20139, #14157, #33116, #38871, #2037, #17428 ),
 ( #32719, #26926, #4515, #39469, #17034, #11256, #29610, #1429, #20332, #7784, #13962, #1622, #26529 ),
 ( #26731, #39063, #10860, #39268, #27734, #24445, #40482, #8587, #15382, #40089, #5720, #34157, #33536 ),
 ( #12293, #33944, #21165, #40289, #2453, #24654, #18258, #17846, #36600, #5926, #8998, #6131, #37406 ),
 ( #33731, #21368, #18667, #15176, #3075, #15593, #30428, #39677, #27327, #2238, #5510, #27537, #21781 ),
 ( #24866, #12077, #36800, #11868, #8378, #9201, #37003, #5310, #18054, #14758, #31256, #39891, #37204 ),
 ( #30643, #18465, #11459, #14977, #21578, #11665, #8784, #2859, #27939, #30851, #2657, #34359, #24027 ),
 ( #20953, #3879, #6544, #10013, #19698, #25876, #3472, #19291, #10216, #28563, #25474, #576, #37605 ),
 ( #9820, #31659, #771, #34564, #15994, #7138, #6336, #22596, #28767, #22399, #13303, #34966, #13115 ),
 ( #6741, #31455, #32273, #4072, #16200, #12906, #28968, #37808, #16395, #371, #31858, #35164, #21988 ),
 ( #38416, #3676, #9613, #25673, #38019, #38216, #18886, #28145, #22796, #35368, #22199, #40699, #12501 ),
 ( #6936, #19500, #25071, #19089, #32074, #9401, #3279, #15801, #28354, #165, #12702, #25276, #35758 ),
 ( #977, #13514, #26084, #38620, #7736, #29563, #13913, #14308, #26482, #7334, #4263, #29367, #7533 ) ),
 .UNSPECIFIED., .F., .F., .F.,
 ( 4, 3, 3, 3, 3, 3, 3, 3, 3, 3, 3, 3, 3, 3, 3, 3, 3, 3, 4 ),
 ( 4, 3, 3, 3, 4 ),
 ( 0.005001841298670386959, 0.005072013119329183903, 0.005142184939987979979, 0.005282528581305572998, 0.005563215863940759037, 0.006124590429211131982, 0.007247339559751877006, 0.008370088690292622896, 0.009492837820833367052, 0.01005421238610373913, 0.01061558695137411121, 0.01089627423400929725, 0.01117696151664448329, 0.01173833608191485710, 0.01286108521245560299, 0.01342245977772597507, 0.01370314706036116111, 0.01384349070167875326, 0.01398383434299634714 ),
 ( 0.000000000000000000, 0.2500000000000000000, 0.5000000000000000000, 0.7500000000000000000, 1.000000000000000000 ),
 .UNSPECIFIED. ) ;
#27553 = LINE ( 'NONE', #14570, #13653 ) ;
#27554 = VERTEX_POINT ( 'NONE', #32887 ) ;
#27555 = CARTESIAN_POINT ( 'NONE',  ( 35.33522163555373652, -3.168965096689021266, 5.721313940429516798 ) ) ;
#27556 = CARTESIAN_POINT ( 'NONE',  ( 4.323672655924887920, -31.73289041085212148, 7.730758795053802146 ) ) ;
#27557 = CARTESIAN_POINT ( 'NONE',  ( 88.23268491810016201, -0.7494148791586221492, 1.919551801057179263 ) ) ;
#27558 = ORIENTED_EDGE ( 'NONE', *, *, #19769, .T. ) ;
#27559 = VERTEX_POINT ( 'NONE', #16809 ) ;
#27561 = CARTESIAN_POINT ( 'NONE',  ( 37.18721867727772690, -2.963692379415546529, 6.000030405913790332 ) ) ;
#27560 = CARTESIAN_POINT ( 'NONE',  ( 79.22467975445887589, 65.90355157830848043, -2.361823859647588897 ) ) ;
#27562 = CARTESIAN_POINT ( 'NONE',  ( 26.16082219273550891, -2.761323807819567655, 4.289427023688758389 ) ) ;
#27563 = CARTESIAN_POINT ( 'NONE',  ( 3.465568536097964447, -32.59220555077066450, 7.640616322432101093 ) ) ;
#27564 = CARTESIAN_POINT ( 'NONE',  ( -78.45330471031414277, 33.71485196875532608, 15.50000000000000000 ) ) ;
#27565 = ADVANCED_FACE ( 'NONE', ( #29389 ), #1799, .F. ) ;
#27566 = VERTEX_POINT ( 'NONE', #13742 ) ;
#27567 = CARTESIAN_POINT ( 'NONE',  ( -1.740011302788441627, -30.21307731605675073, 7.686927408461906808 ) ) ;
#27568 = EDGE_CURVE ( 'NONE', #5299, #21616, #29776, .T. ) ;
#27569 = ORIENTED_EDGE ( 'NONE', *, *, #32206, .F. ) ;
#27570 = EDGE_CURVE ( 'NONE', #9241, #37233, #23469, .T. ) ;
#27571 = ORIENTED_EDGE ( 'NONE', *, *, #4755, .T. ) ;
#27572 = DIRECTION ( 'NONE',  ( 0.3420201433256662704, 0.9396926207859093161, -0.000000000000000000 ) ) ;
#27573 = CARTESIAN_POINT ( 'NONE',  ( 78.93014367432635936, 65.87924701951081374, -2.174925636353739922 ) ) ;
#27574 = CARTESIAN_POINT ( 'NONE',  ( 14.73610008032583885, -5.026708172105184502, 2.500480175786592874 ) ) ;
#27575 = ORIENTED_EDGE ( 'NONE', *, *, #236, .F. ) ;
#27577 = CARTESIAN_POINT ( 'NONE',  ( 21.42227782476107123, 8.036706878627773776, -2.736079366572905514 ) ) ;
#27576 = CARTESIAN_POINT ( 'NONE',  ( 22.49487306056245828, 2.478889120150127301, 4.939610370497833358 ) ) ;
#27578 = EDGE_LOOP ( 'NONE', ( #27176, #30260 ) ) ;
#27579 = CARTESIAN_POINT ( 'NONE',  ( 82.02451737050265024, 62.15044802891514308, -1.700667878122839261 ) ) ;
#27580 = VECTOR ( 'NONE', #28259, 1000.000000000000114 ) ;
#27581 = CARTESIAN_POINT ( 'NONE',  ( -53.21549048184568420, -30.38627270959228710, -4.152976064860135708 ) ) ;
#27582 = ORIENTED_EDGE ( 'NONE', *, *, #33196, .T. ) ;
#27583 = B_SPLINE_CURVE_WITH_KNOTS ( 'NONE', 3,
 ( #31510, #12554, #35022, #15437, #26, #6394, #6601, #25126, #15850, #2917 ),
 .UNSPECIFIED., .F., .F.,
 ( 4, 3, 3, 4 ),
 ( 0.0001585009270395724978, 0.0001815657551981850074, 0.0002118214035944123428, 0.0002170292169044763799 ),
 .UNSPECIFIED. ) ;
#27585 = CARTESIAN_POINT ( 'NONE',  ( 85.58789802481842912, 2.221335288533847319, -3.332472240576935363 ) ) ;
#27584 = DIRECTION ( 'NONE',  ( 0.3757233601570931225, 0.9267318687906784813, 0.000000000000000000 ) ) ;
#27586 = CARTESIAN_POINT ( 'NONE',  ( -1.798596309351013334, -29.48570337927768392, 6.865554069792297653 ) ) ;
#27587 = CARTESIAN_POINT ( 'NONE',  ( 74.44738948069034734, 59.23650550459285569, 3.391332960764822158 ) ) ;
#27588 = CARTESIAN_POINT ( 'NONE',  ( 22.03209494260425316, 3.823468488147809374, -4.290561760811918646 ) ) ;
#27589 = ORIENTED_EDGE ( 'NONE', *, *, #2049, .T. ) ;
#27590 = CARTESIAN_POINT ( 'NONE',  ( 0.5038905087661823545, -26.38741722279598534, 7.691066658568948888 ) ) ;
#27591 = CARTESIAN_POINT ( 'NONE',  ( 21.85643539959774273, 11.82890447862143546, -1.931159885854170311 ) ) ;
#27592 = CARTESIAN_POINT ( 'NONE',  ( -2.527465627618633803, -28.94812858826901802, 7.754798119455333705 ) ) ;
#27593 = ORIENTED_EDGE ( 'NONE', *, *, #2976, .F. ) ;
#27594 = CARTESIAN_POINT ( 'NONE',  ( 79.89307030929712994, 66.05340108613447114, 2.264354540981408093 ) ) ;
#27595 = CARTESIAN_POINT ( 'NONE',  ( 85.03556247682649882, 2.841744791465048880, -1.219259102000758821 ) ) ;
#27596 = DIRECTION ( 'NONE',  ( 1.000000000000000000, 0.000000000000000000, 0.000000000000000000 ) ) ;
#27597 = CARTESIAN_POINT ( 'NONE',  ( 2.721716728528035922, -32.91760109509163357, 6.989977667959444751 ) ) ;
#27598 = ORIENTED_EDGE ( 'NONE', *, *, #28704, .F. ) ;
#27599 = CARTESIAN_POINT ( 'NONE',  ( 0.6456758497273269448, -26.33765886672673062, 6.864276522220859711 ) ) ;
#27600 = LINE ( 'NONE', #37063, #40711 ) ;
#27601 = CARTESIAN_POINT ( 'NONE',  ( 36.89739936142836996, -3.002644431800062463, -5.965129555963346597 ) ) ;
#27602 = CARTESIAN_POINT ( 'NONE',  ( 0.9904113513190105911, -32.89497607571279758, 7.754798119455333705 ) ) ;
#27603 = CARTESIAN_POINT ( 'NONE',  ( 5.196076649799282521, -29.67970906813446064, 7.766640943994654656 ) ) ;
#27604 = CARTESIAN_POINT ( 'NONE',  ( -6.348748702180634140, -25.49307895267003587, 6.800000000000000711 ) ) ;
#27605 = LINE ( 'NONE', #30099, #34140 ) ;
#27606 = CARTESIAN_POINT ( 'NONE',  ( -34.87867591359218977, -24.55319635012989110, 6.800000000000000711 ) ) ;
#27607 = ORIENTED_EDGE ( 'NONE', *, *, #34525, .T. ) ;
#27608 = CARTESIAN_POINT ( 'NONE',  ( 36.63478925368298178, -2.000665574028761107, 5.847389373914565702 ) ) ;
#27609 = CARTESIAN_POINT ( 'NONE',  ( -70.81198565705318515, 0.2164538760997103128, 3.999856464806924361 ) ) ;
#27610 = CARTESIAN_POINT ( 'NONE',  ( 66.90064367344375285, 57.83598502562791310, -3.997265020308770289 ) ) ;
#27611 = FACE_OUTER_BOUND ( 'NONE', #11789, .T. ) ;
#27612 = ORIENTED_EDGE ( 'NONE', *, *, #3654, .F. ) ;
#27613 = CYLINDRICAL_SURFACE ( 'NONE', #29233, 0.09010775117052866046 ) ;
#27615 = EDGE_CURVE ( 'NONE', #6790, #5705, #23210, .T. ) ;
#27614 = LINE ( 'NONE', #49, #31836 ) ;
#27616 = DIRECTION ( 'NONE',  ( 0.4987820251299098784, 0.06975647374412531632, -0.8639158094271057742 ) ) ;
#27617 = EDGE_LOOP ( 'NONE', ( #13904, #15235, #20531, #23050 ) ) ;
#27618 = PLANE ( 'NONE',  #35246 ) ;
#27619 = DIRECTION ( 'NONE',  ( 0.000000000000000000, 0.000000000000000000, 1.000000000000000000 ) ) ;
#27620 = VERTEX_POINT ( 'NONE', #13930 ) ;
#27621 = CARTESIAN_POINT ( 'NONE',  ( 22.63992908519401581, 4.527459582470855004, 3.136945245597487553 ) ) ;
#27622 = CARTESIAN_POINT ( 'NONE',  ( 81.04763707098177861, 66.10603528134693363, -1.133121492189030244 ) ) ;
#27623 = CARTESIAN_POINT ( 'NONE',  ( 80.46181058475262660, 63.58258928487767037, 3.654032574946329603 ) ) ;
#27624 = CARTESIAN_POINT ( 'NONE',  ( 21.94884155547715920, 5.596816108778505772, -3.078664276110406384 ) ) ;
#27625 = ORIENTED_EDGE ( 'NONE', *, *, #32458, .F. ) ;
#27626 = CARTESIAN_POINT ( 'NONE',  ( 78.09760114435862022, 60.38799743245723306, -2.844364419925348830 ) ) ;
#27628 = CARTESIAN_POINT ( 'NONE',  ( 14.73630591169358617, -5.028744660188785076, -2.500462426279348893 ) ) ;
#27627 = CARTESIAN_POINT ( 'NONE',  ( 24.11813316538267316, 0.4652667653683164040, 5.100766439816002418 ) ) ;
#27629 = DIRECTION ( 'NONE',  ( 1.000000000000000000, -0.000000000000000000, 0.000000000000000000 ) ) ;
#27630 = CARTESIAN_POINT ( 'NONE',  ( 79.92917477698983930, 65.49944209122774907, -2.989933650881962279 ) ) ;
#27631 = CARTESIAN_POINT ( 'NONE',  ( 77.65955580186948737, 62.78993503910592011, 3.839379600940506343 ) ) ;
#27632 = ORIENTED_EDGE ( 'NONE', *, *, #1378, .T. ) ;
#27633 = AXIS2_PLACEMENT_3D ( 'NONE', #33079, #29772, #2202 ) ;
#27634 = DIRECTION ( 'NONE',  ( 0.1006641980670203301, -0.9949204587440765302, 0.000000000000000000 ) ) ;
#27635 = ORIENTED_EDGE ( 'NONE', *, *, #32739, .F. ) ;
#27636 = CARTESIAN_POINT ( 'NONE',  ( 81.73765358980278961, 61.68994590043250525, 1.132734665583299494 ) ) ;
#27637 =( BOUNDED_CURVE ( )  B_SPLINE_CURVE ( 3, ( #17708, #37065, #39752, #23891 ),
 .UNSPECIFIED., .F., .T. ) 
 B_SPLINE_CURVE_WITH_KNOTS ( ( 4, 4 ),
 ( 4.748221474220557958, 4.941946782021392259 ),
 .UNSPECIFIED. ) 
 CURVE ( )  GEOMETRIC_REPRESENTATION_ITEM ( )  RATIONAL_B_SPLINE_CURVE ( ( 1.000000000000000000, 0.9968749865767494445, 0.9968749865767494445, 1.000000000000000000 ) ) 
 REPRESENTATION_ITEM ( '' )  );
#27639 = DIRECTION ( 'NONE',  ( 0.1542073060391599970, 0.000000000000000000, -0.9880385148181951571 ) ) ;
#27638 = LINE ( 'NONE', #21683, #19799 ) ;
#27640 = CARTESIAN_POINT ( 'NONE',  ( 32.93308485139972674, -2.920656968542761245, -5.757540729513444866 ) ) ;
#27641 = EDGE_CURVE ( 'NONE', #36985, #33555, #10831, .T. ) ;
#27642 = CARTESIAN_POINT ( 'NONE',  ( -1.760064674761432801, -30.09457558617890527, 6.865554069792297653 ) ) ;
#27643 = DIRECTION ( 'NONE',  ( -0.3757233601570931225, -0.9267318687906784813, 0.000000000000000000 ) ) ;
#27644 = CARTESIAN_POINT ( 'NONE',  ( -64.30032790741496740, 34.77233229845844420, 5.249462333892575217 ) ) ;
#27645 = CARTESIAN_POINT ( 'NONE',  ( 22.64608778944036516, 0.3051270519629841194, -6.453714758063171075 ) ) ;
#27646 = DIRECTION ( 'NONE',  ( 0.000000000000000000, 0.000000000000000000, -1.000000000000000000 ) ) ;
#27647 = CARTESIAN_POINT ( 'NONE',  ( 5.001192086984713292, -30.73384879920740431, 7.710604733652629328 ) ) ;
#27648 = CARTESIAN_POINT ( 'NONE',  ( 5.166866161692755810, -29.08666662507720702, 7.750000000000000888 ) ) ;
#27649 = CARTESIAN_POINT ( 'NONE',  ( 36.84739796419923863, -2.124053305941548953, -5.880516947223020985 ) ) ;
#27650 = CARTESIAN_POINT ( 'NONE',  ( 3.413184693633389610, -32.60729755094480709, 7.783750581861600182 ) ) ;
#27651 = CYLINDRICAL_SURFACE ( 'NONE', #17620, 0.09010775117052910455 ) ;
#27652 = DIRECTION ( 'NONE',  ( -0.000000000000000000, -0.000000000000000000, 1.000000000000000000 ) ) ;
#27653 = LINE ( 'NONE', #31371, #7446 ) ;
#27654 = LINE ( 'NONE', #21701, #1007 ) ;
#27655 = B_SPLINE_CURVE_WITH_KNOTS ( 'NONE', 3,
 ( #7634, #7233, #19794, #7031, #3972, #29467, #16886, #13611, #19600, #1676 ),
 .UNSPECIFIED., .F., .F.,
 ( 4, 2, 2, 2, 4 ),
 ( 1.084202172485504434E-19, 0.0003915860703966683948, 0.0007831721407933366812, 0.001174758211190004859, 0.001566344281586673146 ),
 .UNSPECIFIED. ) ;
#27656 = CARTESIAN_POINT ( 'NONE',  ( 5.097277635046815192, -29.71537786563932215, 6.868387053540522480 ) ) ;
#27657 = FACE_OUTER_BOUND ( 'NONE', #34597, .T. ) ;
#27658 = EDGE_CURVE ( 'NONE', #22592, #2595, #32943, .T. ) ;
#27659 = CARTESIAN_POINT ( 'NONE',  ( 14.75868911325587796, -5.145464069203309343, -2.500012630750525933 ) ) ;
#27660 = CARTESIAN_POINT ( 'NONE',  ( 22.03785866058321119, 1.984797309109682217, -5.805693036113302341 ) ) ;
#27661 = ORIENTED_EDGE ( 'NONE', *, *, #13870, .T. ) ;
#27662 =( LENGTH_UNIT ( ) NAMED_UNIT ( * ) SI_UNIT ( .MILLI., .METRE. ) );
#27663 = CARTESIAN_POINT ( 'NONE',  ( 69.70139497306261944, 59.23354404394888917, -3.977789803233245269 ) ) ;
#27664 = CIRCLE ( 'NONE', #31622, 0.1000000000000028644 ) ;
#27665 = EDGE_LOOP ( 'NONE', ( #28118, #20, #18944, #11921 ) ) ;
#27666 = LINE ( 'NONE', #40417, #16029 ) ;
#27668 = EDGE_CURVE ( 'NONE', #28242, #6497, #40316, .T. ) ;
#27667 = LINE ( 'NONE', #295, #12743 ) ;
#27669 = CARTESIAN_POINT ( 'NONE',  ( 69.82526079983220768, 58.91932963963509451, 3.982895692900140894 ) ) ;
#27670 = CARTESIAN_POINT ( 'NONE',  ( 2.989640894365640289, -26.42383226750358816, 6.865312560952603782 ) ) ;
#27671 = CARTESIAN_POINT ( 'NONE',  ( -70.92837670882107659, -65.19654454972992141, 6.000000000000002665 ) ) ;
#27672 = CARTESIAN_POINT ( 'NONE',  ( 5.048237804244037008, -30.16315501756571393, 7.769368695748486431 ) ) ;
#27673 = ORIENTED_EDGE ( 'NONE', *, *, #28157, .T. ) ;
#27674 = CARTESIAN_POINT ( 'NONE',  ( 22.61684402008435768, 4.633385194857577716, 3.026614357573721215 ) ) ;
#27675 = AXIS2_PLACEMENT_3D ( 'NONE', #15498, #31567, #3390 ) ;
#27676 = ORIENTED_EDGE ( 'NONE', *, *, #15351, .T. ) ;
#27677 = CARTESIAN_POINT ( 'NONE',  ( 78.38646849266343963, 65.84297019793960715, -1.584170212883422524 ) ) ;
#27678 = CARTESIAN_POINT ( 'NONE',  ( 3.300000000000000711, 3.061616997868383141E-16, -2.500000000000000000 ) ) ;
#27679 = CARTESIAN_POINT ( 'NONE',  ( 78.68815740766761735, 66.05701152551952759, -1.050153991572640777 ) ) ;
#27680 = CARTESIAN_POINT ( 'NONE',  ( 78.92462413491021778, 65.07527128086412915, 3.128253119413329397 ) ) ;
#27681 = DIRECTION ( 'NONE',  ( 0.000000000000000000, -0.000000000000000000, 1.000000000000000000 ) ) ;
#27683 = VERTEX_POINT ( 'NONE', #26985 ) ;
#27682 = DIRECTION ( 'NONE',  ( 0.000000000000000000, 0.000000000000000000, 1.000000000000000000 ) ) ;
#27684 = CARTESIAN_POINT ( 'NONE',  ( 21.85643539959780313, -7.722266916079949972, 9.821539774841749448 ) ) ;
#27685 = VERTEX_POINT ( 'NONE', #10519 ) ;
#27686 = CARTESIAN_POINT ( 'NONE',  ( -78.52360362737910293, 11.36405371355654736, 6.517260701712046078 ) ) ;
#27687 = CARTESIAN_POINT ( 'NONE',  ( 35.65372115386870888, -3.750406728026652647, 5.582374933998859312 ) ) ;
#27688 = LINE ( 'NONE', #30599, #39232 ) ;
#27689 = CARTESIAN_POINT ( 'NONE',  ( -1.799609906766908685, -29.56993018339339940, 6.929570838012926615 ) ) ;
#27690 = CARTESIAN_POINT ( 'NONE',  ( 31.99016054316349056, -3.341357271039956611, -5.178217504156710227 ) ) ;
#27691 = CARTESIAN_POINT ( 'NONE',  ( 23.38648856837436441, 3.560657187999370699, -3.090153159693794116 ) ) ;
#27692 = LINE ( 'NONE', #21330, #39325 ) ;
#27693 = CARTESIAN_POINT ( 'NONE',  ( 15.09522703660796239, 11.91064461445325229, 2.554458953684618283 ) ) ;
#27694 = DIRECTION ( 'NONE',  ( -1.000000000000000000, 0.000000000000000000, -0.000000000000000000 ) ) ;
#27695 = CARTESIAN_POINT ( 'NONE',  ( 0.9213240864078056092, -26.64985754041175525, 6.700000000000000178 ) ) ;
#27696 = EDGE_CURVE ( 'NONE', #26593, #5299, #34672, .T. ) ;
#27697 = ADVANCED_FACE ( 'NONE', ( #36063 ), #14215, .T. ) ;
#27698 = CARTESIAN_POINT ( 'NONE',  ( 5.066811727378471630, -29.09326952720500969, 7.761597726988851420 ) ) ;
#27699 = EDGE_CURVE ( 'NONE', #33227, #7215, #1086, .T. ) ;
#27700 = CARTESIAN_POINT ( 'NONE',  ( 19.29296610083087415, 12.44317219469094660, -2.499999999999999556 ) ) ;
#27701 = AXIS2_PLACEMENT_3D ( 'NONE', #32770, #35461, #17283 ) ;
#27702 = CARTESIAN_POINT ( 'NONE',  ( 37.08720602107538866, -2.368560226880349173, -5.943858709518226036 ) ) ;
#27703 = CARTESIAN_POINT ( 'NONE',  ( 25.75309628829585762, 2.097993264449613537, -4.157463482038479263 ) ) ;
#27704 = ORIENTED_EDGE ( 'NONE', *, *, #26030, .F. ) ;
#27705 = CARTESIAN_POINT ( 'NONE',  ( -69.43806570890772889, -47.31353566070715999, 5.812001725005383257 ) ) ;
#27706 = CARTESIAN_POINT ( 'NONE',  ( 67.09515986712425217, 58.21407947277521089, 3.993497817183392584 ) ) ;
#27707 = CARTESIAN_POINT ( 'NONE',  ( 34.38864450132898298, -1.330693349609932241, 5.573577685579110153 ) ) ;
#27708 = CARTESIAN_POINT ( 'NONE',  ( -1.662376691416499019, -30.07172650866636587, 7.778050822775631978 ) ) ;
#27709 = LINE ( 'NONE', #12886, #8224 ) ;
#27710 = CARTESIAN_POINT ( 'NONE',  ( 85.36258410344761671, 2.204690851838579047, 4.549306268726941660 ) ) ;
#27711 = ADVANCED_FACE ( 'NONE', ( #10921 ), #8031, .T. ) ;
#27713 = CARTESIAN_POINT ( 'NONE',  ( 35.92909550028735310, -2.111770154685527423, -5.814002319914921557 ) ) ;
#27712 = CARTESIAN_POINT ( 'NONE',  ( -75.45330471031414277, 33.71485196875532608, -8.800414904976364028 ) ) ;
#27714 = CARTESIAN_POINT ( 'NONE',  ( -1.558538563793567588, -30.53915227141846955, 6.920489980334481928 ) ) ;
#27715 = EDGE_LOOP ( 'NONE', ( #4985, #18537, #7771, #22284 ) ) ;
#27716 = CARTESIAN_POINT ( 'NONE',  ( -1.604992392964304626, -28.77340840982227732, 6.949473656533219135 ) ) ;
#27717 = CARTESIAN_POINT ( 'NONE',  ( -8.348748702180635917, -26.64985754041175525, 6.800000000000000711 ) ) ;
#27718 = EDGE_LOOP ( 'NONE', ( #19219, #20172, #19244, #25337, #2846, #39687, #16188, #21600 ) ) ;
#27719 = CARTESIAN_POINT ( 'NONE',  ( -40.97867591359219119, -26.64985754041175525, 6.700000000000000178 ) ) ;
#27720 = ORIENTED_EDGE ( 'NONE', *, *, #39453, .F. ) ;
#27721 = CARTESIAN_POINT ( 'NONE',  ( 79.06216475166031898, 65.51459655345134081, -2.804471013201359497 ) ) ;
#27722 = CARTESIAN_POINT ( 'NONE',  ( -1.519718581689926351, -28.19846911342024143, 6.984548363133217030 ) ) ;
#27723 = CARTESIAN_POINT ( 'NONE',  ( 79.33915194569573259, 65.11111034845949064, 3.233326467035608331 ) ) ;
#27725 = VERTEX_POINT ( 'NONE', #1287 ) ;
#27724 = DIRECTION ( 'NONE',  ( -0.000000000000000000, -1.000000000000000000, -0.000000000000000000 ) ) ;
#27726 = EDGE_CURVE ( 'NONE', #25277, #35446, #22899, .T. ) ;
#27727 = CARTESIAN_POINT ( 'NONE',  ( 74.74317362787380148, 60.13816936446348649, -3.762445401688810698 ) ) ;
#27728 = AXIS2_PLACEMENT_3D ( 'NONE', #33113, #27324, #26728 ) ;
#27729 = DIRECTION ( 'NONE',  ( -1.000000000000000000, 0.000000000000000000, 0.000000000000000000 ) ) ;
#27731 = FACE_OUTER_BOUND ( 'NONE', #2997, .T. ) ;
#27730 = CARTESIAN_POINT ( 'NONE',  ( 4.918643498309219986, -30.94573722681042582, 6.951256099901581997 ) ) ;
#27732 = CARTESIAN_POINT ( 'NONE',  ( 3.438683469850188690, -26.53211252316276259, 7.635761828346582014 ) ) ;
#27733 = PLANE ( 'NONE',  #35997 ) ;
#27734 = CARTESIAN_POINT ( 'NONE',  ( 23.42254319797303452, 3.705070095891317639, -3.277622970724664686 ) ) ;
#27735 = ORIENTED_EDGE ( 'NONE', *, *, #15251, .T. ) ;
#27736 = CARTESIAN_POINT ( 'NONE',  ( -1.303108374136985104, -31.16335321463953534, 7.754798119455333705 ) ) ;
#27737 = EDGE_CURVE ( 'NONE', #10898, #19388, #38562, .T. ) ;
#27738 = CARTESIAN_POINT ( 'NONE',  ( 24.55145103709714505, -1.086933616027371263, 6.883468691731016165 ) ) ;
#27739 = ADVANCED_FACE ( 'NONE', ( #7434, #35467 ), #23688, .F. ) ;
#27740 = DIRECTION ( 'NONE',  ( -0.000000000000000000, 1.000000000000000000, -0.000000000000000000 ) ) ;
#27741 = CARTESIAN_POINT ( 'NONE',  ( 5.009673027830494618, -30.35011694869506371, 7.006423389747791219 ) ) ;
#27742 = CARTESIAN_POINT ( 'NONE',  ( 81.09074532527962731, 63.51554843946190232, 3.425340496581063654 ) ) ;
#27743 = CARTESIAN_POINT ( 'NONE',  ( 87.24982552262115121, -1.326261458569501839, 4.881571762780114732 ) ) ;
#27744 = DIRECTION ( 'NONE',  ( 0.8660254037844380415, 0.5000000000000009992, -0.000000000000000000 ) ) ;
#27745 = ORIENTED_EDGE ( 'NONE', *, *, #28504, .F. ) ;
#27746 = CARTESIAN_POINT ( 'NONE',  ( 2.869513165557623147, -26.27096686817759874, 7.660770905198779346 ) ) ;
#27747 = CARTESIAN_POINT ( 'NONE',  ( -72.35147488751991318, -46.63281737808343053, 9.898294814228878025 ) ) ;
#27748 = EDGE_CURVE ( 'NONE', #15627, #28082, #32577, .T. ) ;
#27749 = CARTESIAN_POINT ( 'NONE',  ( -61.24591834330252027, -23.80776546975053520, -2.500000000000000000 ) ) ;
#27750 = CARTESIAN_POINT ( 'NONE',  ( 14.86430981739665746, -4.493068681216141336, -2.516462316360253748 ) ) ;
#27751 = CARTESIAN_POINT ( 'NONE',  ( -65.33937732661527775, 36.44481994371090394, -7.201454646436823204 ) ) ;
#27752 = DIRECTION ( 'NONE',  ( 1.385724075720358314E-16, -1.000000000000000000, 0.000000000000000000 ) ) ;
#27753 = CARTESIAN_POINT ( 'NONE',  ( -0.4014682958407423952, -26.89743201442601972, 7.768425012602594215 ) ) ;
#27754 = CARTESIAN_POINT ( 'NONE',  ( 34.33173276390347439, -1.489116378852566980, 5.564695232538289460 ) ) ;
#27755 = DIRECTION ( 'NONE',  ( -0.000000000000000000, -0.000000000000000000, 1.000000000000000000 ) ) ;
#27756 = DIRECTION ( 'NONE',  ( -0.000000000000000000, -0.000000000000000000, -1.000000000000000000 ) ) ;
#27757 = VERTEX_POINT ( 'NONE', #29274 ) ;
#27759 = CARTESIAN_POINT ( 'NONE',  ( 36.13337973148855298, -1.529159196477766880, 5.642270371453538047 ) ) ;
#27758 = CARTESIAN_POINT ( 'NONE',  ( 80.77164629763790060, 63.73694215246327133, -3.562450064734660415 ) ) ;
#27760 = CARTESIAN_POINT ( 'NONE',  ( 21.59288859382414572, -2.652561316991649765, 3.576490509687073160 ) ) ;
#27761 = CARTESIAN_POINT ( 'NONE',  ( 17.57044049449111967, -3.218502976824792139, -2.911085957591616591 ) ) ;
#27762 = VECTOR ( 'NONE', #37336, 1000.000000000000000 ) ;
#27763 = CARTESIAN_POINT ( 'NONE',  ( 14.61802080322610919, 12.62870316934875881, -2.500000000000000000 ) ) ;
#27764 = ORIENTED_EDGE ( 'NONE', *, *, #34058, .F. ) ;
#27765 = PLANE ( 'NONE',  #4322 ) ;
#27766 = ORIENTED_EDGE ( 'NONE', *, *, #14302, .F. ) ;
#27767 = ORIENTED_EDGE ( 'NONE', *, *, #26630, .T. ) ;
#27768 = CARTESIAN_POINT ( 'NONE',  ( 80.04018988431747061, 64.49293993294404004, -3.578839808218921004 ) ) ;
#27769 = DIRECTION ( 'NONE',  ( 0.4999999999999979461, 0.8660254037844397068, -0.000000000000000000 ) ) ;
#27770 = ORIENTED_EDGE ( 'NONE', *, *, #8105, .F. ) ;
#27772 = CARTESIAN_POINT ( 'NONE',  ( 14.73664178711200101, 12.61985148690355985, 2.505541970458036616 ) ) ;
#27771 = CARTESIAN_POINT ( 'NONE',  ( 22.04733053187323222, 2.939797654462655618, 4.949211021722255133 ) ) ;
#27773 = VERTEX_POINT ( 'NONE', #39124 ) ;
#27774 = CARTESIAN_POINT ( 'NONE',  ( 82.02157412789767932, 62.93630067300345843, -2.502189764415934548 ) ) ;
#27775 = EDGE_CURVE ( 'NONE', #28759, #28641, #14285, .T. ) ;
#27776 = CARTESIAN_POINT ( 'NONE',  ( 79.89212576172680258, 63.66154800590240370, 4.000000000000000000 ) ) ;
#27777 = EDGE_LOOP ( 'NONE', ( #40216, #37246, #20847, #7521 ) ) ;
#27779 = CARTESIAN_POINT ( 'NONE',  ( 87.04213330793400871, 0.5878691963681514920, -4.891134986362597914 ) ) ;
#27778 = CARTESIAN_POINT ( 'NONE',  ( -20.87867591359218977, -26.64985754041175525, 6.700000000000000178 ) ) ;
#27780 = CARTESIAN_POINT ( 'NONE',  ( -1.799316637852572009, -29.52373849819694485, 6.880608371227948439 ) ) ;
#27781 = CARTESIAN_POINT ( 'NONE',  ( -12.44874870218064267, -26.64985754041175525, 6.800000000000000711 ) ) ;
#27782 = CARTESIAN_POINT ( 'NONE',  ( 74.62207946275562165, 60.41194043352551546, 3.856662941142526169 ) ) ;
#27783 = CARTESIAN_POINT ( 'NONE',  ( 23.26269754767185560, 3.142007143762405086, -3.939437242187847410 ) ) ;
#27784 = ORIENTED_EDGE ( 'NONE', *, *, #31745, .F. ) ;
#27785 = CARTESIAN_POINT ( 'NONE',  ( -4.890026461918809630, -25.50263309590217276, 27.90461065042423527 ) ) ;
#27786 = CARTESIAN_POINT ( 'NONE',  ( 21.85643539959777826, -4.218647804531223677, -15.78683364351815221 ) ) ;
#27787 = CARTESIAN_POINT ( 'NONE',  ( 3.543304674501073226, -26.59746626410985826, 7.766640943994650215 ) ) ;
#27788 = ORIENTED_EDGE ( 'NONE', *, *, #5864, .F. ) ;
#27789 = CARTESIAN_POINT ( 'NONE',  ( 81.88105255503974433, 62.58610580235438192, 2.445541897054072766 ) ) ;
#27790 = CARTESIAN_POINT ( 'NONE',  ( 88.38542499104009664, -0.9209797785659445957, 1.969977704346236536 ) ) ;
#27791 = CARTESIAN_POINT ( 'NONE',  ( 16.11725891507163766, 15.27317977277692052, -2.500000000000000000 ) ) ;
#27792 = AXIS2_PLACEMENT_3D ( 'NONE', #33672, #26666, #10993 ) ;
#27793 = ADVANCED_FACE ( 'NONE', ( #11119 ), #33174, .T. ) ;
#27794 = ADVANCED_FACE ( 'NONE', ( #26584 ), #13824, .F. ) ;
#27795 = CARTESIAN_POINT ( 'NONE',  ( 2.788398779348973733, -32.89652560498232248, 6.865482280155368322 ) ) ;
#27796 = CARTESIAN_POINT ( 'NONE',  ( 26.27633885242532585, -3.098738397173856018, 4.268606335983216482 ) ) ;
#27797 = DIRECTION ( 'NONE',  ( 1.000000000000000000, 7.232507224765808510E-18, 0.000000000000000000 ) ) ;
#27798 = EDGE_CURVE ( 'NONE', #14959, #3867, #35865, .T. ) ;
#27799 = CARTESIAN_POINT ( 'NONE',  ( 29.13959756157474246, 0.4692356663346191059, -4.754336961950639484 ) ) ;
#27800 = CARTESIAN_POINT ( 'NONE',  ( 5.100295740189424443, -29.54432006460276128, 7.652160403243382980 ) ) ;
#27801 = CARTESIAN_POINT ( 'NONE',  ( 4.633009665528590837, -31.48036009422220616, 6.980586498568963627 ) ) ;
#27802 = DIRECTION ( 'NONE',  ( -0.000000000000000000, -0.000000000000000000, 1.000000000000000000 ) ) ;
#27803 = CARTESIAN_POINT ( 'NONE',  ( 21.81833114184418321, 5.350335711903964508, -3.566543258216577250 ) ) ;
#27804 = DIRECTION ( 'NONE',  ( -0.000000000000000000, -0.000000000000000000, 1.000000000000000000 ) ) ;
#27805 = ORIENTED_EDGE ( 'NONE', *, *, #20871, .T. ) ;
#27806 = CARTESIAN_POINT ( 'NONE',  ( 37.17273293948297663, -2.956732537645826220, 5.999804286280149945 ) ) ;
#27807 = CARTESIAN_POINT ( 'NONE',  ( -71.35621909400492768, 0.1208619214844364048, 3.984726467720987042 ) ) ;
#27808 = CARTESIAN_POINT ( 'NONE',  ( 66.81810912255278367, 58.06508983445694128, -3.996770903032645261 ) ) ;
#27809 = EDGE_LOOP ( 'NONE', ( #12625, #32363 ) ) ;
#27810 = CARTESIAN_POINT ( 'NONE',  ( 88.19592634550657806, -0.7081259057544491142, 2.233392006332136859 ) ) ;
#27811 = CARTESIAN_POINT ( 'NONE',  ( -71.86858480636978186, 0.9314695403570354415, -9.956036837141201801 ) ) ;
#27812 = CARTESIAN_POINT ( 'NONE',  ( -71.72734055786713725, -21.39831690710585477, 5.947291465561956869 ) ) ;
#27813 = FACE_OUTER_BOUND ( 'NONE', #7924, .T. ) ;
#27814 = ORIENTED_EDGE ( 'NONE', *, *, #449, .T. ) ;
#27815 = DIRECTION ( 'NONE',  ( 0.000000000000000000, 0.000000000000000000, -1.000000000000000000 ) ) ;
#27816 = CARTESIAN_POINT ( 'NONE',  ( -1.531573891984414848, -33.61112889622174293, 7.754798119455333705 ) ) ;
#27817 = ORIENTED_EDGE ( 'NONE', *, *, #28369, .F. ) ;
#27818 = CARTESIAN_POINT ( 'NONE',  ( 23.42725932339659423, 3.763513707203086867, 3.172503157220333048 ) ) ;
#27819 = CARTESIAN_POINT ( 'NONE',  ( 81.62248346935345467, 65.70993096190730398, -1.000000000000000000 ) ) ;
#27820 = CARTESIAN_POINT ( 'NONE',  ( 78.70126604931442671, 66.02149264047228883, 1.577285172236843280 ) ) ;
#27821 = CARTESIAN_POINT ( 'NONE',  ( -0.1730901457863348591, -32.40719633966231328, 6.920489980334476599 ) ) ;
#27822 = ORIENTED_EDGE ( 'NONE', *, *, #30743, .T. ) ;
#27823 = CARTESIAN_POINT ( 'NONE',  ( 77.29563288604617810, 62.10585478181958763, -3.856837490696089610 ) ) ;
#27824 = B_SPLINE_CURVE_WITH_KNOTS ( 'NONE', 3,
 ( #21200, #36435, #40322, #11294, #33774, #8206, #39511, #20781, #5144, #27574, #33374, #11500, #17677, #5551, #14590, #11703, #33983, #24065 ),
 .UNSPECIFIED., .F., .F.,
 ( 4, 2, 2, 2, 2, 2, 2, 2, 4 ),
 ( -5.999999609784804829E-08, 8.963808126167891594E-05, 0.0001793361625194556759, 0.0003587323250350066208, 0.0005381284875505575657, 0.0006278265688083316557, 0.0006726756094372194055, 0.0006951001297516632262, 0.0007175246500661071553 ),
 .UNSPECIFIED. ) ;
#27826 = CARTESIAN_POINT ( 'NONE',  ( 3.751251297819363728, -26.64985754041175525, 6.800000000000000711 ) ) ;
#27825 = CARTESIAN_POINT ( 'NONE',  ( -1.852189108926798777, -33.38420822586166281, 6.894806418505347700 ) ) ;
#27827 = CARTESIAN_POINT ( 'NONE',  ( 0.5199030923387487624, -26.38144301222279964, 7.748216051605120391 ) ) ;
#27828 = CARTESIAN_POINT ( 'NONE',  ( 79.01071357413613327, 66.12284964548064181, -1.692865493181706649 ) ) ;
#27829 = CARTESIAN_POINT ( 'NONE',  ( 77.96902425052304864, 62.15836910947907512, 3.808649511194706516 ) ) ;
#27830 = VERTEX_POINT ( 'NONE', #17094 ) ;
#27831 = B_SPLINE_CURVE_WITH_KNOTS ( 'NONE', 3,
 ( #10060, #22645, #23237, #23042, #29016, #29418, #35211, #13765, #820, #35806 ),
 .UNSPECIFIED., .F., .F.,
 ( 4, 3, 3, 4 ),
 ( 0.0002170292169044783044, 0.0002420761345915947911, 0.0002723302478207000944, 0.0002816811360866801079 ),
 .UNSPECIFIED. ) ;
#27832 = AXIS2_PLACEMENT_3D ( 'NONE', #38377, #13077, #4040 ) ;
#27833 = DIRECTION ( 'NONE',  ( -0.1385056645183609658, 0.9903616414705929127, 3.027401012299304875E-16 ) ) ;
#27834 = VECTOR ( 'NONE', #39567, 1000.000000000000000 ) ;
#27835 = VERTEX_POINT ( 'NONE', #29667 ) ;
#27836 = CARTESIAN_POINT ( 'NONE',  ( 81.88767907424694670, 65.09350295521473129, 2.164558651853291771 ) ) ;
#27839 = VERTEX_POINT ( 'NONE', #1479 ) ;
#27838 = CARTESIAN_POINT ( 'NONE',  ( -1.698824908307911219, -29.49622598863939871, 6.874555630061442102 ) ) ;
#27837 = DIRECTION ( 'NONE',  ( -1.000000000000000000, 0.000000000000000000, 0.000000000000000000 ) ) ;
#27840 = CARTESIAN_POINT ( 'NONE',  ( 30.81316972100007590, -2.191302700533721115, -5.899179390191041428 ) ) ;
#27841 = DIRECTION ( 'NONE',  ( -0.000000000000000000, -0.000000000000000000, 1.000000000000000000 ) ) ;
#27842 = CARTESIAN_POINT ( 'NONE',  ( -1.601932461984457490, -30.40839394270583540, 7.505001789837628223 ) ) ;
#27843 = CARTESIAN_POINT ( 'NONE',  ( 1.510748483419375621, -33.06479068383551123, 6.931070083220559397 ) ) ;
#27844 = CARTESIAN_POINT ( 'NONE',  ( 26.67714935503705931, 0.9909774768816611568, -4.380117908427034301 ) ) ;
#27845 = ADVANCED_FACE ( 'NONE', ( #24504 ), #5367, .F. ) ;
#27846 = LINE ( 'NONE', #14876, #2481 ) ;
#27847 = CARTESIAN_POINT ( 'NONE',  ( 1.664433243520564654, -26.07011488755866679, 7.695279973900954751 ) ) ;
#27848 = CARTESIAN_POINT ( 'NONE',  ( 5.198120437317888864, -29.69595573662939358, 7.750000000000000888 ) ) ;
#27849 = EDGE_CURVE ( 'NONE', #25767, #24264, #1051, .T. ) ;
#27850 = CARTESIAN_POINT ( 'NONE',  ( 36.70922304957898064, -3.420571215935285903, -5.875113064356194847 ) ) ;
#27851 = DIRECTION ( 'NONE',  ( -0.000000000000000000, -0.000000000000000000, 1.000000000000000000 ) ) ;
#27852 = CARTESIAN_POINT ( 'NONE',  ( 1.138951562800235795, -32.92325491812241012, 7.661510568013095934 ) ) ;
#27853 = PLANE ( 'NONE',  #35168 ) ;
#27854 = DIRECTION ( 'NONE',  ( -1.000000000000000000, 0.000000000000000000, 0.000000000000000000 ) ) ;
#27855 = LINE ( 'NONE', #34476, #23355 ) ;
#27856 = CARTESIAN_POINT ( 'NONE',  ( -75.25715755557821751, 8.188700395369970408, 10.38624776870203981 ) ) ;
#27857 = CARTESIAN_POINT ( 'NONE',  ( 86.59537683758360060, -0.3992097724244685342, -5.811584838773467432 ) ) ;
#27858 = DIRECTION ( 'NONE',  ( 1.000000000000000000, 0.000000000000000000, 0.000000000000000000 ) ) ;
#27859 = CARTESIAN_POINT ( 'NONE',  ( 25.38987815660813041, 2.286237158485121324, -4.080818507191673383 ) ) ;
#27860 = CARTESIAN_POINT ( 'NONE',  ( -26.44874870218064089, -26.64985754041175525, 6.800000000000000711 ) ) ;
#27861 = EDGE_LOOP ( 'NONE', ( #18252, #33936 ) ) ;
#27862 = ORIENTED_EDGE ( 'NONE', *, *, #5582, .T. ) ;
#27863 = FACE_OUTER_BOUND ( 'NONE', #13098, .T. ) ;
#27864 = CARTESIAN_POINT ( 'NONE',  ( 69.89919258653301881, 58.73135405362895511, -3.965028736237033780 ) ) ;
#27865 = AXIS2_PLACEMENT_3D ( 'NONE', #32802, #35492, #1709 ) ;
#27866 = ORIENTED_EDGE ( 'NONE', *, *, #12820, .T. ) ;
#27867 = VECTOR ( 'NONE', #17687, 1000.000000000000000 ) ;
#27868 = DIRECTION ( 'NONE',  ( -0.000000000000000000, -1.000000000000000000, -0.000000000000000000 ) ) ;
#27869 = DIRECTION ( 'NONE',  ( -1.000000000000000000, -8.706234683161959233E-16, 0.000000000000000000 ) ) ;
#27870 = LINE ( 'NONE', #17988, #38623 ) ;
#27871 = CARTESIAN_POINT ( 'NONE',  ( 1.192341134868766028, -26.20810236866151754, 6.870716933885665512 ) ) ;
#27872 = ADVANCED_FACE ( 'NONE', ( #11520 ), #10562, .T. ) ;
#27873 = CARTESIAN_POINT ( 'NONE',  ( 5.046791071466609324, -30.17131961341260649, 7.775108481317161591 ) ) ;
#27874 = ORIENTED_EDGE ( 'NONE', *, *, #10918, .F. ) ;
#27875 = CARTESIAN_POINT ( 'NONE',  ( 21.98910052706983365, 5.614098391567612367, 3.090586958385738825 ) ) ;
#27876 = VECTOR ( 'NONE', #27919, 1000.000000000000114 ) ;
#27877 = ORIENTED_EDGE ( 'NONE', *, *, #15327, .T. ) ;
#27878 = CARTESIAN_POINT ( 'NONE',  ( 78.37355578220726215, 65.75145430471653185, -1.935054690158703128 ) ) ;
#27879 =( BOUNDED_CURVE ( )  B_SPLINE_CURVE ( 3, ( #11269, #36409, #8180, #20752 ),
 .UNSPECIFIED., .F., .T. ) 
 B_SPLINE_CURVE_WITH_KNOTS ( ( 4, 4 ),
 ( 1.347909859412854461, 1.534781240595299856 ),
 .UNSPECIFIED. ) 
 CURVE ( )  GEOMETRIC_REPRESENTATION_ITEM ( )  RATIONAL_B_SPLINE_CURVE ( ( 1.000000000000000000, 0.9970920404276226723, 0.9970920404276226723, 1.000000000000000000 ) ) 
 REPRESENTATION_ITEM ( '' )  );
#27880 = CARTESIAN_POINT ( 'NONE',  ( -1.485716978080746209, -30.75683203970418944, 7.652160403243385645 ) ) ;
#27881 = CARTESIAN_POINT ( 'NONE',  ( 79.93288853953357886, 66.07525097314714912, -2.222430037836083727 ) ) ;
#27882 = CARTESIAN_POINT ( 'NONE',  ( 79.32339967214608123, 64.38349706316869003, 3.578491385641963785 ) ) ;
#27883 = EDGE_CURVE ( 'NONE', #21217, #35449, #24762, .T. ) ;
#27884 = FACE_OUTER_BOUND ( 'NONE', #35644, .T. ) ;
#27885 = CARTESIAN_POINT ( 'NONE',  ( 2.806342938108580043, -32.78503022925695376, 7.785172627573962778 ) ) ;
#27886 = CARTESIAN_POINT ( 'NONE',  ( 22.75155763331752112, -5.137713618528696458, -6.528071535057289765 ) ) ;
#27887 = EDGE_LOOP ( 'NONE', ( #14245, #18036, #3945, #21877 ) ) ;
#27888 = CARTESIAN_POINT ( 'NONE',  ( -71.75673233877098767, 2.217010188227585665, 9.965676783907941427 ) ) ;
#27889 = CARTESIAN_POINT ( 'NONE',  ( 34.29746155415688236, -3.857051845548268521, 5.268846866181171151 ) ) ;
#27890 = CARTESIAN_POINT ( 'NONE',  ( -63.38942448388426243, -60.53509472482660669, 0.000000000000000000 ) ) ;
#27891 = VECTOR ( 'NONE', #13647, 1000.000000000000000 ) ;
#27892 = CARTESIAN_POINT ( 'NONE',  ( -53.21549048184568420, -30.38627270959228710, 4.000000000000000000 ) ) ;
#27893 = EDGE_CURVE ( 'NONE', #39394, #9668, #16001, .T. ) ;
#27894 = CARTESIAN_POINT ( 'NONE',  ( 33.45155509882757627, -3.250653912085893715, -5.427322220725915969 ) ) ;
#27895 = CARTESIAN_POINT ( 'NONE',  ( 34.79242720853928006, -3.835804077954089397, -5.376515837512373608 ) ) ;
#27896 = APPLICATION_CONTEXT ( 'automotive_design' ) ;
#27897 = CARTESIAN_POINT ( 'NONE',  ( -1.754526989783608437, -30.08320498581767666, 7.776484688137383472 ) ) ;
#27898 = CARTESIAN_POINT ( 'NONE',  ( 15.05256153508802086, 12.14757130736968449, 2.534552796716138978 ) ) ;
#27899 = DIRECTION ( 'NONE',  ( 1.000000000000000000, 0.000000000000000000, 0.000000000000000000 ) ) ;
#27900 = CARTESIAN_POINT ( 'NONE',  ( 38.29999999999999716, 0.000000000000000000, 0.000000000000000000 ) ) ;
#27901 = CARTESIAN_POINT ( 'NONE',  ( 5.050665697719591840, -28.99051485080055102, 7.775108481317161591 ) ) ;
#27902 = VECTOR ( 'NONE', #22054, 1000.000000000000000 ) ;
#27903 = DIRECTION ( 'NONE',  ( -0.000000000000000000, -1.000000000000000000, -0.000000000000000000 ) ) ;
#27904 = CARTESIAN_POINT ( 'NONE',  ( 23.11875216611918660, 0.3874244158500451674, -5.890943838375131136 ) ) ;
#27905 = CARTESIAN_POINT ( 'NONE',  ( 30.30972199426953040, -3.799155601095605128, -4.460120920599953465 ) ) ;
#27906 = CARTESIAN_POINT ( 'NONE',  ( 24.71566706424699689, 3.001517176038623447, -3.434326518345315105 ) ) ;
#27907 = ORIENTED_EDGE ( 'NONE', *, *, #35268, .F. ) ;
#27908 = CARTESIAN_POINT ( 'NONE',  ( -69.42837670882107659, -47.21594255105944171, 5.809475019311132193 ) ) ;
#27909 = CARTESIAN_POINT ( 'NONE',  ( 67.10107710889761279, 58.19782780592215943, 3.994504660676310159 ) ) ;
#27910 = CARTESIAN_POINT ( 'NONE',  ( 34.95690096516870682, -1.636465606770671100, 5.662267850096001531 ) ) ;
#27911 = DIRECTION ( 'NONE',  ( 1.000000000000000000, 0.000000000000000000, 0.000000000000000000 ) ) ;
#27912 = DIRECTION ( 'NONE',  ( -0.9848077530122015810, -0.1736481776669674404, 0.000000000000000000 ) ) ;
#27913 = CARTESIAN_POINT ( 'NONE',  ( 88.80901725076027731, -1.591322664339660298, -1.862171775454326550 ) ) ;
#27915 = CARTESIAN_POINT ( 'NONE',  ( 35.98288326577282703, -3.153944312834425556, -5.822397201580947979 ) ) ;
#27914 = CARTESIAN_POINT ( 'NONE',  ( 29.67925625648019405, 0.9272574953382407559, 4.669903954941619695 ) ) ;
#27916 = ORIENTED_EDGE ( 'NONE', *, *, #37780, .T. ) ;
#27917 = CARTESIAN_POINT ( 'NONE',  ( 24.58210053396808448, 2.978637365502128542, 3.574180794472539446 ) ) ;
#27918 = EDGE_CURVE ( 'NONE', #38404, #29405, #3478, .T. ) ;
#27919 = DIRECTION ( 'NONE',  ( -0.7660444431189725734, -0.6427876096865456912, -0.000000000000000000 ) ) ;
#27920 = ORIENTED_EDGE ( 'NONE', *, *, #7555, .F. ) ;
#27921 = CARTESIAN_POINT ( 'NONE',  ( -70.14820770166069508, -21.41850222705690143, 5.961650403247820584 ) ) ;
#27922 = VECTOR ( 'NONE', #27502, 1000.000000000000000 ) ;
#27923 = ORIENTED_EDGE ( 'NONE', *, *, #39836, .T. ) ;
#27924 = CARTESIAN_POINT ( 'NONE',  ( 80.11945187304007732, 63.42025125984802969, -3.710743084827438310 ) ) ;
#27925 = VECTOR ( 'NONE', #9525, 1000.000000000000000 ) ;
#27926 = EDGE_CURVE ( 'NONE', #4011, #9702, #17905, .T. ) ;
#27927 = CARTESIAN_POINT ( 'NONE',  ( 2.921324086407800280, -26.64985754041175525, 6.700000000000000178 ) ) ;
#27928 = CARTESIAN_POINT ( 'NONE',  ( 80.29143557890645866, 63.14717164025322660, 3.649417990092601372 ) ) ;
#27930 = EDGE_LOOP ( 'NONE', ( #21292, #20542, #7179, #36739 ) ) ;
#27929 = CARTESIAN_POINT ( 'NONE',  ( -1.333638583621181928, -31.10443431896878508, 6.895222827070020877 ) ) ;
#27931 = ADVANCED_FACE ( 'NONE', ( #2293 ), #14819, .T. ) ;
#27932 = CIRCLE ( 'NONE', #5574, 3.000000000000002665 ) ;
#27933 = ADVANCED_FACE ( 'NONE', ( #5569 ), #18108, .F. ) ;
#27934 = DIRECTION ( 'NONE',  ( 0.7660444431189857850, -0.6427876096865300370, -0.000000000000000000 ) ) ;
#27936 = CARTESIAN_POINT ( 'NONE',  ( -29.07867591359219617, -26.64985754041175525, 6.700000000000000178 ) ) ;
#27935 = DIRECTION ( 'NONE',  ( 0.3757233601570964532, 0.9267318687906771491, -0.000000000000000000 ) ) ;
#27937 = DIRECTION ( 'NONE',  ( 1.047444401652940007E-14, -1.000000000000000000, -0.000000000000000000 ) ) ;
#27938 = DIRECTION ( 'NONE',  ( -0.6427876096865328126, -0.7660444431189835646, -0.000000000000000000 ) ) ;
#27939 = CARTESIAN_POINT ( 'NONE',  ( 22.40201758004466015, 4.861284111922041795, -3.110657656184960373 ) ) ;
#27940 = VERTEX_POINT ( 'NONE', #31460 ) ;
#27941 = DIRECTION ( 'NONE',  ( -1.000000000000000000, -7.232507224765808510E-18, 0.000000000000000000 ) ) ;
#27942 = CARTESIAN_POINT ( 'NONE',  ( 24.54460225945253526, -1.054324096271329614, -6.891227800717186547 ) ) ;
#27943 = CARTESIAN_POINT ( 'NONE',  ( -77.84099478799700478, -6.330046395677443982, -7.228837368596992441 ) ) ;
#27944 = EDGE_CURVE ( 'NONE', #38484, #39394, #37139, .T. ) ;
#27945 = CARTESIAN_POINT ( 'NONE',  ( 5.007316143351812521, -30.36002356176803829, 6.920489980334479263 ) ) ;
#27946 = CARTESIAN_POINT ( 'NONE',  ( 79.15160802321621247, 66.03480532732626784, 2.011547652603496328 ) ) ;
#27947 = CARTESIAN_POINT ( 'NONE',  ( 87.06687503756165825, -0.7302844941506287935, -5.541598948305895611 ) ) ;
#27948 = CARTESIAN_POINT ( 'NONE',  ( -0.2487487021806331078, -26.64985754041175525, 6.800000000000000711 ) ) ;
#27949 = ORIENTED_EDGE ( 'NONE', *, *, #4869, .F. ) ;
#27950 = CARTESIAN_POINT ( 'NONE',  ( -64.36785089794297221, 34.71712033580043055, -5.456534462680674658 ) ) ;
#27951 = CARTESIAN_POINT ( 'NONE',  ( 4.639291099620161063, -31.27958793520167191, 7.775108481317161591 ) ) ;
#27952 = VECTOR ( 'NONE', #7773, 1000.000000000000000 ) ;
#27953 = CARTESIAN_POINT ( 'NONE',  ( 4.029674975067525367, -26.95754872143103498, 6.863784140767622333 ) ) ;
#27954 = CARTESIAN_POINT ( 'NONE',  ( 14.92718052254917183, -5.911376862938025667, -2.518629130483756473 ) ) ;
#27955 = CARTESIAN_POINT ( 'NONE',  ( 36.44585954531025607, -2.356780152367485393, -5.894655847126518466 ) ) ;
#27956 = CARTESIAN_POINT ( 'NONE',  ( -2.585338981833881000, -32.18494463595775557, 7.754798119455333705 ) ) ;
#27957 = CARTESIAN_POINT ( 'NONE',  ( 1.793640042356549946, -26.17119502933373809, 6.866852738645443210 ) ) ;
#27958 = VERTEX_POINT ( 'NONE', #15805 ) ;
#27959 = CARTESIAN_POINT ( 'NONE',  ( 36.44622604588383297, -2.355887491903832398, 5.894713048404869760 ) ) ;
#27960 = CIRCLE ( 'NONE', #14174, 1.000000000000002220 ) ;
#27961 = EDGE_CURVE ( 'NONE', #6853, #26757, #32080, .T. ) ;
#27962 = CARTESIAN_POINT ( 'NONE',  ( 85.13880989351328310, 2.725772392624387308, 0.2960746283792183853 ) ) ;
#27963 = ORIENTED_EDGE ( 'NONE', *, *, #2853, .T. ) ;
#27965 = DIRECTION ( 'NONE',  ( 1.000000000000000000, 0.000000000000000000, 0.000000000000000000 ) ) ;
#27964 = CARTESIAN_POINT ( 'NONE',  ( 80.13405435096433393, 64.91068451853310250, -3.368075118064919327 ) ) ;
#27966 = CARTESIAN_POINT ( 'NONE',  ( 25.89546385390948657, -2.750212554045368130, 4.248011437199279428 ) ) ;
#27967 = DIRECTION ( 'NONE',  ( 0.000000000000000000, 0.6834397476448840214, 0.7300069255418726311 ) ) ;
#27968 = PLANE ( 'NONE',  #14523 ) ;
#27969 = CARTESIAN_POINT ( 'NONE',  ( 27.33867765376834313, -4.445383502205745074, -3.667891126866987594 ) ) ;
#27970 = VERTEX_POINT ( 'NONE', #22601 ) ;
#27971 = ORIENTED_EDGE ( 'NONE', *, *, #2049, .F. ) ;
#27972 = CARTESIAN_POINT ( 'NONE',  ( 78.71191388991731230, 66.03048852543453506, -1.560659576774502622 ) ) ;
#27973 = CARTESIAN_POINT ( 'NONE',  ( -1.506494769919744403, -28.44037730863004398, 7.680992449362117114 ) ) ;
#27974 = EDGE_CURVE ( 'NONE', #5793, #30874, #29173, .T. ) ;
#27975 = ORIENTED_EDGE ( 'NONE', *, *, #35088, .T. ) ;
#27977 = CARTESIAN_POINT ( 'NONE',  ( 31.60216379219463789, 0.4244636512702888442, 4.640344443660871399 ) ) ;
#27976 = CARTESIAN_POINT ( 'NONE',  ( 23.82088032715813242, 2.765655670818042200, 4.014859125618367663 ) ) ;
#27978 = ORIENTED_EDGE ( 'NONE', *, *, #5820, .F. ) ;
#27979 = EDGE_CURVE ( 'NONE', #36468, #9338, #4472, .T. ) ;
#27980 = CARTESIAN_POINT ( 'NONE',  ( 80.30040509403147553, 65.99001427540433440, -2.270757614041408523 ) ) ;
#27981 = CIRCLE ( 'NONE', #33261, 6.000000000000002665 ) ;
#27982 = AXIS2_PLACEMENT_3D ( 'NONE', #35985, #1605, #38249 ) ;
#27983 = CARTESIAN_POINT ( 'NONE',  ( 4.740160921379847458, -31.30480577326951064, 7.750000000000000000 ) ) ;
#27985 = CARTESIAN_POINT ( 'NONE',  ( 86.15668803663793085, 1.582443350855704978, -4.576617297167563159 ) ) ;
#27984 = CARTESIAN_POINT ( 'NONE',  ( -70.31448100068961082, 0.01729022305976556789, 5.969247584478902802 ) ) ;
#27986 = DIRECTION ( 'NONE',  ( 0.000000000000000000, 0.000000000000000000, -1.000000000000000000 ) ) ;
#27987 = CARTESIAN_POINT ( 'NONE',  ( 0.5871758347987294790, -26.26248204398054753, 7.780491323090171996 ) ) ;
#27988 = CARTESIAN_POINT ( 'NONE',  ( 73.28086911227147482, 60.35416371166882499, 3.944160774611113585 ) ) ;
#27989 = ORIENTED_EDGE ( 'NONE', *, *, #1104, .T. ) ;
#27990 = CARTESIAN_POINT ( 'NONE',  ( 22.23429677150355843, 3.418736078724165850, -4.405329081129731428 ) ) ;
#27991 = ORIENTED_EDGE ( 'NONE', *, *, #11596, .T. ) ;
#27992 = DIRECTION ( 'NONE',  ( -0.000000000000000000, -0.000000000000000000, -1.000000000000000000 ) ) ;
#27993 = AXIS2_PLACEMENT_3D ( 'NONE', #14655, #39166, #39792 ) ;
#27994 = CARTESIAN_POINT ( 'NONE',  ( 21.85643539959778892, -12.39743456692229628, -10.22857181343751520 ) ) ;
#27995 = CARTESIAN_POINT ( 'NONE',  ( 16.10603109343461981, 15.28195951419911580, 3.145749391472286050 ) ) ;
#27996 = ORIENTED_EDGE ( 'NONE', *, *, #21970, .F. ) ;
#27997 = CARTESIAN_POINT ( 'NONE',  ( 28.44383639013767962, -4.073698245608341040, -4.060485434070885802 ) ) ;
#27998 = CARTESIAN_POINT ( 'NONE',  ( 80.26729624682498354, 65.68772892857236911, 2.758880570191253323 ) ) ;
#27999 = SHAPE_REPRESENTATION ( 'Press Pin', ( #30744 ), #8364 ) ;
#28000 = CARTESIAN_POINT ( 'NONE',  ( 87.15505355144220800, 0.4610318193416703680, -5.246243280819175681 ) ) ;
#28001 = ORIENTED_EDGE ( 'NONE', *, *, #10372, .T. ) ;
#28002 = B_SPLINE_CURVE_WITH_KNOTS ( 'NONE', 3,
 ( #3593, #16117, #28683, #13028, #25592, #38136, #3791, #9937, #22518, #6861 ),
 .UNSPECIFIED., .F., .F.,
 ( 4, 3, 3, 4 ),
 ( 2.168404344971008868E-19, 3.025570593003071339E-05, 6.051145698343921226E-05, 6.468151674593626945E-05 ),
 .UNSPECIFIED. ) ;
#28003 = CARTESIAN_POINT ( 'NONE',  ( 2.730055066371769090, -32.91505153338314216, 6.903112506833889661 ) ) ;
#28004 = CARTESIAN_POINT ( 'NONE',  ( 21.53101133388948085, -2.979226547270804382, 3.510723884023187136 ) ) ;
#28005 = CARTESIAN_POINT ( 'NONE',  ( 25.06775773363566984, 3.218135757308234091, 2.425511022795127758 ) ) ;
#28006 = CARTESIAN_POINT ( 'NONE',  ( 22.97036411035692538, 2.781245753741529825, -3.791478878413661047 ) ) ;
#28007 = LINE ( 'NONE', #21437, #22068 ) ;
#28008 = CARTESIAN_POINT ( 'NONE',  ( 21.78047190118184773, 5.616103730238553027, 3.473245441588607374 ) ) ;
#28009 = CARTESIAN_POINT ( 'NONE',  ( -64.01189449551645794, 34.81586596186931359, 6.999999999999992006 ) ) ;
#28010 = DIRECTION ( 'NONE',  ( 0.000000000000000000, 0.000000000000000000, 1.000000000000000000 ) ) ;
#28011 = AXIS2_PLACEMENT_3D ( 'NONE', #30606, #33501, #2415 ) ;
#28012 = ORIENTED_EDGE ( 'NONE', *, *, #20688, .F. ) ;
#28013 = ORIENTED_EDGE ( 'NONE', *, *, #17895, .T. ) ;
#28014 = CARTESIAN_POINT ( 'NONE',  ( 37.00785681416889616, -3.244586891125645245, 5.947379696897557189 ) ) ;
#28015 = EDGE_LOOP ( 'NONE', ( #1528, #36675, #37777, #7225 ) ) ;
#28016 = CARTESIAN_POINT ( 'NONE',  ( 66.74404603967394678, 57.81040951471371159, -3.998354769210576976 ) ) ;
#28017 = EDGE_CURVE ( 'NONE', #20612, #309, #15764, .T. ) ;
#28018 = CARTESIAN_POINT ( 'NONE',  ( 87.65927558969256950, -2.189574935990458382, -2.847504520461086486 ) ) ;
#28019 = VECTOR ( 'NONE', #38566, 1000.000000000000000 ) ;
#28020 = ORIENTED_EDGE ( 'NONE', *, *, #21656, .T. ) ;
#28021 = CARTESIAN_POINT ( 'NONE',  ( -57.59497484894375674, 32.71166363405644262, 4.078840986107554301 ) ) ;
#28022 = ADVANCED_FACE ( 'NONE', ( #10617 ), #20094, .T. ) ;
#28023 = CARTESIAN_POINT ( 'NONE',  ( -72.11214491845440477, -0.3118290589227806775, -9.931028944812110737 ) ) ;
#28024 = CARTESIAN_POINT ( 'NONE',  ( 16.66455774270143664, 9.373215685664842312, 2.807305288237325502 ) ) ;
#28025 = ORIENTED_EDGE ( 'NONE', *, *, #13576, .T. ) ;
#28026 = CARTESIAN_POINT ( 'NONE',  ( 1.700390093233090871, -29.56993018339339940, 7.800000000000000711 ) ) ;
#28027 = DIRECTION ( 'NONE',  ( 0.000000000000000000, 0.000000000000000000, 1.000000000000000000 ) ) ;
#28028 = VERTEX_POINT ( 'NONE', #32671 ) ;
#28029 = CARTESIAN_POINT ( 'NONE',  ( 22.40535950346533056, 4.849712323715404061, 3.119056588188622303 ) ) ;
#28030 = EDGE_CURVE ( 'NONE', #33546, #10597, #32682, .T. ) ;
#28031 = CARTESIAN_POINT ( 'NONE',  ( 82.42900007550682062, 62.86339166853757376, -1.342843868341962343 ) ) ;
#28032 = CARTESIAN_POINT ( 'NONE',  ( 81.11951992695615843, 61.28566998660698317, 1.215327096190474965 ) ) ;
#28033 = EDGE_CURVE ( 'NONE', #18658, #36134, #26089, .T. ) ;
#28034 = CARTESIAN_POINT ( 'NONE',  ( -0.1781345077003545219, -32.40385772722507340, 6.959317978105162616 ) ) ;
#28035 = EDGE_LOOP ( 'NONE', ( #5995, #36821, #28865, #20815 ) ) ;
#28036 = CARTESIAN_POINT ( 'NONE',  ( 76.86947707741236968, 60.02096306738866360, -3.097219288968816375 ) ) ;
#28038 = CARTESIAN_POINT ( 'NONE',  ( 0.1331427388959149360, -0.6000000000000004219, 3.927368078836517729 ) ) ;
#28037 = CARTESIAN_POINT ( 'NONE',  ( 2.338742698598151204, -26.12863595720122234, 6.894806418505347700 ) ) ;
#28039 = CARTESIAN_POINT ( 'NONE',  ( 15.16793238289938373, 11.41091229596485057, -2.573720704819107308 ) ) ;
#28040 = CARTESIAN_POINT ( 'NONE',  ( 81.34140156818914136, 61.66514490546132521, -2.058202901128797446 ) ) ;
#28041 = CARTESIAN_POINT ( 'NONE',  ( 78.76819457884748488, 61.97782169454070811, 3.640295653905004425 ) ) ;
#28042 = EDGE_LOOP ( 'NONE', ( #37078, #18709, #14238, #37293 ) ) ;
#28043 = CARTESIAN_POINT ( 'NONE',  ( -32.34874870218063592, -25.49307895267003587, 6.800000000000000711 ) ) ;
#28044 = DIRECTION ( 'NONE',  ( -1.000000000000000000, 0.000000000000000000, 0.000000000000000000 ) ) ;
#28045 = CARTESIAN_POINT ( 'NONE',  ( 81.07719038108473342, 65.78599662769329370, 2.192618372226455836 ) ) ;
#28047 = FACE_OUTER_BOUND ( 'NONE', #26376, .T. ) ;
#28046 = CARTESIAN_POINT ( 'NONE',  ( 4.292159273299870570, -31.92212432182409287, 6.870724624169667116 ) ) ;
#28048 = CARTESIAN_POINT ( 'NONE',  ( 31.44014676667174157, -3.103618331322294921, 5.406754918213918515 ) ) ;
#28049 = VECTOR ( 'NONE', #32212, 1000.000000000000114 ) ;
#28050 =( BOUNDED_SURFACE ( )  B_SPLINE_SURFACE ( 3, 2, ( 
 ( #30458, #37232, #30879 ),
 ( #30673, #30051, #27763 ),
 ( #15208, #8814, #8613 ),
 ( #36831, #20985, #33563 ) ),
 .UNSPECIFIED., .F., .F., .T. ) 
 B_SPLINE_SURFACE_WITH_KNOTS ( ( 4, 4 ),
 ( 3, 3 ),
 ( 0.000000000000000000, 0.0008754244208249594870 ),
 ( 0.000000000000000000, 1.000000000000000000 ),
 .UNSPECIFIED. ) 
 GEOMETRIC_REPRESENTATION_ITEM ( )  RATIONAL_B_SPLINE_SURFACE ( (
 ( 1.000000000000000000, 0.9970051441236976730, 1.000000000000000000),
 ( 1.000000000000000000, 0.9987001331027346440, 1.000000000000000000),
 ( 1.000000000000000000, 0.9999578578056158573, 1.000000000000000000),
 ( 1.000000000000000000, 1.000000000000000000, 1.000000000000000000) ) ) 
 REPRESENTATION_ITEM ( '' )  SURFACE ( )  );
#28051 = DIRECTION ( 'NONE',  ( -1.000000000000000000, 8.723105632544016523E-16, 0.000000000000000000 ) ) ;
#28052 = CARTESIAN_POINT ( 'NONE',  ( -62.75662366181008878, 35.73757431566994569, -5.477568781475775417 ) ) ;
#28053 = CARTESIAN_POINT ( 'NONE',  ( -64.44214806826555275, 36.58397470404603524, 5.707342493247510973 ) ) ;
#28054 = CARTESIAN_POINT ( 'NONE',  ( 25.35178780325773218, 0.7567565456469654839, -4.605944304649653986 ) ) ;
#28055 = AXIS2_PLACEMENT_3D ( 'NONE', #9829, #38027, #12141 ) ;
#28056 = PLANE ( 'NONE',  #16900 ) ;
#28057 = DIRECTION ( 'NONE',  ( 0.000000000000000000, 0.000000000000000000, 1.000000000000000000 ) ) ;
#28058 = LINE ( 'NONE', #15088, #13772 ) ;
#28059 = PLANE ( 'NONE',  #35438 ) ;
#28060 = CARTESIAN_POINT ( 'NONE',  ( 33.66549675240646167, -3.596112717151957572, -5.375207407732099263 ) ) ;
#28061 = CARTESIAN_POINT ( 'NONE',  ( 81.14431272898491443, 61.29471917812056603, -1.169946933694579583 ) ) ;
#28062 = VECTOR ( 'NONE', #24599, 1000.000000000000000 ) ;
#28063 = CARTESIAN_POINT ( 'NONE',  ( 1.754540994691119460, -33.27093018339341768, 7.695279973900954751 ) ) ;
#28064 = CARTESIAN_POINT ( 'NONE',  ( 4.358291535071522560, -27.29274773012506827, 7.697032948437508182 ) ) ;
#28065 = DIRECTION ( 'NONE',  ( 0.000000000000000000, 0.000000000000000000, -1.000000000000000000 ) ) ;
#28066 = CARTESIAN_POINT ( 'NONE',  ( 2.111802210604301511, -32.94495686453777239, 6.887945620086121323 ) ) ;
#28067 = CARTESIAN_POINT ( 'NONE',  ( -62.96463773297413269, 37.71389135159273565, -4.136849086240373730 ) ) ;
#28068 = CARTESIAN_POINT ( 'NONE',  ( 21.47057743101996152, 7.821696842773389058, 2.778301367339317984 ) ) ;
#28069 = CARTESIAN_POINT ( 'NONE',  ( -1.512578315116791750, -30.68206402898919904, 6.889465824494257262 ) ) ;
#28070 = ORIENTED_EDGE ( 'NONE', *, *, #10593, .F. ) ;
#28071 = CARTESIAN_POINT ( 'NONE',  ( -14.24874870218063450, -26.64985754041175525, 6.700000000000000178 ) ) ;
#28072 = CARTESIAN_POINT ( 'NONE',  ( 69.94804423520642445, 58.60696991578217308, -3.944663542062683881 ) ) ;
#28073 = CIRCLE ( 'NONE', #26755, 3.449999999999999734 ) ;
#28074 = VERTEX_POINT ( 'NONE', #28974 ) ;
#28075 = CARTESIAN_POINT ( 'NONE',  ( -0.9624133124989321386, -27.31194369618440732, 7.778495531946297170 ) ) ;
#28076 = CARTESIAN_POINT ( 'NONE',  ( 0.05654071202359058079, -26.59372095824146243, 6.880147297696980857 ) ) ;
#28077 = PLANE ( 'NONE',  #28677 ) ;
#28078 = VECTOR ( 'NONE', #35374, 1000.000000000000000 ) ;
#28079 = CIRCLE ( 'NONE', #23472, 3.499999999999999556 ) ;
#28081 = EDGE_CURVE ( 'NONE', #38902, #19590, #28526, .T. ) ;
#28080 = DIRECTION ( 'NONE',  ( 0.000000000000000000, 0.000000000000000000, 1.000000000000000000 ) ) ;
#28082 = VERTEX_POINT ( 'NONE', #38221 ) ;
#28083 = CARTESIAN_POINT ( 'NONE',  ( 23.44311166670899027, 3.801244202611772760, 3.077376805319965936 ) ) ;
#28084 = EDGE_CURVE ( 'NONE', #24333, #7, #7337, .T. ) ;
#28085 = ORIENTED_EDGE ( 'NONE', *, *, #21256, .T. ) ;
#28086 = EDGE_CURVE ( 'NONE', #20612, #32452, #776, .T. ) ;
#28087 = ORIENTED_EDGE ( 'NONE', *, *, #25026, .T. ) ;
#28088 = CARTESIAN_POINT ( 'NONE',  ( 80.40236172895532718, 61.11465044667751556, -2.108843360059433625 ) ) ;
#28090 = CARTESIAN_POINT ( 'NONE',  ( -1.678016691892348700, -29.95251036351044149, 6.959317978105168834 ) ) ;
#28089 = CARTESIAN_POINT ( 'NONE',  ( 24.12062818113409435, 0.5588176674967194613, 5.091530623029829172 ) ) ;
#28091 = CARTESIAN_POINT ( 'NONE',  ( 81.87453109492308556, 63.55405699985828960, -2.808566127056343564 ) ) ;
#28092 = CARTESIAN_POINT ( 'NONE',  ( 80.65804582012491153, 61.64568945823259583, 2.699019001080979141 ) ) ;
#28093 = CARTESIAN_POINT ( 'NONE',  ( -18.44874870218064089, -26.64985754041175525, 6.700000000000000178 ) ) ;
#28094 = DIRECTION ( 'NONE',  ( 0.000000000000000000, -0.000000000000000000, 1.000000000000000000 ) ) ;
#28095 = CARTESIAN_POINT ( 'NONE',  ( 21.85643539959777115, 3.923092093126210322, -11.21220060410217734 ) ) ;
#28096 = DIRECTION ( 'NONE',  ( -0.000000000000000000, -0.000000000000000000, -1.000000000000000000 ) ) ;
#28097 = ORIENTED_EDGE ( 'NONE', *, *, #1532, .F. ) ;
#28098 = CARTESIAN_POINT ( 'NONE',  ( -73.12593961609827886, 4.566678402415828231, 9.815056785847646736 ) ) ;
#28099 = CARTESIAN_POINT ( 'NONE',  ( 37.19253098679411806, -2.880311961911129703, 5.999669043459923579 ) ) ;
#28100 = VERTEX_POINT ( 'NONE', #25880 ) ;
#28101 = CARTESIAN_POINT ( 'NONE',  ( -64.78958187800138546, -27.85319909218681644, 0.000000000000000000 ) ) ;
#28102 = DIRECTION ( 'NONE',  ( -0.000000000000000000, -0.000000000000000000, -1.000000000000000000 ) ) ;
#28103 = CARTESIAN_POINT ( 'NONE',  ( 1.616945372681888538, -32.96890605541899077, 6.870716933885664623 ) ) ;
#28104 = CARTESIAN_POINT ( 'NONE',  ( 36.71933413544295632, -3.459668038622879305, -5.860247842560236009 ) ) ;
#28105 = FACE_OUTER_BOUND ( 'NONE', #15781, .T. ) ;
#28106 = CARTESIAN_POINT ( 'NONE',  ( 14.72178876176509199, 13.26025408016186802, 2.500108498187831430 ) ) ;
#28107 = CARTESIAN_POINT ( 'NONE',  ( -73.45070404594234503, 38.65432087843066000, -9.800414904976365804 ) ) ;
#28108 = CARTESIAN_POINT ( 'NONE',  ( 4.317861630214887114, -31.73992721779714898, 7.643333865083951295 ) ) ;
#28109 = PRODUCT_DEFINITION_FORMATION_WITH_SPECIFIED_SOURCE ( 'ANY', '', #11783, .NOT_KNOWN. ) ;
#28110 = CARTESIAN_POINT ( 'NONE',  ( 0.7149948906900660539, -26.31585638355339185, 7.013842709614101167 ) ) ;
#28111 = AXIS2_PLACEMENT_3D ( 'NONE', #26840, #5220, #23553 ) ;
#28112 = CIRCLE ( 'NONE', #11628, 114.6618724293813898 ) ;
#28113 = CARTESIAN_POINT ( 'NONE',  ( 18.47097006516344564, 13.26508273762688717, -2.500000000000000000 ) ) ;
#28114 = CARTESIAN_POINT ( 'NONE',  ( 25.22036471513533584, 0.8962270189713842372, -4.613828365072303761 ) ) ;
#28115 = FACE_OUTER_BOUND ( 'NONE', #38053, .T. ) ;
#28116 = CARTESIAN_POINT ( 'NONE',  ( 24.56079138214657931, 2.730512922303396817, -3.879043415943517203 ) ) ;
#28117 = ORIENTED_EDGE ( 'NONE', *, *, #23641, .T. ) ;
#28118 = ORIENTED_EDGE ( 'NONE', *, *, #26938, .F. ) ;
#28119 = CARTESIAN_POINT ( 'NONE',  ( 67.01285850879368411, 57.98447793263278527, 3.999354069328931782 ) ) ;
#28120 = CARTESIAN_POINT ( 'NONE',  ( 21.35934345986309069, 3.587023842369657878, 3.540040143219671531 ) ) ;
#28121 = CARTESIAN_POINT ( 'NONE',  ( 4.960724736016636882, -30.80272740983260604, 7.785096263473211486 ) ) ;
#28122 = CARTESIAN_POINT ( 'NONE',  ( 88.36353413610991936, -2.347965962749813063, -0.8794284646705250452 ) ) ;
#28123 = CARTESIAN_POINT ( 'NONE',  ( 35.48404000816106674, -1.920476918020975754, -5.744540646660859728 ) ) ;
#28124 =( BOUNDED_CURVE ( )  B_SPLINE_CURVE ( 3, ( #6966, #39039, #16424, #4494 ),
 .UNSPECIFIED., .F., .T. ) 
 B_SPLINE_CURVE_WITH_KNOTS ( ( 4, 4 ),
 ( 1.381924640371167579, 1.574767692156076260 ),
 .UNSPECIFIED. ) 
 CURVE ( )  GEOMETRIC_REPRESENTATION_ITEM ( )  RATIONAL_B_SPLINE_CURVE ( ( 1.000000000000000000, 0.9969033633783032089, 0.9969033633783032089, 1.000000000000000000 ) ) 
 REPRESENTATION_ITEM ( '' )  );
#28125 = VECTOR ( 'NONE', #11004, 1000.000000000000000 ) ;
#28126 = ORIENTED_EDGE ( 'NONE', *, *, #8300, .T. ) ;
#28127 = CARTESIAN_POINT ( 'NONE',  ( 25.60585682308668964, 2.174458409923740287, 4.126442313751081059 ) ) ;
#28128 = CARTESIAN_POINT ( 'NONE',  ( 0.000000000000000000, 0.000000000000000000, 0.000000000000000000 ) ) ;
#28129 = CARTESIAN_POINT ( 'NONE',  ( -70.92837670882201451, -21.78299143689573469, 6.000000000001379341 ) ) ;
#28130 = ORIENTED_EDGE ( 'NONE', *, *, #39302, .T. ) ;
#28131 = CARTESIAN_POINT ( 'NONE',  ( -42.44874870218064444, -25.49307895267003587, 6.700000000000000178 ) ) ;
#28132 = EDGE_CURVE ( 'NONE', #17194, #2391, #16239, .T. ) ;
#28133 = EDGE_LOOP ( 'NONE', ( #34846, #14266, #4738, #15157 ) ) ;
#28134 = CARTESIAN_POINT ( 'NONE',  ( 78.75315097705549761, 65.71977079011871581, -2.326060681237740013 ) ) ;
#28135 = CARTESIAN_POINT ( 'NONE',  ( -1.697580213352021250, -29.45244296570870901, 7.759451378593097637 ) ) ;
#28136 = AXIS2_PLACEMENT_3D ( 'NONE', #16859, #13582, #33350 ) ;
#28137 = CARTESIAN_POINT ( 'NONE',  ( 79.25608414939210888, 65.04333590781634200, 3.260928702718600469 ) ) ;
#28139 = ORIENTED_EDGE ( 'NONE', *, *, #9483, .F. ) ;
#28138 = DIRECTION ( 'NONE',  ( 0.000000000000000000, 0.000000000000000000, 1.000000000000000000 ) ) ;
#28140 = CARTESIAN_POINT ( 'NONE',  ( 0.009528945288370773911, -26.52245690844340231, 7.785593909369613819 ) ) ;
#28142 = CARTESIAN_POINT ( 'NONE',  ( 23.06594672544511582, -8.086844732617873177, 2.500000000000001332 ) ) ;
#28141 = DIRECTION ( 'NONE',  ( 1.000000000000000000, 0.000000000000000000, 0.000000000000000000 ) ) ;
#28143 = CARTESIAN_POINT ( 'NONE',  ( -63.99293516169446150, 35.89893413629672381, -7.506047544094577084 ) ) ;
#28144 = CARTESIAN_POINT ( 'NONE',  ( 33.89863206464382017, -5.476329442118064605, -0.1430302926928115892 ) ) ;
#28145 = CARTESIAN_POINT ( 'NONE',  ( 22.61884710626975092, 4.600495562082832279, -3.071470106280676404 ) ) ;
#28146 = ORIENTED_EDGE ( 'NONE', *, *, #34910, .F. ) ;
#28147 = CARTESIAN_POINT ( 'NONE',  ( -63.58520484588294153, 35.72026407271188475, -7.000000000000000888 ) ) ;
#28148 = CARTESIAN_POINT ( 'NONE',  ( 24.23947115566313926, 0.8503125907183233245, 6.739520400040675874 ) ) ;
#28149 = CARTESIAN_POINT ( 'NONE',  ( -75.99771073292856727, -5.502405136523671025, -8.621866671386070990 ) ) ;
#28150 = CARTESIAN_POINT ( 'NONE',  ( 5.012588991809223238, -30.33765636181075109, 6.887945620086120435 ) ) ;
#28151 = CARTESIAN_POINT ( 'NONE',  ( 81.11561130678133225, 63.91242180912993831, 3.402511877379639227 ) ) ;
#28152 = CARTESIAN_POINT ( 'NONE',  ( 84.32222422711384979, 2.914578286995431977, 1.930349914595605343 ) ) ;
#28153 = CARTESIAN_POINT ( 'NONE',  ( 14.96986543946197479, 12.33094088818544698, 2.523832330313138250 ) ) ;
#28154 = VERTEX_POINT ( 'NONE', #16993 ) ;
#28155 = FACE_OUTER_BOUND ( 'NONE', #19503, .T. ) ;
#28156 = CARTESIAN_POINT ( 'NONE',  ( 4.584375091198674035, -31.37066225182081425, 7.759451378593099413 ) ) ;
#28157 = EDGE_CURVE ( 'NONE', #12484, #24796, #13916, .T. ) ;
#28158 = CARTESIAN_POINT ( 'NONE',  ( 4.094185015697331842, -27.01655085626599018, 6.961115707816238896 ) ) ;
#28159 = CARTESIAN_POINT ( 'NONE',  ( 31.38401102386968589, -3.643146459872906195, -4.878133479856779253 ) ) ;
#28160 = CARTESIAN_POINT ( 'NONE',  ( 34.92827436638099670, -1.713443684080601992, -5.657799977018275861 ) ) ;
#28161 = FACE_OUTER_BOUND ( 'NONE', #18853, .T. ) ;
#28162 = ORIENTED_EDGE ( 'NONE', *, *, #7495, .F. ) ;
#28163 = CARTESIAN_POINT ( 'NONE',  ( 29.10048579223744980, 0.3561570061246891461, 4.748232624423857295 ) ) ;
#28164 = EDGE_CURVE ( 'NONE', #22409, #13396, #2452, .T. ) ;
#28165 = CARTESIAN_POINT ( 'NONE',  ( 86.80434382515846892, 0.8549656295913086179, -5.002690157204635391 ) ) ;
#28166 = ORIENTED_EDGE ( 'NONE', *, *, #39181, .F. ) ;
#28168 = DIRECTION ( 'NONE',  ( 0.000000000000000000, 0.000000000000000000, -1.000000000000000000 ) ) ;
#28167 = CARTESIAN_POINT ( 'NONE',  ( 80.49748116766497219, 63.97695225015618803, -3.602832836245128956 ) ) ;
#28169 = CARTESIAN_POINT ( 'NONE',  ( -69.61748845350692250, -47.87187071230540170, 9.913994275702524561 ) ) ;
#28170 = CARTESIAN_POINT ( 'NONE',  ( 2.930077627932792250, -32.84679970447462694, 7.678495282201405203 ) ) ;
#28171 = ORIENTED_EDGE ( 'NONE', *, *, #19193, .F. ) ;
#28172 = CARTESIAN_POINT ( 'NONE',  ( 25.89164700572842293, -5.102322433750814845, -3.184945769527233850 ) ) ;
#28173 = ORIENTED_EDGE ( 'NONE', *, *, #345, .T. ) ;
#28174 = CARTESIAN_POINT ( 'NONE',  ( -80.90861860399088812, 11.45717611192839591, 0.6283086135788885640 ) ) ;
#28175 = EDGE_LOOP ( 'NONE', ( #1228, #27343, #3060 ) ) ;
#28176 = ADVANCED_FACE ( 'NONE', ( #26488 ), #610, .F. ) ;
#28177 = CARTESIAN_POINT ( 'NONE',  ( 79.27128227901765456, 65.37053819277495847, -2.988136994358709497 ) ) ;
#28178 = CARTESIAN_POINT ( 'NONE',  ( 35.63425396194121220, -3.169062201350007157, 5.767985167086449927 ) ) ;
#28179 = EDGE_LOOP ( 'NONE', ( #20218, #35226, #23458, #5363 ) ) ;
#28181 = DIRECTION ( 'NONE',  ( 1.000000000000000000, 8.966158204770716457E-16, 0.000000000000000000 ) ) ;
#28180 = CARTESIAN_POINT ( 'NONE',  ( 22.68890514319382135, 2.782549721596407455, 4.545382121805146447 ) ) ;
#28182 = ORIENTED_EDGE ( 'NONE', *, *, #37239, .T. ) ;
#28183 = CARTESIAN_POINT ( 'NONE',  ( 78.68884106766326170, 66.05749720280910253, -1.041818241550652724 ) ) ;
#28184 = DIRECTION ( 'NONE',  ( -0.000000000000000000, -0.000000000000000000, 1.000000000000000000 ) ) ;
#28186 = PLANE ( 'NONE',  #32178 ) ;
#28185 = CARTESIAN_POINT ( 'NONE',  ( 4.882868366733327470, -28.37333834040810032, 7.695279973900954751 ) ) ;
#28187 = CARTESIAN_POINT ( 'NONE',  ( 5.913338541744446175, -28.86358524566460915, 7.695279973900954751 ) ) ;
#28188 = CARTESIAN_POINT ( 'NONE',  ( -64.08758708074093136, 41.64075302466238071, -2.960467338825643058 ) ) ;
#28189 = CARTESIAN_POINT ( 'NONE',  ( 73.78163614357571021, 59.18917187859454998, 3.552420216828422017 ) ) ;
#28190 = CARTESIAN_POINT ( 'NONE',  ( 24.18717966629001737, 2.859004644576334631, -3.837239278320205838 ) ) ;
#28191 = EDGE_LOOP ( 'NONE', ( #23911, #21135, #29154, #1715 ) ) ;
#28192 = ADVANCED_FACE ( 'NONE', ( #9571, #21733 ), #12657, .T. ) ;
#28193 = CARTESIAN_POINT ( 'NONE',  ( 21.85643539959776760, 10.44946649885084966, 7.640826779728119078 ) ) ;
#28194 = CARTESIAN_POINT ( 'NONE',  ( 3.439741984728057478, -26.53271409599866715, 7.756742906098588186 ) ) ;
#28195 = EDGE_LOOP ( 'NONE', ( #28404, #14465, #15213, #39292, #29126 ) ) ;
#28196 = CARTESIAN_POINT ( 'NONE',  ( -77.95330471031414277, 33.71485196875532608, 12.49999999999999645 ) ) ;
#28197 = CARTESIAN_POINT ( 'NONE',  ( 81.54961753534279012, 61.59690320141231723, 1.551099981298355468 ) ) ;
#28198 = CARTESIAN_POINT ( 'NONE',  ( 85.12050554930138446, 2.746332700819607453, -1.966258668667607123 ) ) ;
#28199 = EDGE_LOOP ( 'NONE', ( #30677, #4735, #24313, #20429 ) ) ;
#28200 = CARTESIAN_POINT ( 'NONE',  ( 0.5426199015143727822, -32.76674687291834687, 7.763628509615287498 ) ) ;
#28201 = CARTESIAN_POINT ( 'NONE',  ( 18.27257696809985177, -3.066843069763234286, 3.029022186580533127 ) ) ;
#28202 = VECTOR ( 'NONE', #37001, 1000.000000000000000 ) ;
#28203 = CARTESIAN_POINT ( 'NONE',  ( 29.10272931528550799, 0.3625471829554103298, -4.748582780455301133 ) ) ;
#28204 = CARTESIAN_POINT ( 'NONE',  ( -12.99139449055068596, 10.37661300689600097, 2.500000000000000000 ) ) ;
#28205 = CARTESIAN_POINT ( 'NONE',  ( -28.97867591359219475, -24.55319635012989110, 6.800000000000000711 ) ) ;
#28206 = EDGE_CURVE ( 'NONE', #9863, #11496, #40438, .T. ) ;
#28207 = EDGE_CURVE ( 'NONE', #24466, #13676, #31016, .T. ) ;
#28208 = EDGE_CURVE ( 'NONE', #23822, #25264, #24405, .T. ) ;
#28209 = CARTESIAN_POINT ( 'NONE',  ( -1.225953191357326277, -31.30097466021442187, 7.695279973900954751 ) ) ;
#28210 = ORIENTED_EDGE ( 'NONE', *, *, #8857, .F. ) ;
#28211 = VERTEX_POINT ( 'NONE', #18838 ) ;
#28212 = CARTESIAN_POINT ( 'NONE',  ( 25.73261264963540995, 2.635811757010384504, 3.523854048240384618 ) ) ;
#28213 = CARTESIAN_POINT ( 'NONE',  ( -38.24874870218063450, -26.64985754041175525, 6.700000000000000178 ) ) ;
#28214 = ORIENTED_EDGE ( 'NONE', *, *, #4793, .T. ) ;
#28215 = CARTESIAN_POINT ( 'NONE',  ( 66.59136238364995108, 57.77385624644436746, -3.999229419681933351 ) ) ;
#28216 = CARTESIAN_POINT ( 'NONE',  ( 87.69516453960757474, -2.233259521322014329, -2.657756335895389288 ) ) ;
#28217 = CIRCLE ( 'NONE', #10470, 7.999999999999992895 ) ;
#28218 = VERTEX_POINT ( 'NONE', #37363 ) ;
#28219 = CARTESIAN_POINT ( 'NONE',  ( -57.81912131869246707, 32.28080896713289860, 4.194423477175957871 ) ) ;
#28220 = CARTESIAN_POINT ( 'NONE',  ( -20.24874870218063805, -26.64985754041175525, 6.700000000000000178 ) ) ;
#28221 = DIRECTION ( 'NONE',  ( 1.000000000000000000, 0.000000000000000000, 0.000000000000000000 ) ) ;
#28222 = CARTESIAN_POINT ( 'NONE',  ( -65.15514661499977933, 34.97220226750606997, 6.888442104241535802 ) ) ;
#28223 = CARTESIAN_POINT ( 'NONE',  ( -74.03402466285142225, 19.33157623370699341, -8.800414904976364028 ) ) ;
#28224 = ORIENTED_EDGE ( 'NONE', *, *, #30609, .T. ) ;
#28225 = FACE_BOUND ( 'NONE', #14233, .T. ) ;
#28226 = CARTESIAN_POINT ( 'NONE',  ( -58.99872204295123623, 28.48507918597136523, -6.834244957304557389 ) ) ;
#28227 = EDGE_LOOP ( 'NONE', ( #34255, #24342 ) ) ;
#28228 = CARTESIAN_POINT ( 'NONE',  ( 22.39794005767262064, 4.875138222190518178, 3.100870480539395402 ) ) ;
#28229 = CARTESIAN_POINT ( 'NONE',  ( 80.00335259508500485, 66.34466434620085806, -1.325417871280742066 ) ) ;
#28230 = DIRECTION ( 'NONE',  ( 0.000000000000000000, 0.000000000000000000, -1.000000000000000000 ) ) ;
#28231 = CARTESIAN_POINT ( 'NONE',  ( 81.17223480711247419, 61.34085670634290466, 1.541060042019463561 ) ) ;
#28232 = VECTOR ( 'NONE', #14011, 999.9999999999998863 ) ;
#28233 = CARTESIAN_POINT ( 'NONE',  ( 2.963912204589347343, -26.41341833881434198, 7.768425012602590662 ) ) ;
#28234 = ORIENTED_EDGE ( 'NONE', *, *, #3997, .T. ) ;
#28235 = CARTESIAN_POINT ( 'NONE',  ( 76.75621762107158474, 64.55157797518407392, -2.701592190110922331 ) ) ;
#28236 = SHAPE_REPRESENTATION ( 'slotted cheese head screw_iso_ISO 1207 - M5 x 35 - 35N', ( #30744 ), #11005 ) ;
#28238 = CARTESIAN_POINT ( 'NONE',  ( 1.700390093233090871, -29.56993018339339940, 7.800000000000000711 ) ) ;
#28237 = CARTESIAN_POINT ( 'NONE',  ( 2.321451664048270302, -33.01438696571141662, 7.635761828346576685 ) ) ;
#28239 = CARTESIAN_POINT ( 'NONE',  ( 16.69750073655492528, 9.540205430295099376, -2.812446839157479506 ) ) ;
#28240 = CARTESIAN_POINT ( 'NONE',  ( 81.39824655423379340, 62.07766870923514801, -2.596981798947365583 ) ) ;
#28241 = CARTESIAN_POINT ( 'NONE',  ( 78.51266523469810465, 61.01400193535553029, 3.220231295875823463 ) ) ;
#28242 = VERTEX_POINT ( 'NONE', #31207 ) ;
#28243 = VERTEX_POINT ( 'NONE', #15132 ) ;
#28244 = EDGE_CURVE ( 'NONE', #35733, #3023, #27688, .T. ) ;
#28245 = FACE_OUTER_BOUND ( 'NONE', #38882, .T. ) ;
#28246 = DIRECTION ( 'NONE',  ( 1.000000000000000000, 0.000000000000000000, 0.000000000000000000 ) ) ;
#28247 = CARTESIAN_POINT ( 'NONE',  ( 79.56604632444089020, 66.26916991809642354, 1.539394129974047676 ) ) ;
#28249 = CARTESIAN_POINT ( 'NONE',  ( -1.699007393330835392, -29.50544089494019673, 6.880147297696982633 ) ) ;
#28248 = DIRECTION ( 'NONE',  ( 0.000000000000000000, 0.000000000000000000, -1.000000000000000000 ) ) ;
#28250 = CARTESIAN_POINT ( 'NONE',  ( 30.28570682881508702, -1.586248365680131167, -6.023113166707004140 ) ) ;
#28251 = CARTESIAN_POINT ( 'NONE',  ( 2.170460981197068762, -32.93727830324805694, 7.754798119455333705 ) ) ;
#28252 = CARTESIAN_POINT ( 'NONE',  ( 30.10852511091080430, -6.281056253467228956, 2.499999999999994671 ) ) ;
#28253 = CARTESIAN_POINT ( 'NONE',  ( -64.17943696418036836, 35.01970154838168980, 4.761094547372117347 ) ) ;
#28254 = CARTESIAN_POINT ( 'NONE',  ( 23.59795352485724962, 0.4334124443017954853, -5.517309192317882527 ) ) ;
#28255 = EDGE_CURVE ( 'NONE', #31660, #7424, #26126, .T. ) ;
#28256 = CIRCLE ( 'NONE', #40092, 1.000000000000002220 ) ;
#28257 = CARTESIAN_POINT ( 'NONE',  ( 1.664433243520564654, -26.07011488755866679, 7.695279973900954751 ) ) ;
#28258 = CARTESIAN_POINT ( 'NONE',  ( 1.664433243520564654, -26.07011488755866679, 7.701614758090453705 ) ) ;
#28259 = DIRECTION ( 'NONE',  ( -0.1736481776669206722, -0.9848077530122096857, -0.000000000000000000 ) ) ;
#28260 = ADVANCED_FACE ( 'NONE', ( #18009, #15547 ), #37762, .F. ) ;
#28261 = FACE_OUTER_BOUND ( 'NONE', #26837, .T. ) ;
#28262 = CARTESIAN_POINT ( 'NONE',  ( 20.85070742889012152, 4.522926380425460025, -2.940039916530858832 ) ) ;
#28263 = FACE_OUTER_BOUND ( 'NONE', #5147, .T. ) ;
#28264 = CARTESIAN_POINT ( 'NONE',  ( -17.69482985384421880, -42.37473357531882101, 2.500000000000000000 ) ) ;
#28265 = CARTESIAN_POINT ( 'NONE',  ( 0.4969225441612274974, -32.85060279565202990, 7.773839561854630098 ) ) ;
#28266 = CARTESIAN_POINT ( 'NONE',  ( 17.04338035915418459, 48.81061067247630092, 4.000000000000000000 ) ) ;
#28267 = EDGE_CURVE ( 'NONE', #35921, #17878, #14258, .T. ) ;
#28268 = PLANE ( 'NONE',  #8312 ) ;
#28269 = CARTESIAN_POINT ( 'NONE',  ( 22.56436664557526584, -9.049820346388647962, 2.499999999999999112 ) ) ;
#28270 = AXIS2_PLACEMENT_3D ( 'NONE', #8069, #17527, #11759 ) ;
#28271 = CARTESIAN_POINT ( 'NONE',  ( -1.513482870951689430, -30.67944384715880091, 6.887041543973314361 ) ) ;
#28272 = ORIENTED_EDGE ( 'NONE', *, *, #3330, .T. ) ;
#28273 = ORIENTED_EDGE ( 'NONE', *, *, #3817, .F. ) ;
#28274 = FACE_OUTER_BOUND ( 'NONE', #9624, .T. ) ;
#28275 = EDGE_CURVE ( 'NONE', #13485, #21972, #11821, .T. ) ;
#28276 = CARTESIAN_POINT ( 'NONE',  ( 67.97136023280155825, 58.53559134324396496, -3.990965707299544363 ) ) ;
#28277 = B_SPLINE_CURVE_WITH_KNOTS ( 'NONE', 3,
 ( #19668, #28731, #25438, #738, #9580, #16363 ),
 .UNSPECIFIED., .F., .F.,
 ( 4, 2, 4 ),
 ( 0.000000000000000000, 0.0003568402636276586356, 0.0007136805272553172711 ),
 .UNSPECIFIED. ) ;
#28278 = CARTESIAN_POINT ( 'NONE',  ( 2.966849565284320978, -26.30708134228679640, 6.867280401193709416 ) ) ;
#28279 = ORIENTED_EDGE ( 'NONE', *, *, #9333, .T. ) ;
#28280 = DIRECTION ( 'NONE',  ( -1.000000000000000000, 0.000000000000000000, 0.000000000000000000 ) ) ;
#28281 = DIRECTION ( 'NONE',  ( 0.000000000000000000, 0.000000000000000000, 1.000000000000000000 ) ) ;
#28282 = CARTESIAN_POINT ( 'NONE',  ( 3.483130834601454229, -26.55797363598811245, 6.887161170156904433 ) ) ;
#28283 = DIRECTION ( 'NONE',  ( 0.000000000000000000, 0.000000000000000000, 1.000000000000000000 ) ) ;
#28284 = VERTEX_POINT ( 'NONE', #25027 ) ;
#28285 = CARTESIAN_POINT ( 'NONE',  ( 23.14409375757164256, 4.053802376405804431, 3.062998084521663333 ) ) ;
#28286 = DIRECTION ( 'NONE',  ( 0.000000000000000000, 0.000000000000000000, 1.000000000000000000 ) ) ;
#28287 = ORIENTED_EDGE ( 'NONE', *, *, #18209, .F. ) ;
#28288 = CARTESIAN_POINT ( 'NONE',  ( 4.666500650180242182, -31.42793668606411117, 7.750000000000000888 ) ) ;
#28289 = ORIENTED_EDGE ( 'NONE', *, *, #38773, .F. ) ;
#28290 = CARTESIAN_POINT ( 'NONE',  ( 78.44523713320049296, 65.65863411530537519, -2.218931858625903697 ) ) ;
#28292 = CARTESIAN_POINT ( 'NONE',  ( -7.078675913592194391, -24.55319635012989110, 6.700000000000000178 ) ) ;
#28291 = CARTESIAN_POINT ( 'NONE',  ( 23.62020001075898179, 0.4737404876348103588, 5.490607732800076413 ) ) ;
#28293 = CARTESIAN_POINT ( 'NONE',  ( 79.54388053879580411, 66.09379204087656490, -2.134710458528699561 ) ) ;
#28294 = CARTESIAN_POINT ( 'NONE',  ( 80.53617040090055923, 61.82406284986342371, 2.948506306558747347 ) ) ;
#28295 = ORIENTED_EDGE ( 'NONE', *, *, #117, .T. ) ;
#28296 = EDGE_CURVE ( 'NONE', #1666, #37345, #37562, .T. ) ;
#28297 = CIRCLE ( 'NONE', #13840, 5.329987104167474676 ) ;
#28298 = CARTESIAN_POINT ( 'NONE',  ( 80.38645948019593845, 66.31981033314002616, 1.000000000000000000 ) ) ;
#28300 = VERTEX_POINT ( 'NONE', #8741 ) ;
#28299 = CARTESIAN_POINT ( 'NONE',  ( 2.868360829923958022, -32.76303417817520369, 7.763628509615287498 ) ) ;
#28301 = CARTESIAN_POINT ( 'NONE',  ( 21.85643539959777470, -4.742028430345498258, -11.91557605213902882 ) ) ;
#28302 = CARTESIAN_POINT ( 'NONE',  ( -11.07867591359219794, -26.64985754041175525, 6.700000000000000178 ) ) ;
#28303 = ORIENTED_EDGE ( 'NONE', *, *, #7385, .T. ) ;
#28304 = CARTESIAN_POINT ( 'NONE',  ( -77.44400633864859174, 9.722113372229207684, 9.166479153956517578 ) ) ;
#28305 = CARTESIAN_POINT ( 'NONE',  ( 37.04442315954803178, -3.197375157205383456, 5.958390354492890673 ) ) ;
#28306 = VERTEX_POINT ( 'NONE', #21324 ) ;
#28307 = DIRECTION ( 'NONE',  ( -0.000000000000000000, 1.000000000000000000, -0.000000000000000000 ) ) ;
#28308 = EDGE_LOOP ( 'NONE', ( #17024, #22325, #6319, #27814 ) ) ;
#28309 = CARTESIAN_POINT ( 'NONE',  ( -54.01549048184568846, -30.38627270959228710, -4.152976064860135708 ) ) ;
#28310 = CARTESIAN_POINT ( 'NONE',  ( 30.68983369444830345, -3.022615581088325509, -4.996288803099273146 ) ) ;
#28311 = CARTESIAN_POINT ( 'NONE',  ( 33.94754086493713174, -0.4854118941598933867, -5.118189633504289127 ) ) ;
#28312 = CARTESIAN_POINT ( 'NONE',  ( 1.700390093233090871, -29.56993018339339940, -8.199999999999999289 ) ) ;
#28313 = CARTESIAN_POINT ( 'NONE',  ( 3.733834482138272737, -32.29483457019856019, 6.903372536218459032 ) ) ;
#28314 = CARTESIAN_POINT ( 'NONE',  ( 19.11796579935018059, 7.216354979127149960, 3.190218951375439982 ) ) ;
#28315 = DIRECTION ( 'NONE',  ( 0.000000000000000000, 0.000000000000000000, 1.000000000000000000 ) ) ;
#28316 = CARTESIAN_POINT ( 'NONE',  ( 29.63236135128273929, -3.802766571116140248, 4.424495427163341432 ) ) ;
#28317 = LINE ( 'NONE', #16167, #35524 ) ;
#28318 = EDGE_CURVE ( 'NONE', #28942, #20340, #36900, .T. ) ;
#28319 = AXIS2_PLACEMENT_3D ( 'NONE', #228, #9891, #13184 ) ;
#28320 = ADVANCED_FACE ( 'NONE', ( #21940, #30808 ), #12029, .F. ) ;
#28321 = DIRECTION ( 'NONE',  ( 0.6751708784618154491, -0.7376613619250370624, 0.000000000000000000 ) ) ;
#28322 = CARTESIAN_POINT ( 'NONE',  ( 25.02876953629550272, 1.120990461282832751, -4.601145122132357379 ) ) ;
#28323 = CARTESIAN_POINT ( 'NONE',  ( 32.15421574055506682, -3.772606034914804951, -4.832894874862167178 ) ) ;
#28324 = EDGE_CURVE ( 'NONE', #14526, #24466, #4966, .T. ) ;
#28325 = CARTESIAN_POINT ( 'NONE',  ( 26.61849259059863826, 1.625058386879766559, -4.334342491016723642 ) ) ;
#28326 = EDGE_LOOP ( 'NONE', ( #16737, #27362, #11241, #4842 ) ) ;
#28327 = CARTESIAN_POINT ( 'NONE',  ( 67.06698855917106528, 57.83491659372258908, 3.993952884371010814 ) ) ;
#28328 = CARTESIAN_POINT ( 'NONE',  ( 36.98982775529254496, -2.542815128719615014, 5.977429629229624730 ) ) ;
#28329 = CARTESIAN_POINT ( 'NONE',  ( 2.187796539937281182, -33.03559314236433408, 7.754798119455333705 ) ) ;
#28330 = CARTESIAN_POINT ( 'NONE',  ( 87.91375683397511409, -1.031045523906674033, -4.794500835981626352 ) ) ;
#28331 = AXIS2_PLACEMENT_3D ( 'NONE', #2768, #15294, #30135 ) ;
#28332 = CARTESIAN_POINT ( 'NONE',  ( -1.796521113867400654, -29.56993018341788826, 7.767301406056523305 ) ) ;
#28333 = VERTEX_POINT ( 'NONE', #13467 ) ;
#28334 = CARTESIAN_POINT ( 'NONE',  ( 25.35519752494395362, 2.304653593253668031, 4.072349217575649938 ) ) ;
#28335 =( NAMED_UNIT ( * ) SI_UNIT ( $, .STERADIAN. ) SOLID_ANGLE_UNIT ( ) );
#28336 = DIRECTION ( 'NONE',  ( 0.9999026450364576490, 0.01395351027862084051, 0.000000000000000000 ) ) ;
#28337 = DIRECTION ( 'NONE',  ( 0.7660444431189770143, 0.6427876096865404731, -0.000000000000000000 ) ) ;
#28338 = ORIENTED_EDGE ( 'NONE', *, *, #5120, .F. ) ;
#28339 = CARTESIAN_POINT ( 'NONE',  ( 0.000000000000000000, 13.37661300689600097, 2.500000000000000000 ) ) ;
#28340 = DIRECTION ( 'NONE',  ( 0.000000000000000000, -0.000000000000000000, -1.000000000000000000 ) ) ;
#28341 = ORIENTED_EDGE ( 'NONE', *, *, #10410, .T. ) ;
#28342 = CARTESIAN_POINT ( 'NONE',  ( 80.23164863168994998, 63.12273326640273297, -3.657510014241807106 ) ) ;
#28343 = CARTESIAN_POINT ( 'NONE',  ( -70.92837670882107659, -23.80776546975053165, 0.000000000000000000 ) ) ;
#28344 = CARTESIAN_POINT ( 'NONE',  ( 80.00230669363345726, 63.71856487089239351, 3.706996517075249908 ) ) ;
#28347 = ORIENTED_EDGE ( 'NONE', *, *, #7073, .T. ) ;
#28346 = ORIENTED_EDGE ( 'NONE', *, *, #28318, .F. ) ;
#28345 = CARTESIAN_POINT ( 'NONE',  ( 14.74516149782244057, 13.12656125137344532, 2.499999999999999556 ) ) ;
#28348 = AXIS2_PLACEMENT_3D ( 'NONE', #2139, #14867, #1186 ) ;
#28349 = B_SPLINE_CURVE_WITH_KNOTS ( 'NONE', 3,
 ( #22401, #34970, #19295, #31865, #3678, #16203, #27642, #8693, #7537, #30757, #1191, #17542, #32467, #21069, #14871, #27443, #29371, #8488, #40198, #10616, #21273, #18165, #33845, #33643, #20644, #36506, #4267, #5623, #27038, #5418, #2352 ),
 .UNSPECIFIED., .F., .F.,
 ( 4, 3, 3, 3, 3, 3, 3, 3, 3, 3, 4 ),
 ( 3.885015761172426832E-18, 3.077658087705615681E-05, 6.152638666998687552E-05, 9.267501192706369616E-05, 0.0001241882240135191984, 0.0001556618703051669626, 0.0001866161554452214634, 0.0002167966385860943524, 0.0002463805737537729358, 0.0002758761370306496170, 0.0002847094172290017965 ),
 .UNSPECIFIED. ) ;
#28350 = FACE_OUTER_BOUND ( 'NONE', #24817, .T. ) ;
#28351 = DIRECTION ( 'NONE',  ( -0.000000000000000000, -0.000000000000000000, -1.000000000000000000 ) ) ;
#28352 = DIRECTION ( 'NONE',  ( 0.9848077530122081313, 0.1736481776669300814, 0.000000000000000000 ) ) ;
#28353 = CARTESIAN_POINT ( 'NONE',  ( 11.29080664838498649, 1.564594260697056104E-15, 6.000000000000000000 ) ) ;
#28354 = CARTESIAN_POINT ( 'NONE',  ( 22.38437366705409204, 4.924138827339338498, -3.063762403727182448 ) ) ;
#28355 = EDGE_LOOP ( 'NONE', ( #15691, #12846, #18862, #11818 ) ) ;
#28356 = LINE ( 'NONE', #3474, #22886 ) ;
#28357 = B_SPLINE_CURVE_WITH_KNOTS ( 'NONE', 3,
 ( #5306, #39265, #39060, #4511, #11056, #20527 ),
 .UNSPECIFIED., .F., .F.,
 ( 4, 2, 4 ),
 ( 8.484391014525137476E-05, 0.003152276965141869499, 0.006219710020138487054 ),
 .UNSPECIFIED. ) ;
#28358 = CARTESIAN_POINT ( 'NONE',  ( 5.686407058211319310, -26.27220315192986888, 7.695279973900954751 ) ) ;
#28359 = CARTESIAN_POINT ( 'NONE',  ( -1.656077431862442717, -30.11226380117775037, 6.894806418505347700 ) ) ;
#28360 = CARTESIAN_POINT ( 'NONE',  ( -76.83524845872202036, -4.539336671474099028, -9.585163668414178773 ) ) ;
#28361 = CARTESIAN_POINT ( 'NONE',  ( -70.92837670882107659, -23.80776546975053520, 0.000000000000000000 ) ) ;
#28362 = CARTESIAN_POINT ( 'NONE',  ( 81.27686174477064185, 61.37652599617184990, 1.416821487223855813 ) ) ;
#28363 = CARTESIAN_POINT ( 'NONE',  ( 87.88829317789571860, -2.466143857431153830, 1.215092630805642671 ) ) ;
#28364 = DIRECTION ( 'NONE',  ( 0.000000000000000000, 1.000000000000000000, 0.000000000000000000 ) ) ;
#28365 = ORIENTED_EDGE ( 'NONE', *, *, #28912, .T. ) ;
#28366 = CARTESIAN_POINT ( 'NONE',  ( 2.863609035986292461, -26.26888160889163615, 7.686927408461905031 ) ) ;
#28367 = CARTESIAN_POINT ( 'NONE',  ( 25.01357312920399778, 3.324376023134533842, -1.959542026491533750 ) ) ;
#28368 = ORIENTED_EDGE ( 'NONE', *, *, #30981, .T. ) ;
#28369 = EDGE_CURVE ( 'NONE', #20410, #38669, #728, .T. ) ;
#28370 = CARTESIAN_POINT ( 'NONE',  ( 4.059384891591554911, -26.98436573025793095, 6.875780273367531059 ) ) ;
#28371 = ADVANCED_FACE ( 'NONE', ( #7292 ), #15952, .F. ) ;
#28372 = CARTESIAN_POINT ( 'NONE',  ( -70.92837670882107659, -27.85319909218681644, 0.000000000000000000 ) ) ;
#28373 = CARTESIAN_POINT ( 'NONE',  ( 30.19003827612802482, -2.952522945788203845, 4.918283640461378781 ) ) ;
#28374 =( BOUNDED_CURVE ( )  B_SPLINE_CURVE ( 3, ( #38792, #4824, #26453, #20660 ),
 .UNSPECIFIED., .F., .T. ) 
 B_SPLINE_CURVE_WITH_KNOTS ( ( 4, 4 ),
 ( 1.381924640371167801, 1.574767692156075372 ),
 .UNSPECIFIED. ) 
 CURVE ( )  GEOMETRIC_REPRESENTATION_ITEM ( )  RATIONAL_B_SPLINE_CURVE ( ( 1.000000000000000000, 0.9969033633783033199, 0.9969033633783033199, 1.000000000000000000 ) ) 
 REPRESENTATION_ITEM ( '' )  );
#28375 = ORIENTED_EDGE ( 'NONE', *, *, #7794, .F. ) ;
#28376 = CARTESIAN_POINT ( 'NONE',  ( 34.77313873784321885, -3.161490297579837350, 5.633587310215530053 ) ) ;
#28377 = CARTESIAN_POINT ( 'NONE',  ( 87.92727933775610438, -0.4063688358931643041, -3.816426586085390760 ) ) ;
#28378 = ORIENTED_EDGE ( 'NONE', *, *, #29293, .T. ) ;
#28380 = CARTESIAN_POINT ( 'NONE',  ( -4.444218661349752963, -35.94265729135299381, -6.000000000000000000 ) ) ;
#28379 = CARTESIAN_POINT ( 'NONE',  ( 80.75501959326771839, 63.35152955421530407, -3.552238747020028953 ) ) ;
#28381 = CARTESIAN_POINT ( 'NONE',  ( -28.87867591359219333, -26.64985754041175525, 6.800000000000000711 ) ) ;
#28382 = CARTESIAN_POINT ( 'NONE',  ( -42.24874870218063450, -26.64985754041175525, 6.800000000000000711 ) ) ;
#28383 = VERTEX_POINT ( 'NONE', #35121 ) ;
#28384 = DIRECTION ( 'NONE',  ( 1.000000000000000000, 0.000000000000000000, 0.000000000000000000 ) ) ;
#28385 = EDGE_LOOP ( 'NONE', ( #11444, #6181, #17119, #40039, #18978 ) ) ;
#28386 = CARTESIAN_POINT ( 'NONE',  ( -79.57508400964319151, -6.640697488684422112, 5.040913395559038612 ) ) ;
#28387 = VECTOR ( 'NONE', #29017, 1000.000000000000000 ) ;
#28388 = ORIENTED_EDGE ( 'NONE', *, *, #1032, .T. ) ;
#28389 = CARTESIAN_POINT ( 'NONE',  ( 80.39050082614866710, 63.54812927569808778, -3.668443954219268832 ) ) ;
#28390 = CARTESIAN_POINT ( 'NONE',  ( 24.75830837035764276, 3.019210359990082804, 3.350572556515618583 ) ) ;
#28391 = EDGE_CURVE ( 'NONE', #13762, #19523, #16763, .T. ) ;
#28393 = CARTESIAN_POINT ( 'NONE',  ( 4.381563664431031846, -27.47916279290977570, 7.754798119455333705 ) ) ;
#28392 = CARTESIAN_POINT ( 'NONE',  ( 25.61003942877132289, 2.172251185455080780, 4.127339093466678044 ) ) ;
#28395 = ORIENTED_EDGE ( 'NONE', *, *, #8811, .T. ) ;
#28394 = ORIENTED_EDGE ( 'NONE', *, *, #31958, .T. ) ;
#28396 = CARTESIAN_POINT ( 'NONE',  ( 78.92300404249584744, 66.17133619070195039, -1.270639542487659535 ) ) ;
#28397 = LINE ( 'NONE', #25322, #5534 ) ;
#28399 = DIRECTION ( 'NONE',  ( 0.000000000000000000, 0.000000000000000000, 1.000000000000000000 ) ) ;
#28398 = PLANE ( 'NONE',  #13421 ) ;
#28400 = FACE_OUTER_BOUND ( 'NONE', #8210, .T. ) ;
#28401 = CARTESIAN_POINT ( 'NONE',  ( 0.6711941891205337463, -0.6000000000000004219, 3.974981096219152299 ) ) ;
#28402 = CARTESIAN_POINT ( 'NONE',  ( 71.32664523234116416, 58.52704510057537135, 3.775670717450666736 ) ) ;
#28403 = CARTESIAN_POINT ( 'NONE',  ( 22.19554510023723637, 4.144875652714271830, -3.913740728431892801 ) ) ;
#28404 = ORIENTED_EDGE ( 'NONE', *, *, #24687, .T. ) ;
#28405 = CARTESIAN_POINT ( 'NONE',  ( 21.85643539959774984, 10.28856666709980594, -7.862822601098399034 ) ) ;
#28406 = CARTESIAN_POINT ( 'NONE',  ( -58.72867408015306978, 29.68869064929980794, -5.572828569880161176 ) ) ;
#28407 = VERTEX_POINT ( 'NONE', #26250 ) ;
#28408 = CARTESIAN_POINT ( 'NONE',  ( 2.123610019918336089, -26.08872931251818983, 7.139344958878410807 ) ) ;
#28409 = CARTESIAN_POINT ( 'NONE',  ( 81.68586513309682573, 63.81782706256000637, 3.019849704268901647 ) ) ;
#28410 = CARTESIAN_POINT ( 'NONE',  ( 87.09859342968812257, 0.5244505078549105415, -5.068689133590885909 ) ) ;
#28411 = B_SPLINE_CURVE_WITH_KNOTS ( 'NONE', 3,
 ( #25591, #38135, #9936, #15710, #25185, #37716, #22517, #9523, #35084, #6859 ),
 .UNSPECIFIED., .F., .F.,
 ( 4, 3, 3, 4 ),
 ( 0.000000000000000000, 3.025505781527818361E-05, 6.051003801291508300E-05, 6.468145402690557617E-05 ),
 .UNSPECIFIED. ) ;
#28412 = ORIENTED_EDGE ( 'NONE', *, *, #22520, .F. ) ;
#28413 = LINE ( 'NONE', #12759, #9717 ) ;
#28414 = VERTEX_POINT ( 'NONE', #7095 ) ;
#28415 = CARTESIAN_POINT ( 'NONE',  ( 19.70671233036541281, -2.908903325760366698, 3.265966001044424249 ) ) ;
#28416 = EDGE_CURVE ( 'NONE', #29405, #28154, #13625, .T. ) ;
#28417 = CARTESIAN_POINT ( 'NONE',  ( 35.78597716193907274, -3.162283487670411120, -5.791665241885592508 ) ) ;
#28418 = CARTESIAN_POINT ( 'NONE',  ( -1.751698146652124866, -30.14706689514045479, 6.894806418505347700 ) ) ;
#28419 = CARTESIAN_POINT ( 'NONE',  ( -4.890026461918814071, -8.228598103685714525E-16, 6.000000000000000000 ) ) ;
#28420 = CARTESIAN_POINT ( 'NONE',  ( 4.404484264602725574, -31.79206310534561553, 7.698786668945011513 ) ) ;
#28421 = DIRECTION ( 'NONE',  ( -0.000000000000000000, -0.000000000000000000, -1.000000000000000000 ) ) ;
#28422 = VECTOR ( 'NONE', #16707, 1000.000000000000227 ) ;
#28423 = CARTESIAN_POINT ( 'NONE',  ( -1.268944822877880352, -31.22617634019398380, 7.785868773668303433 ) ) ;
#28424 = CARTESIAN_POINT ( 'NONE',  ( 29.47104931226115099, -2.981108624964739828, 4.806068023836186143 ) ) ;
#28425 = ORIENTED_EDGE ( 'NONE', *, *, #36472, .F. ) ;
#28426 = ORIENTED_EDGE ( 'NONE', *, *, #27748, .F. ) ;
#28427 = CARTESIAN_POINT ( 'NONE',  ( 36.71885878822434535, -3.457450448323470038, 5.861098606071526440 ) ) ;
#28428 = DIRECTION ( 'NONE',  ( -1.000000000000000000, 0.000000000000000000, 0.000000000000000000 ) ) ;
#28429 = EDGE_LOOP ( 'NONE', ( #10104, #17356, #25930, #35759 ) ) ;
#28430 = CARTESIAN_POINT ( 'NONE',  ( 66.56592146697632018, 57.84521198437244038, -3.999917672785076483 ) ) ;
#28431 = ORIENTED_EDGE ( 'NONE', *, *, #3762, .T. ) ;
#28432 = CARTESIAN_POINT ( 'NONE',  ( 87.86569408387285307, -0.3371933557188040997, -3.487338236652987700 ) ) ;
#28433 = CARTESIAN_POINT ( 'NONE',  ( 4.715819433959782536, -31.34677736058242559, 6.894806418505347700 ) ) ;
#28434 = CARTESIAN_POINT ( 'NONE',  ( 4.952701570995533764, -28.57870110776509875, 6.887945620086120435 ) ) ;
#28435 = CARTESIAN_POINT ( 'NONE',  ( -5.078675913592192614, -24.55319635012989110, 6.700000000000000178 ) ) ;
#28436 = ORIENTED_EDGE ( 'NONE', *, *, #4123, .F. ) ;
#28437 = FACE_BOUND ( 'NONE', #5334, .T. ) ;
#28438 = CARTESIAN_POINT ( 'NONE',  ( -70.92837670882107659, 28.72470171467712063, 0.000000000000000000 ) ) ;
#28439 = EDGE_LOOP ( 'NONE', ( #15613, #38444, #23831, #15219 ) ) ;
#28440 = CARTESIAN_POINT ( 'NONE',  ( 23.99719617098446989, 3.301072601594968070, 3.381232105112813358 ) ) ;
#28441 = CARTESIAN_POINT ( 'NONE',  ( 82.20671311902168554, 64.86843738523475622, -1.633153239555407144 ) ) ;
#28442 = CARTESIAN_POINT ( 'NONE',  ( 5.198120437317888864, -29.69595573662939358, 7.750000000000000888 ) ) ;
#28443 = CARTESIAN_POINT ( 'NONE',  ( 81.12024331894987483, 61.43208913379082503, 1.925402693829570300 ) ) ;
#28444 = CARTESIAN_POINT ( 'NONE',  ( -1.752498985642891860, -28.99760421947165057, 7.701614758090454593 ) ) ;
#28445 = ORIENTED_EDGE ( 'NONE', *, *, #14099, .F. ) ;
#28446 = CARTESIAN_POINT ( 'NONE',  ( 77.39092423430425072, 61.90746491491129433, -3.829716617890468022 ) ) ;
#28448 = CYLINDRICAL_SURFACE ( 'NONE', #15789, 0.09010775117052816086 ) ;
#28447 = CARTESIAN_POINT ( 'NONE',  ( -71.59377001835473209, -45.76911956692035943, 5.963683625267878874 ) ) ;
#28449 = CARTESIAN_POINT ( 'NONE',  ( 15.09416660562139789, 11.91275931974590030, -2.554301580912084368 ) ) ;
#28450 = EDGE_CURVE ( 'NONE', #14209, #40275, #7439, .T. ) ;
#28451 = CARTESIAN_POINT ( 'NONE',  ( 80.22001885188437598, 64.95903095167622610, -3.330128783915600632 ) ) ;
#28452 = CARTESIAN_POINT ( 'NONE',  ( 76.82516749139865908, 64.42394039557471785, 2.889099817377080548 ) ) ;
#28453 = VECTOR ( 'NONE', #25607, 1000.000000000000114 ) ;
#28454 = ORIENTED_EDGE ( 'NONE', *, *, #25349, .T. ) ;
#28455 = EDGE_CURVE ( 'NONE', #39647, #37652, #19050, .T. ) ;
#28456 = FACE_OUTER_BOUND ( 'NONE', #34958, .T. ) ;
#28457 = DIRECTION ( 'NONE',  ( 0.000000000000000000, -0.000000000000000000, -1.000000000000000000 ) ) ;
#28458 = CARTESIAN_POINT ( 'NONE',  ( 82.29876416100432834, 62.79692783100102105, 1.831286414254331030 ) ) ;
#28460 = CARTESIAN_POINT ( 'NONE',  ( 16.92333500577657190, 7.515569495004324807, 3.484773800360644991 ) ) ;
#28459 = FACE_OUTER_BOUND ( 'NONE', #23522, .T. ) ;
#28461 = CARTESIAN_POINT ( 'NONE',  ( 28.22557690513166762, 1.384627073958520249, -4.541740331631825001 ) ) ;
#28462 = DIRECTION ( 'NONE',  ( 0.000000000000000000, -0.000000000000000000, 1.000000000000000000 ) ) ;
#28463 = CARTESIAN_POINT ( 'NONE',  ( 4.890701645444022638, -28.39438256639548896, 7.635761828346577573 ) ) ;
#28464 = CARTESIAN_POINT ( 'NONE',  ( -64.12237394559150516, 36.72939681796538025, 5.075523754375453223 ) ) ;
#28465 = CYLINDRICAL_SURFACE ( 'NONE', #35992, 3.399999999999999911 ) ;
#28466 = CARTESIAN_POINT ( 'NONE',  ( -0.6250228819461873808, -32.05034436148299193, 7.013842709614101167 ) ) ;
#28467 = DIRECTION ( 'NONE',  ( 0.000000000000000000, 1.000000000000000000, 0.000000000000000000 ) ) ;
#28468 = CARTESIAN_POINT ( 'NONE',  ( -18.44874870218064089, -25.49307895267003587, 6.800000000000000711 ) ) ;
#28469 = EDGE_CURVE ( 'NONE', #18087, #713, #6898, .T. ) ;
#28470 = CARTESIAN_POINT ( 'NONE',  ( 36.15893501698462842, -3.359997738205348750, -5.843264819365881380 ) ) ;
#28471 = CARTESIAN_POINT ( 'NONE',  ( 80.84587339237160108, 61.18626677283346993, -1.559707275244749836 ) ) ;
#28472 = CARTESIAN_POINT ( 'NONE',  ( -0.9488855924148063004, -31.70099553385623992, 7.784476445165072533 ) ) ;
#28473 = CARTESIAN_POINT ( 'NONE',  ( 21.50460961888511946, -2.679762898963643281, -3.562712440612756826 ) ) ;
#28474 = CARTESIAN_POINT ( 'NONE',  ( 3.356636250033691482, -32.53926509950436952, 7.785868773668303433 ) ) ;
#28475 = CARTESIAN_POINT ( 'NONE',  ( -77.49308833732668234, 9.745258916933323690, 9.129529565702688032 ) ) ;
#28476 = CIRCLE ( 'NONE', #25189, 12.73502530973474300 ) ;
#28477 = FACE_OUTER_BOUND ( 'NONE', #11239, .T. ) ;
#28478 = CARTESIAN_POINT ( 'NONE',  ( -1.504465140167883019, -28.43462789667258406, 7.730758795053805699 ) ) ;
#28479 = CARTESIAN_POINT ( 'NONE',  ( 31.33294556979534917, -2.944313455537491464, 5.096661964955516488 ) ) ;
#28480 = ORIENTED_EDGE ( 'NONE', *, *, #27420, .T. ) ;
#28481 = B_SPLINE_CURVE_WITH_KNOTS ( 'NONE', 3,
 ( #31625, #5894, #3451, #5686, #18229, #34328, #2624, #15143, #27702, #40255, #12041, #15349, #18432, #31020, #2828, #40449, #12258, #24832, #37377, #9173, #21745, #6098, #948, #3645, #35340, #28734, #28939, #25849, #13082, #29141, #22969, #548, #22773, #32249, #4045, #19265, #10187, #35533, #16169, #13483, #7110, #13278, #3850, #25644, #19671, #742, #38384, #6715, #26057, #34937, #16560, #31831, #38588, #10394, #38187, #22370, #9990, #22569, #35137, #6911, #32042, #19469, #16368, #14368, #14562, #11881, #18063 ),
 .UNSPECIFIED., .F., .F.,
 ( 4, 2, 1, 1, 2, 2, 2, 1, 2, 2, 1, 2, 1, 2, 2, 1, 2, 1, 1, 2, 2, 1, 1, 2, 2, 1, 1, 2, 2, 1, 1, 2, 2, 2, 1, 1, 2, 2, 1, 1, 1, 2, 4 ),
 ( 0.1786650602234007013, 0.1800047485722283680, 0.1813444369210560347, 0.1840238136187113960, 0.1893825670140220629, 0.2001000738046433691, 0.2054588271999540083, 0.2067985155487815918, 0.2074683597231953835, 0.2081382038976091753, 0.2108175805952658133, 0.2215350873858937530, 0.2268938407812077229, 0.2295732174788646940, 0.2322525941765216650, 0.2429701009671495771, 0.2644051145484054288, 0.2751226213390333131, 0.2804813747343473107, 0.2811512189087614910, 0.2818210630831757268, 0.2831607514320052532, 0.2858401281296641949, 0.3072751417109392813, 0.3501451688734893430, 0.3715801824547648735, 0.3822976892454029718, 0.3836373775942326647, 0.3849770659430624686, 0.3876564426407219655, 0.3930151960360420138, 0.4358852231986006798, 0.5216252775237169015, 0.5644953046862750679, 0.5859303182675540400, 0.5886096949652139809, 0.5892795391396290494, 0.5899493833140440069, 0.5912890716628744769, 0.5966478250581968013, 0.6073653318488412278, 0.6931053861739944200, 0.8645854948243009153 ),
 .UNSPECIFIED. ) ;
#28482 = LINE ( 'NONE', #22526, #25789 ) ;
#28483 = CARTESIAN_POINT ( 'NONE',  ( 68.03141654933527604, 58.37504561612195886, -3.996230182412892074 ) ) ;
#28484 = CIRCLE ( 'NONE', #10709, 0.1000000000000028644 ) ;
#28485 = VERTEX_POINT ( 'NONE', #38371 ) ;
#28486 = CARTESIAN_POINT ( 'NONE',  ( -0.9039228576583087094, -27.23290037300662902, 7.761113333117551250 ) ) ;
#28487 = CARTESIAN_POINT ( 'NONE',  ( 0.08177934104577368191, -26.57991422468078824, 6.866852738645442322 ) ) ;
#28488 = CARTESIAN_POINT ( 'NONE',  ( 24.19994416937476700, 2.844775240750135215, 3.845692126280272571 ) ) ;
#28489 =( BOUNDED_CURVE ( )  B_SPLINE_CURVE ( 3, ( #2340, #27028, #12186, #5206 ),
 .UNSPECIFIED., .F., .F. ) 
 B_SPLINE_CURVE_WITH_KNOTS ( ( 4, 4 ),
 ( 1.347909859412854017, 1.534781240595299190 ),
 .UNSPECIFIED. ) 
 CURVE ( )  GEOMETRIC_REPRESENTATION_ITEM ( )  RATIONAL_B_SPLINE_CURVE ( ( 1.000000000000000000, 0.9970920404276226723, 0.9970920404276226723, 1.000000000000000000 ) ) 
 REPRESENTATION_ITEM ( '' )  );
#28490 = CARTESIAN_POINT ( 'NONE',  ( 1.216376417621422679, -26.20454968296333220, 7.768425012602591551 ) ) ;
#28491 = CARTESIAN_POINT ( 'NONE',  ( 5.054174351635810858, -30.12861716918250465, 7.721096864323902409 ) ) ;
#28492 = EDGE_LOOP ( 'NONE', ( #9057, #9797, #22684, #18245 ) ) ;
#28493 = CARTESIAN_POINT ( 'NONE',  ( 21.71163078881388486, 6.331898811992721754, 3.191961573981963340 ) ) ;
#28494 = DIRECTION ( 'NONE',  ( -0.000000000000000000, -0.000000000000000000, -1.000000000000000000 ) ) ;
#28495 = AXIS2_PLACEMENT_3D ( 'NONE', #3491, #31675, #19107 ) ;
#28496 = CARTESIAN_POINT ( 'NONE',  ( 0.6527267737179240914, -26.33536660093865578, 7.754798119455333705 ) ) ;
#28497 = ORIENTED_EDGE ( 'NONE', *, *, #19028, .T. ) ;
#28498 = CARTESIAN_POINT ( 'NONE',  ( 80.72640005664072760, 61.14345848406946260, -1.640065189519674060 ) ) ;
#28500 = DIRECTION ( 'NONE',  ( -0.000000000000000000, -0.000000000000000000, 1.000000000000000000 ) ) ;
#28499 = CARTESIAN_POINT ( 'NONE',  ( 22.69308311670009815, 0.3336789988226459558, 6.387223081350540177 ) ) ;
#28501 = CARTESIAN_POINT ( 'NONE',  ( 81.73261497063171532, 63.12224843555907938, -2.914706979937542020 ) ) ;
#28502 = CARTESIAN_POINT ( 'NONE',  ( 79.28407881342867825, 64.35615987108396041, 3.584461231902843714 ) ) ;
#28503 = ORIENTED_EDGE ( 'NONE', *, *, #10053, .F. ) ;
#28504 = EDGE_CURVE ( 'NONE', #26819, #19906, #34049, .T. ) ;
#28505 = VECTOR ( 'NONE', #31383, 1000.000000000000000 ) ;
#28506 = CARTESIAN_POINT ( 'NONE',  ( -1.627984416835427162, -30.65173788820889200, 7.754798119455333705 ) ) ;
#28508 = VERTEX_POINT ( 'NONE', #28514 ) ;
#28507 = CARTESIAN_POINT ( 'NONE',  ( 2.890739320099559695, -32.75474996909392189, 7.730758795053806587 ) ) ;
#28509 = CARTESIAN_POINT ( 'NONE',  ( 25.50874925706157725, -4.568791516319697266, 1.869930813790659618 ) ) ;
#28510 = ORIENTED_EDGE ( 'NONE', *, *, #12845, .F. ) ;
#28511 = CARTESIAN_POINT ( 'NONE',  ( -71.81805169721867799, 3.553745898376941437, 9.960391718072360234 ) ) ;
#28512 = CARTESIAN_POINT ( 'NONE',  ( 23.04769018874944919, 0.3307018522552950812, -5.968051205461429198 ) ) ;
#28513 = VERTEX_POINT ( 'NONE', #22957 ) ;
#28514 = CARTESIAN_POINT ( 'NONE',  ( -40.87867591359218977, -26.64985754041175525, 6.800000000000000711 ) ) ;
#28515 = ORIENTED_EDGE ( 'NONE', *, *, #20331, .T. ) ;
#28516 = DIRECTION ( 'NONE',  ( -0.7508067542896647018, -7.864283315039239776E-15, 0.6605219282605377940 ) ) ;
#28517 = CARTESIAN_POINT ( 'NONE',  ( 1.596524671759634195, -32.96835966857143774, 6.864651958020304257 ) ) ;
#28518 = CARTESIAN_POINT ( 'NONE',  ( 35.83241067984241113, -3.730005543395272571, -5.623145078173256373 ) ) ;
#28519 = CARTESIAN_POINT ( 'NONE',  ( -1.560415995823573931, -30.53281333591209545, 6.949473656533220911 ) ) ;
#28520 = DIRECTION ( 'NONE',  ( 1.682730792515357087E-16, -1.000000000000000000, 0.000000000000000000 ) ) ;
#28521 = CARTESIAN_POINT ( 'NONE',  ( 5.741588806061445283, -32.80189416861090024, 7.754798119455333705 ) ) ;
#28522 = CARTESIAN_POINT ( 'NONE',  ( 5.199130151573005953, -29.66439072687301959, 6.863805608295730387 ) ) ;
#28523 = PRODUCT_DEFINITION_SHAPE ( 'NONE', 'NONE',  #17491 ) ;
#28524 = DIRECTION ( 'NONE',  ( 0.4999999999999979461, 0.8660254037844397068, -0.000000000000000000 ) ) ;
#28525 = CARTESIAN_POINT ( 'NONE',  ( -72.84815947045233031, 2.429809908889422498, 10.96147798754374669 ) ) ;
#28526 = B_SPLINE_CURVE_WITH_KNOTS ( 'NONE', 3,
 ( #38627, #23193, #16791, #31866, #7538, #4077, #16591, #34971, #28774, #983, #35170, #581, #10426, #19296, #35569, #29372, #13728, #19897, #13120 ),
 .UNSPECIFIED., .F., .F.,
 ( 4, 3, 3, 3, 3, 3, 4 ),
 ( 9.697399036122160616E-19, 2.546128104244903007E-05, 5.711050680484518844E-05, 8.113074941676767392E-05, 0.0001053129305727209560, 0.0001360598016347318545, 0.0001612931755713721809 ),
 .UNSPECIFIED. ) ;
#28527 = CIRCLE ( 'NONE', #25911, 83.68529983683480111 ) ;
#28528 = CYLINDRICAL_SURFACE ( 'NONE', #2718, 0.1000000000000028644 ) ;
#28529 = CARTESIAN_POINT ( 'NONE',  ( 10.58508780786439374, 19.59913305159139441, 2.500000000000000000 ) ) ;
#28530 = CARTESIAN_POINT ( 'NONE',  ( 11.29080664838498649, 1.564594260697056104E-15, -2.500000000000000000 ) ) ;
#28531 = ORIENTED_EDGE ( 'NONE', *, *, #4346, .T. ) ;
#28532 = EDGE_LOOP ( 'NONE', ( #6168, #40176 ) ) ;
#28533 = CARTESIAN_POINT ( 'NONE',  ( 66.96854123855969476, 58.10689591609776983, 3.996990690923977407 ) ) ;
#28534 = CARTESIAN_POINT ( 'NONE',  ( -6.448748702180637338, -26.64985754041175525, 6.700000000000000178 ) ) ;
#28535 = CARTESIAN_POINT ( 'NONE',  ( 87.67494654488285732, -1.518266458920173312, 4.408571129606221994 ) ) ;
#28536 = B_SPLINE_CURVE_WITH_KNOTS ( 'NONE', 3,
 ( #37815, #27741, #31262, #34774, #12084, #18470, #9620, #21583, #31462, #31055, #27945, #24872, #37411, #15598, #28150, #3285, #40091, #33946, #5722, #36399, #27539, #24029 ),
 .UNSPECIFIED., .F., .F.,
 ( 4, 3, 3, 3, 3, 3, 3, 4 ),
 ( 4.982613841084487634E-18, 2.999644130997582546E-05, 6.002588995694560330E-05, 8.960886084587831848E-05, 0.0001190604700446494589, 0.0001489538463052702839, 0.0001796139255493956323, 0.0002076538946377561555 ),
 .UNSPECIFIED. ) ;
#28537 = EDGE_LOOP ( 'NONE', ( #9793, #33587, #42, #17751 ) ) ;
#28538 = CARTESIAN_POINT ( 'NONE',  ( 24.52463446364352251, 2.971563934966741094, 3.617821987212675783 ) ) ;
#28539 = SHAPE_REPRESENTATION_RELATIONSHIP ( 'NONE' , 'NONE' ,  #27999, #4380 ) ;
#28540 = EDGE_CURVE ( 'NONE', #15683, #25264, #7070, .T. ) ;
#28541 = CARTESIAN_POINT ( 'NONE',  ( -3.078675913592197944, -24.55319635012989110, 6.800000000000000711 ) ) ;
#28542 = CARTESIAN_POINT ( 'NONE',  ( 4.921324086407802056, -26.64985754041175525, 6.800000000000000711 ) ) ;
#28543 = VERTEX_POINT ( 'NONE', #3835 ) ;
#28544 = LINE ( 'NONE', #35152, #39953 ) ;
#28545 = CARTESIAN_POINT ( 'NONE',  ( -12.99139449055068241, -10.90558813203967148, 6.000000000000000000 ) ) ;
#28546 = ORIENTED_EDGE ( 'NONE', *, *, #25748, .F. ) ;
#28547 = EDGE_CURVE ( 'NONE', #33357, #23776, #16354, .T. ) ;
#28548 = ORIENTED_EDGE ( 'NONE', *, *, #17090, .T. ) ;
#28549 = CARTESIAN_POINT ( 'NONE',  ( 80.89520131247707013, 61.53942361443163378, -2.340042473998850348 ) ) ;
#28550 = CARTESIAN_POINT ( 'NONE',  ( -1.699110614488611226, -29.51162730196624651, 7.785315938117270740 ) ) ;
#28551 = CARTESIAN_POINT ( 'NONE',  ( 80.14986013843031287, 63.43437088187635453, 3.706996517075249020 ) ) ;
#28554 = EDGE_LOOP ( 'NONE', ( #21090, #203, #1752, #8299 ) ) ;
#28553 = ORIENTED_EDGE ( 'NONE', *, *, #33410, .F. ) ;
#28552 = CARTESIAN_POINT ( 'NONE',  ( -0.8150251588124118873, -27.28240185911760918, 6.865312560952603782 ) ) ;
#28555 = EDGE_CURVE ( 'NONE', #5955, #33555, #38695, .T. ) ;
#28556 = AXIS2_PLACEMENT_3D ( 'NONE', #25923, #14152, #7375 ) ;
#28557 = CIRCLE ( 'NONE', #325, 2.500000000000002220 ) ;
#28559 = ADVANCED_FACE ( 'NONE', ( #20649 ), #39178, .T. ) ;
#28558 = DIRECTION ( 'NONE',  ( -0.000000000000000000, -0.000000000000000000, 1.000000000000000000 ) ) ;
#28560 = CARTESIAN_POINT ( 'NONE',  ( 27.68079990455899875, -4.321696173663788443, 3.781977261579025917 ) ) ;
#28561 = CARTESIAN_POINT ( 'NONE',  ( 3.422192536544015340, -26.52273535105849689, 7.670465701733744091 ) ) ;
#28562 = CARTESIAN_POINT ( 'NONE',  ( -32.44874870218063734, -25.49307895267003587, 6.700000000000000178 ) ) ;
#28563 = CARTESIAN_POINT ( 'NONE',  ( 22.20314648110986866, 5.198427163008500607, -3.120655278281623257 ) ) ;
#28564 = ORIENTED_EDGE ( 'NONE', *, *, #21021, .T. ) ;
#28565 = FACE_OUTER_BOUND ( 'NONE', #28035, .T. ) ;
#28566 = ORIENTED_EDGE ( 'NONE', *, *, #23481, .F. ) ;
#28567 = AXIS2_PLACEMENT_3D ( 'NONE', #22107, #34684, #31169 ) ;
#28568 = CARTESIAN_POINT ( 'NONE',  ( -0.9891828103420344798, -31.64990550078098508, 6.865312560952604670 ) ) ;
#28569 = CARTESIAN_POINT ( 'NONE',  ( 1.700390093233090871, -29.56993018339339940, 7.750000000000000888 ) ) ;
#28570 = CARTESIAN_POINT ( 'NONE',  ( -80.20246960484742260, -5.670552041663467158, -3.761216877785253931 ) ) ;
#28571 = CARTESIAN_POINT ( 'NONE',  ( 11.65737507970504439, -32.06993018339339585, 6.800000000000000711 ) ) ;
#28572 = CARTESIAN_POINT ( 'NONE',  ( 2.406396206790859527, -33.27093018339341057, 6.954324564059724878 ) ) ;
#28573 = CARTESIAN_POINT ( 'NONE',  ( 78.91475304129781421, 66.06124928554449127, 1.777114115212670598 ) ) ;
#28574 = CARTESIAN_POINT ( 'NONE',  ( 86.71282820137585645, -0.9518751250403653108, -5.452277641718156431 ) ) ;
#28575 = DIRECTION ( 'NONE',  ( 1.000000000000000000, 0.000000000000000000, 0.000000000000000000 ) ) ;
#28576 = ORIENTED_EDGE ( 'NONE', *, *, #37534, .T. ) ;
#28577 = DIRECTION ( 'NONE',  ( 0.4690749385695657803, 0.8831583674551003460, 0.000000000000000000 ) ) ;
#28578 = CARTESIAN_POINT ( 'NONE',  ( 24.91801205947951559, 3.522942266573565018, -0.6749513148134329565 ) ) ;
#28579 = EDGE_LOOP ( 'NONE', ( #19335, #31105, #5521, #3881 ) ) ;
#28580 = CARTESIAN_POINT ( 'NONE',  ( 1.681622008834811721, -26.16998198393388009, 7.748216051605119503 ) ) ;
#28581 = CARTESIAN_POINT ( 'NONE',  ( -73.07498068578524908, 39.58105274722134226, 9.800414904976365804 ) ) ;
#28582 = LINE ( 'NONE', #16415, #5723 ) ;
#28583 = CARTESIAN_POINT ( 'NONE',  ( -1.748756095191392523, -28.97546355617463121, 7.635761828346576685 ) ) ;
#28584 = CARTESIAN_POINT ( 'NONE',  ( 33.68717198159223614, -3.103543658905335345, 5.464095933698846608 ) ) ;
#28585 = VECTOR ( 'NONE', #19616, 1000.000000000000000 ) ;
#28586 = VECTOR ( 'NONE', #784, 1000.000000000000000 ) ;
#28587 = CARTESIAN_POINT ( 'NONE',  ( 85.29288036551089647, 2.552713125850948117, 2.517437320556888736 ) ) ;
#28588 = VERTEX_POINT ( 'NONE', #11170 ) ;
#28590 = CARTESIAN_POINT ( 'NONE',  ( -62.14171895907916365, -49.48408358960642062, 4.951123000344127334 ) ) ;
#28589 = CARTESIAN_POINT ( 'NONE',  ( 79.82117971689783076, 65.09389273565577128, -3.300462285847908905 ) ) ;
#28591 = CARTESIAN_POINT ( 'NONE',  ( -70.53845072783826708, -45.66527594205425089, 9.992858605650345893 ) ) ;
#28592 = CARTESIAN_POINT ( 'NONE',  ( 21.67760900250310030, 6.625191744556888196, -3.088480972488703458 ) ) ;
#28593 = ORIENTED_EDGE ( 'NONE', *, *, #1781, .T. ) ;
#28594 = CARTESIAN_POINT ( 'NONE',  ( -1.633050216874273541, -28.90040684798571746, 7.782034975670478083 ) ) ;
#28595 = VECTOR ( 'NONE', #1173, 1000.000000000000000 ) ;
#28596 = VERTEX_POINT ( 'NONE', #29921 ) ;
#28597 = CARTESIAN_POINT ( 'NONE',  ( -77.44913293113614827, -6.200972306469667572, 7.584227517916080963 ) ) ;
#28598 = ORIENTED_EDGE ( 'NONE', *, *, #29977, .F. ) ;
#28599 = CARTESIAN_POINT ( 'NONE',  ( 78.77108537463556104, 65.94663689831973841, -1.925402693829578515 ) ) ;
#28600 = CARTESIAN_POINT ( 'NONE',  ( -70.92837670882074974, 0.2169278855384722815, 6.000000000000007994 ) ) ;
#28601 = B_SPLINE_CURVE_WITH_KNOTS ( 'NONE', 3,
 ( #7813, #7613, #32751, #39096, #20364, #20560, #11285, #14189, #16867, #32944 ),
 .UNSPECIFIED., .F., .F.,
 ( 4, 3, 3, 4 ),
 ( 0.0002170292169044780875, 0.0002420761345915950621, 0.0002723302478206961370, 0.0002816811360866806500 ),
 .UNSPECIFIED. ) ;
#28602 = CARTESIAN_POINT ( 'NONE',  ( 22.53775728690858315, 1.439289773552580254, 5.787755947322271055 ) ) ;
#28603 = EDGE_LOOP ( 'NONE', ( #9977, #12355, #11488, #1858 ) ) ;
#28604 = CARTESIAN_POINT ( 'NONE',  ( 78.93443484242880004, 66.17773471521378781, -1.251938014746446504 ) ) ;
#28605 = EDGE_CURVE ( 'NONE', #15988, #32186, #33231, .T. ) ;
#28607 = EDGE_CURVE ( 'NONE', #32868, #3311, #5017, .T. ) ;
#28606 = CARTESIAN_POINT ( 'NONE',  ( 4.745871275333505501, -31.29476187647891550, 7.730015791551949178 ) ) ;
#28609 = CARTESIAN_POINT ( 'NONE',  ( 85.70158270174225379, 2.093639263612781409, 3.671950081750952055 ) ) ;
#28608 = CARTESIAN_POINT ( 'NONE',  ( 4.591583649630617714, -31.35909501955320167, 6.864651958020304257 ) ) ;
#28610 = DIRECTION ( 'NONE',  ( 1.000000000000000000, -0.000000000000000000, 0.000000000000000000 ) ) ;
#28611 = B_SPLINE_CURVE_WITH_KNOTS ( 'NONE', 3,
 ( #34055, #5828, #12606, #18369, #40598, #24973, #21883, #34460, #73, #25172 ),
 .UNSPECIFIED., .F., .F.,
 ( 4, 3, 3, 4 ),
 ( 0.0002170292169044690887, 0.0002420761345915941947, 0.0002723302478206990102, 0.0002816811360866637907 ),
 .UNSPECIFIED. ) ;
#28612 = CARTESIAN_POINT ( 'NONE',  ( 0.5083189215983626719, -0.6000000000000004219, 3.960569937088427306 ) ) ;
#28613 = CARTESIAN_POINT ( 'NONE',  ( 71.78591447743995957, 60.68937113591298527, 3.856543183828340826 ) ) ;
#28614 = CARTESIAN_POINT ( 'NONE',  ( 22.01308812227411593, 4.306436655154639581, -3.976313850738264044 ) ) ;
#28615 = EDGE_LOOP ( 'NONE', ( #14561, #36442, #38667, #24276, #13341 ) ) ;
#28616 = VECTOR ( 'NONE', #26994, 1000.000000000000000 ) ;
#28617 = CARTESIAN_POINT ( 'NONE',  ( 21.85643539959778181, 10.07385928288181987, 4.538892979079195200 ) ) ;
#28618 = TOROIDAL_SURFACE ( 'NONE', #5565, 5.329987104167480894, 1.000000000000000000 ) ;
#28619 = CARTESIAN_POINT ( 'NONE',  ( 3.480609529026132520, -26.57320034156991184, 7.785096263473211486 ) ) ;
#28620 = ORIENTED_EDGE ( 'NONE', *, *, #10418, .T. ) ;
#28621 = LINE ( 'NONE', #37868, #31380 ) ;
#28622 = CARTESIAN_POINT ( 'NONE',  ( 81.13122672737068797, 64.30755116177446951, 3.292658836682930801 ) ) ;
#28623 = VECTOR ( 'NONE', #27456, 1000.000000000000000 ) ;
#28624 = B_SPLINE_CURVE_WITH_KNOTS ( 'NONE', 3,
 ( #28222, #12169, #40571, #25762 ),
 .UNSPECIFIED., .F., .F.,
 ( 4, 4 ),
 ( 0.000000000000000000, 0.0005391349717845224593 ),
 .UNSPECIFIED. ) ;
#28625 = CARTESIAN_POINT ( 'NONE',  ( 84.90669483503786807, 2.936226605105188625, 1.856525974524364297 ) ) ;
#28626 = VERTEX_POINT ( 'NONE', #17548 ) ;
#28627 = CIRCLE ( 'NONE', #1681, 3.499999999999999556 ) ;
#28628 = CARTESIAN_POINT ( 'NONE',  ( 0.5713750229309367823, -32.77700439067807281, 7.695279973900954751 ) ) ;
#28629 = CARTESIAN_POINT ( 'NONE',  ( 14.77909459087315724, -5.590190921940234148, 2.503920376596091124 ) ) ;
#28630 = CARTESIAN_POINT ( 'NONE',  ( 20.42596845097466129, 3.670375344256894934, -3.394364399325110693 ) ) ;
#28631 = DIRECTION ( 'NONE',  ( -0.000000000000000000, -0.000000000000000000, 1.000000000000000000 ) ) ;
#28632 = CARTESIAN_POINT ( 'NONE',  ( -72.84815947045271400, 2.214050502457695746, 10.96147798754371472 ) ) ;
#28633 = VERTEX_POINT ( 'NONE', #36511 ) ;
#28634 = CARTESIAN_POINT ( 'NONE',  ( -1.301082122417146048, -31.16716842155108580, 7.759451378593094972 ) ) ;
#28635 = CARTESIAN_POINT ( 'NONE',  ( 32.01160973108229513, -3.695318852608926008, 4.882771644002913192 ) ) ;
#28636 = VERTEX_POINT ( 'NONE', #23347 ) ;
#28637 = ORIENTED_EDGE ( 'NONE', *, *, #33451, .F. ) ;
#28638 = CARTESIAN_POINT ( 'NONE',  ( 21.73770031614145992, 4.234352576155473002, 2.806692369165114442 ) ) ;
#28639 = DIRECTION ( 'NONE',  ( 0.000000000000000000, 0.000000000000000000, 1.000000000000000000 ) ) ;
#28640 = CARTESIAN_POINT ( 'NONE',  ( 66.27376694609004915, 57.73522568913436004, -4.000000000000000000 ) ) ;
#28641 = VERTEX_POINT ( 'NONE', #14668 ) ;
#28642 = VECTOR ( 'NONE', #36277, 1000.000000000000000 ) ;
#28643 = CARTESIAN_POINT ( 'NONE',  ( 87.73404314631468992, -0.1893167741230248335, -3.839138754766225237 ) ) ;
#28644 = CARTESIAN_POINT ( 'NONE',  ( -71.72837670882105954, -34.30579396504363388, -1.385640646055078307 ) ) ;
#28645 = CARTESIAN_POINT ( 'NONE',  ( 4.942166287043163742, -28.54480233319798543, 6.868387053540520704 ) ) ;
#28646 =( NAMED_UNIT ( * ) SI_UNIT ( $, .STERADIAN. ) SOLID_ANGLE_UNIT ( ) );
#28647 = EDGE_LOOP ( 'NONE', ( #34791, #4900, #24805, #31293 ) ) ;
#28648 = FACE_BOUND ( 'NONE', #23225, .T. ) ;
#28649 =( NAMED_UNIT ( * ) SI_UNIT ( $, .STERADIAN. ) SOLID_ANGLE_UNIT ( ) );
#28650 = ORIENTED_EDGE ( 'NONE', *, *, #2019, .F. ) ;
#28651 = AXIS2_PLACEMENT_3D ( 'NONE', #11568, #1945, #39798 ) ;
#28652 = CARTESIAN_POINT ( 'NONE',  ( 82.52706534919252590, 63.19378067493415330, -1.386429027374526557 ) ) ;
#28653 = CARTESIAN_POINT ( 'NONE',  ( 81.04993867939978713, 61.73413400689827313, 2.516896548562573610 ) ) ;
#28655 = EDGE_CURVE ( 'NONE', #19268, #25058, #9236, .T. ) ;
#28654 = CARTESIAN_POINT ( 'NONE',  ( 2.955826417700654130, -26.41018881579227795, 7.774064877406525298 ) ) ;
#28656 = ORIENTED_EDGE ( 'NONE', *, *, #1562, .F. ) ;
#28657 = ORIENTED_EDGE ( 'NONE', *, *, #19980, .T. ) ;
#28658 = CARTESIAN_POINT ( 'NONE',  ( 75.66308047697206973, 62.61957414976298963, -3.723120700747940770 ) ) ;
#28660 = DIRECTION ( 'NONE',  ( 0.000000000000000000, 0.000000000000000000, 1.000000000000000000 ) ) ;
#28659 = CARTESIAN_POINT ( 'NONE',  ( 2.482793419929769207, -26.15850159197103508, 7.002103980607166989 ) ) ;
#28661 = CARTESIAN_POINT ( 'NONE',  ( 15.23622953457498497, 11.45049469319151214, -2.584380127111126413 ) ) ;
#28662 = CARTESIAN_POINT ( 'NONE',  ( 80.95544561733511557, 63.83034742112755566, -3.486376426170565868 ) ) ;
#28663 = CARTESIAN_POINT ( 'NONE',  ( -14.34874870218063769, -26.64985754041175525, 6.700000000000000178 ) ) ;
#28664 = CARTESIAN_POINT ( 'NONE',  ( 77.48272095992959407, 61.71466691532017990, 3.776276000690670376 ) ) ;
#28665 = EDGE_CURVE ( 'NONE', #23338, #39035, #15620, .T. ) ;
#28666 = VERTEX_POINT ( 'NONE', #17150 ) ;
#28667 = CARTESIAN_POINT ( 'NONE',  ( 16.11725891508299924, 15.27317977276803873, 2.500000000000000000 ) ) ;
#28668 = CARTESIAN_POINT ( 'NONE',  ( -58.83394063668751528, 29.29677716115665831, 5.900615745428536840 ) ) ;
#28669 = CARTESIAN_POINT ( 'NONE',  ( 82.04814969336737818, 64.78574761690819628, 2.164558651853291771 ) ) ;
#28671 = CARTESIAN_POINT ( 'NONE',  ( 16.54830199238246990, 9.917958269357011858, 2.500000000000051514 ) ) ;
#28670 = DIRECTION ( 'NONE',  ( 0.000000000000000000, 0.000000000000000000, 1.000000000000000000 ) ) ;
#28672 = CARTESIAN_POINT ( 'NONE',  ( 30.28570682881508702, -1.586248365680131167, -6.023113166707004140 ) ) ;
#28673 = CARTESIAN_POINT ( 'NONE',  ( -34.97867591359219830, -26.64985754041175525, 6.700000000000000178 ) ) ;
#28674 = CARTESIAN_POINT ( 'NONE',  ( 3.875507134935765041, -26.95672030760948346, 7.635761828346577573 ) ) ;
#28675 = CARTESIAN_POINT ( 'NONE',  ( 4.737606180627847330, -31.30928207488832626, 7.756742906098588186 ) ) ;
#28676 = CARTESIAN_POINT ( 'NONE',  ( 1.668552422811426572, -26.07007435252865690, 7.724038915126860694 ) ) ;
#28677 = AXIS2_PLACEMENT_3D ( 'NONE', #3414, #32003, #9754 ) ;
#28678 = CARTESIAN_POINT ( 'NONE',  ( 72.82963479777622240, 58.84354944748790217, 3.620166419653539691 ) ) ;
#28679 = LINE ( 'NONE', #3787, #8443 ) ;
#28680 = CARTESIAN_POINT ( 'NONE',  ( 23.23260763512989158, 3.379986173245406178, -3.619755483646863503 ) ) ;
#28681 = CARTESIAN_POINT ( 'NONE',  ( 3.254454494278365306, -26.53796732577102802, 7.139196562012272373 ) ) ;
#28682 = DIRECTION ( 'NONE',  ( 1.000000000000000000, 0.000000000000000000, 0.000000000000000000 ) ) ;
#28683 = CARTESIAN_POINT ( 'NONE',  ( 1.726000212023766522, -32.96983583034973719, 7.652160403243383868 ) ) ;
#28684 = CARTESIAN_POINT ( 'NONE',  ( 0.6959572223689035608, -26.21002107485291077, 7.387053503561886281 ) ) ;
#28685 = EDGE_CURVE ( 'NONE', #38999, #16562, #18226, .T. ) ;
#28686 = CARTESIAN_POINT ( 'NONE',  ( 28.66920249112477848, -4.024975064351027143, -4.110187144531254333 ) ) ;
#28687 = CARTESIAN_POINT ( 'NONE',  ( -1.502930774124977997, -28.43029404775827373, 7.740055089680399902 ) ) ;
#28688 = DIRECTION ( 'NONE',  ( -1.000000000000000000, 0.000000000000000000, 0.000000000000000000 ) ) ;
#28689 = ORIENTED_EDGE ( 'NONE', *, *, #14723, .F. ) ;
#28690 = DIRECTION ( 'NONE',  ( 0.000000000000000000, -0.000000000000000000, -1.000000000000000000 ) ) ;
#28691 = CARTESIAN_POINT ( 'NONE',  ( 68.53436546801150087, 58.80600050245282517, -3.985059344218151445 ) ) ;
#28692 = ADVANCED_FACE ( 'NONE', ( #33452 ), #17754, .T. ) ;
#28693 = ORIENTED_EDGE ( 'NONE', *, *, #10067, .T. ) ;
#28694 = DIRECTION ( 'NONE',  ( 1.000000000000000000, -0.000000000000000000, -0.000000000000000000 ) ) ;
#28695 = CARTESIAN_POINT ( 'NONE',  ( 30.81211655921321935, -3.351903339995823128, 4.959630491910277605 ) ) ;
#28696 = CARTESIAN_POINT ( 'NONE',  ( 22.03914767488266691, 3.561355022793854630, 4.473374508569111896 ) ) ;
#28697 = CARTESIAN_POINT ( 'NONE',  ( 5.004837170140412184, -28.41636597135046216, 6.880608371227948439 ) ) ;
#28698 = DIRECTION ( 'NONE',  ( -0.000000000000000000, -0.000000000000000000, -1.000000000000000000 ) ) ;
#28699 = CARTESIAN_POINT ( 'NONE',  ( 1.138162326717552908, -26.11537075939349606, 6.880608371227948439 ) ) ;
#28700 = ORIENTED_EDGE ( 'NONE', *, *, #22004, .F. ) ;
#28701 = DIRECTION ( 'NONE',  ( 0.000000000000000000, 0.000000000000000000, -1.000000000000000000 ) ) ;
#28702 = CARTESIAN_POINT ( 'NONE',  ( 78.97731087898851854, 65.91669204587326192, 2.137206601789621185 ) ) ;
#28704 = EDGE_CURVE ( 'NONE', #31282, #29781, #29531, .T. ) ;
#28703 = CARTESIAN_POINT ( 'NONE',  ( -1.411741797515851271, -31.17137799540083876, 7.013842709614101167 ) ) ;
#28705 = ORIENTED_EDGE ( 'NONE', *, *, #14972, .F. ) ;
#28706 = CARTESIAN_POINT ( 'NONE',  ( 80.29582733418162377, 61.38465067277564202, -2.608847861177660654 ) ) ;
#28708 = CARTESIAN_POINT ( 'NONE',  ( 4.224974933773748553, -31.84731275619759927, 7.754798119455333705 ) ) ;
#28707 = CARTESIAN_POINT ( 'NONE',  ( 24.71218170711417272, 0.6478519780817281193, 4.786773077597882953 ) ) ;
#28709 = VECTOR ( 'NONE', #30159, 1000.000000000000114 ) ;
#28710 = CARTESIAN_POINT ( 'NONE',  ( 80.26729624682485564, 65.68772892857229806, -2.758880570191356796 ) ) ;
#28711 = CARTESIAN_POINT ( 'NONE',  ( 78.31969284963511768, 65.55289002357415029, 2.305838555344982499 ) ) ;
#28712 = VECTOR ( 'NONE', #35464, 1000.000000000000000 ) ;
#28713 = DIRECTION ( 'NONE',  ( -0.000000000000000000, -1.000000000000000000, -0.000000000000000000 ) ) ;
#28714 = CARTESIAN_POINT ( 'NONE',  ( -64.08758708074093136, 43.50655619156747633, 1.588711929257163868 ) ) ;
#28715 = B_SPLINE_CURVE_WITH_KNOTS ( 'NONE', 3,
 ( #19263, #13080, #25642, #38793, #26851, #39391, #4827, #20457, #1750, #33035, #17162, #33244, #1356, #8095, #32841, #39189, #11182, #26260, #29540, #5029, #26655, #36324, #35728, #27055, #7908, #36127, #29338, #32643, #17354, #38984, #4439 ),
 .UNSPECIFIED., .F., .F.,
 ( 4, 3, 3, 3, 3, 3, 3, 3, 3, 3, 4 ),
 ( 4.336808689942017736E-19, 3.077658087705600095E-05, 6.152638666998949115E-05, 9.267501192706537668E-05, 0.0001241882240135188460, 0.0001556618703051674505, 0.0001866161554452211923, 0.0002167966385860986621, 0.0002463805737537775979, 0.0002758761370306543332, 0.0002847094172290070006 ),
 .UNSPECIFIED. ) ;
#28716 = CARTESIAN_POINT ( 'NONE',  ( 22.31703049540045924, 6.264542857755036387, 0.009563241200241559548 ) ) ;
#28717 = DIRECTION ( 'NONE',  ( 1.000000000000000000, 0.000000000000000000, 0.000000000000000000 ) ) ;
#28718 = ORIENTED_EDGE ( 'NONE', *, *, #7495, .T. ) ;
#28719 = CARTESIAN_POINT ( 'NONE',  ( -74.87858385344040357, 7.803706760580113588, 9.233433073997890261 ) ) ;
#28720 = CARTESIAN_POINT ( 'NONE',  ( 22.60587387393427150, 0.2865033312617634720, -6.509150990572208251 ) ) ;
#28721 = EDGE_CURVE ( 'NONE', #32112, #34664, #38972, .T. ) ;
#28722 = CARTESIAN_POINT ( 'NONE',  ( -0.08658257670950372797, -32.56233827099918443, 7.785344483711591934 ) ) ;
#28723 = EDGE_LOOP ( 'NONE', ( #18681, #15514, #38074, #11374 ) ) ;
#28724 = CARTESIAN_POINT ( 'NONE',  ( -1.042158050042817585, -31.73691429932165420, 7.771081512783705847 ) ) ;
#28725 = CARTESIAN_POINT ( 'NONE',  ( 28.74843373310636707, -3.747644898664072688, -4.540536534472360941 ) ) ;
#28726 = CARTESIAN_POINT ( 'NONE',  ( 37.10943087117655637, -2.404357389779887555, -5.951804628107819184 ) ) ;
#28727 = DIRECTION ( 'NONE',  ( 1.000000000000000000, 1.682730792515357087E-16, -0.000000000000000000 ) ) ;
#28728 = CARTESIAN_POINT ( 'NONE',  ( 16.37363295469527102, 9.900998059239732640, 2.761899439026373582 ) ) ;
#28729 = DIRECTION ( 'NONE',  ( 1.000000000000000000, 0.000000000000000000, 0.000000000000000000 ) ) ;
#28730 = CARTESIAN_POINT ( 'NONE',  ( 30.59788246744356854, -3.614912645528273849, 4.745426083186703003 ) ) ;
#28731 = CARTESIAN_POINT ( 'NONE',  ( -60.05933043039490826, 24.84364830758654108, -9.240995299818665742 ) ) ;
#28732 = CARTESIAN_POINT ( 'NONE',  ( -21.07867591359219617, -26.64985754041175525, 6.700000000000000178 ) ) ;
#28733 = CARTESIAN_POINT ( 'NONE',  ( 22.77327910074270889, 0.4820626211097077118, -6.224882446762404875 ) ) ;
#28734 = CARTESIAN_POINT ( 'NONE',  ( 36.20303916938638622, -1.578649729842889649, -5.665109327158619479 ) ) ;
#28735 = CARTESIAN_POINT ( 'NONE',  ( -24.87867591359218977, -26.64985754041175525, 6.700000000000000178 ) ) ;
#28736 = ORIENTED_EDGE ( 'NONE', *, *, #16907, .F. ) ;
#28737 =( BOUNDED_CURVE ( )  B_SPLINE_CURVE ( 3, ( #5838, #24356, #30344, #2150 ),
 .UNSPECIFIED., .F., .T. ) 
 B_SPLINE_CURVE_WITH_KNOTS ( ( 4, 4 ),
 ( 1.347909859412855127, 1.534781240595300744 ),
 .UNSPECIFIED. ) 
 CURVE ( )  GEOMETRIC_REPRESENTATION_ITEM ( )  RATIONAL_B_SPLINE_CURVE ( ( 1.000000000000000000, 0.9970920404276225613, 0.9970920404276225613, 1.000000000000000000 ) ) 
 REPRESENTATION_ITEM ( '' )  );
#28738 = EDGE_CURVE ( 'NONE', #28626, #36858, #4621, .T. ) ;
#28739 = AXIS2_PLACEMENT_3D ( 'NONE', #34590, #25703, #27967 ) ;
#28741 = EDGE_CURVE ( 'NONE', #31670, #24744, #18787, .T. ) ;
#28740 = CARTESIAN_POINT ( 'NONE',  ( 66.74698822326750758, 57.80221319398844315, 3.998057522770657624 ) ) ;
#28742 = EDGE_CURVE ( 'NONE', #39711, #11084, #24353, .T. ) ;
#28743 = CARTESIAN_POINT ( 'NONE',  ( 2.285759857818613572, -26.11922848102776484, 7.742274884880762542 ) ) ;
#28744 = CARTESIAN_POINT ( 'NONE',  ( 84.45327006356104960, 2.923007647743876447, -2.091752339247905823 ) ) ;
#28745 = DIRECTION ( 'NONE',  ( 1.047444401652940007E-14, -1.000000000000000000, -0.000000000000000000 ) ) ;
#28746 = ORIENTED_EDGE ( 'NONE', *, *, #9799, .T. ) ;
#28747 = CARTESIAN_POINT ( 'NONE',  ( 24.59812680050050915, 2.980866690065322011, 3.560245512678282598 ) ) ;
#28748 = DIRECTION ( 'NONE',  ( 1.000000000000000000, 0.000000000000000000, 0.000000000000000000 ) ) ;
#28749 = CARTESIAN_POINT ( 'NONE',  ( 5.121324086407808451, -24.55319635012989110, 6.800000000000000711 ) ) ;
#28750 = CARTESIAN_POINT ( 'NONE',  ( 1.178420402900119512, -26.11942198568385010, 7.780491323090171996 ) ) ;
#28751 = ORIENTED_EDGE ( 'NONE', *, *, #5617, .F. ) ;
#28752 = DIRECTION ( 'NONE',  ( -0.000000000000000000, -0.000000000000000000, 1.000000000000000000 ) ) ;
#28753 = ORIENTED_EDGE ( 'NONE', *, *, #12314, .T. ) ;
#28754 = ORIENTED_EDGE ( 'NONE', *, *, #7287, .T. ) ;
#28755 = CARTESIAN_POINT ( 'NONE',  ( 80.91969899470512928, 61.54505855127015934, -2.326060681237731576 ) ) ;
#28756 = CARTESIAN_POINT ( 'NONE',  ( 4.355058743506291741, -27.27855411587562884, 7.255881584735162093 ) ) ;
#28757 = CARTESIAN_POINT ( 'NONE',  ( 80.69037048981478222, 62.35571368504050582, 3.252077313700840300 ) ) ;
#28760 = ORIENTED_EDGE ( 'NONE', *, *, #4934, .T. ) ;
#28759 = VERTEX_POINT ( 'NONE', #28257 ) ;
#28758 = CARTESIAN_POINT ( 'NONE',  ( -1.309506077955794323, -31.15126656862256027, 6.865312560952602006 ) ) ;
#28761 = CARTESIAN_POINT ( 'NONE',  ( -58.17279802585986204, 29.79606812221977563, 4.661957855074470025 ) ) ;
#28762 = CARTESIAN_POINT ( 'NONE',  ( -0.5217032702065450556, -32.27405686018898479, 7.697032948437508182 ) ) ;
#28763 = CARTESIAN_POINT ( 'NONE',  ( -1.788336217227144198, -29.48479552071361809, 7.780491323090173772 ) ) ;
#28764 = CIRCLE ( 'NONE', #24800, 0.1000000000000028644 ) ;
#28765 = CARTESIAN_POINT ( 'NONE',  ( 21.85643539959772497, -14.97654459006671068, 3.851724272136834326 ) ) ;
#28766 = AXIS2_PLACEMENT_3D ( 'NONE', #24772, #27447, #2767 ) ;
#28767 = CARTESIAN_POINT ( 'NONE',  ( 22.39454719451790510, 4.886617018807966950, -3.092752845356960822 ) ) ;
#28768 = ORIENTED_EDGE ( 'NONE', *, *, #32739, .T. ) ;
#28769 = LINE ( 'NONE', #13117, #7097 ) ;
#28770 = VECTOR ( 'NONE', #8103, 1000.000000000000000 ) ;
#28771 = ORIENTED_EDGE ( 'NONE', *, *, #40102, .F. ) ;
#28772 = EDGE_CURVE ( 'NONE', #38473, #7785, #27846, .T. ) ;
#28773 = CARTESIAN_POINT ( 'NONE',  ( -0.9826570473272854267, -31.65831881584441021, 6.863904403958576594 ) ) ;
#28774 = CARTESIAN_POINT ( 'NONE',  ( -0.5731604851916571874, -32.21200110443151488, 7.785096263473213263 ) ) ;
#28775 = CARTESIAN_POINT ( 'NONE',  ( -77.24581433579317036, -6.124437853233426488, -7.754200975113157313 ) ) ;
#28776 = CARTESIAN_POINT ( 'NONE',  ( 1.700390093233090871, -29.56993018339339940, 7.800000000000000711 ) ) ;
#28777 = DIRECTION ( 'NONE',  ( 0.000000000000000000, 0.000000000000000000, 1.000000000000000000 ) ) ;
#28778 = CARTESIAN_POINT ( 'NONE',  ( 79.95152939680102122, 65.17166210280107919, 3.248659383495577480 ) ) ;
#28779 = CARTESIAN_POINT ( 'NONE',  ( 87.05329302184628659, -1.423768201249274945, 4.835531253876708568 ) ) ;
#28780 = DIRECTION ( 'NONE',  ( 1.000000000000000000, 0.000000000000000000, 0.000000000000000000 ) ) ;
#28781 = CARTESIAN_POINT ( 'NONE',  ( -0.8809027425463861194, -31.78283038357269419, 7.693875151218755093 ) ) ;
#28782 = CARTESIAN_POINT ( 'NONE',  ( 4.589539118170550935, -31.36237908435458976, 7.768425012602596880 ) ) ;
#28783 = EDGE_CURVE ( 'NONE', #25658, #2020, #21074, .T. ) ;
#28784 = DIRECTION ( 'NONE',  ( 0.000000000000000000, -1.000000000000000000, -0.000000000000000000 ) ) ;
#28785 = EDGE_CURVE ( 'NONE', #13485, #40691, #25473, .T. ) ;
#28786 = CARTESIAN_POINT ( 'NONE',  ( -70.92837670882107659, -60.53509472482660669, 0.000000000000000000 ) ) ;
#28787 = CARTESIAN_POINT ( 'NONE',  ( -12.99139449055068241, -10.90558813203967148, 6.000000000000000000 ) ) ;
#28788 = CARTESIAN_POINT ( 'NONE',  ( 69.07430361466936120, 59.13263628650475567, 3.969490915146614007 ) ) ;
#28789 = CARTESIAN_POINT ( 'NONE',  ( 36.99314941111227739, -2.718566000083574519, 5.980073666940257660 ) ) ;
#28790 = EDGE_CURVE ( 'NONE', #4723, #31392, #6374, .T. ) ;
#28792 = CIRCLE ( 'NONE', #24851, 0.1000000000000028644 ) ;
#28791 = CARTESIAN_POINT ( 'NONE',  ( 73.38675137958711048, 60.10977650211887635, -3.914122288815134798 ) ) ;
#28793 = CARTESIAN_POINT ( 'NONE',  ( 4.291692624794518629, -31.77112207655784815, 7.779495906702011965 ) ) ;
#28794 = B_SPLINE_CURVE_WITH_KNOTS ( 'NONE', 3,
 ( #20635, #30330, #14865, #14261, #17141, #36500, #1523, #39576, #11560, #27436, #24344, #10964, #2137, #39371, #11162, #29713, #26633, #20846, #23545, #17950, #39992, #33439, #11763, #17537, #24137 ),
 .UNSPECIFIED., .F., .F.,
 ( 4, 3, 3, 3, 3, 3, 3, 3, 4 ),
 ( 6.468151674594376400E-05, 9.076621574722102369E-05, 0.0001210204262067959878, 0.0001512763324577431315, 0.0001815301820994218911, 0.0002117781465860683475, 0.0002420274594459756413, 0.0002722905548971167101, 0.0002816827545175690879 ),
 .UNSPECIFIED. ) ;
#28795 = CARTESIAN_POINT ( 'NONE',  ( 87.05115134601746263, 0.5777397079708905814, 5.111878656935144427 ) ) ;
#28796 = ORIENTED_EDGE ( 'NONE', *, *, #31764, .F. ) ;
#28798 = CARTESIAN_POINT ( 'NONE',  ( 14.71586241334793677, -5.063781084897545526, 2.500000000000000444 ) ) ;
#28797 = CARTESIAN_POINT ( 'NONE',  ( 81.28814307398172900, 61.80674180605062418, -2.393593008231202024 ) ) ;
#28799 = LINE ( 'NONE', #2888, #3108 ) ;
#28800 = VECTOR ( 'NONE', #22438, 1000.000000000000000 ) ;
#28801 = CARTESIAN_POINT ( 'NONE',  ( 14.77291369204805882, 13.25874409045904301, -2.500174547565549243 ) ) ;
#28802 = ORIENTED_EDGE ( 'NONE', *, *, #25489, .T. ) ;
#28803 = CARTESIAN_POINT ( 'NONE',  ( -1.640792392766696750, -28.94017299183985514, 7.784838882742138644 ) ) ;
#28804 = ORIENTED_EDGE ( 'NONE', *, *, #9729, .F. ) ;
#28805 = CARTESIAN_POINT ( 'NONE',  ( -71.75719754330091860, 2.253829733506131472, 9.965625675682359130 ) ) ;
#28806 = ORIENTED_EDGE ( 'NONE', *, *, #1016, .T. ) ;
#28807 = CARTESIAN_POINT ( 'NONE',  ( 79.92294945466714751, 64.42298636752006757, -3.607546830629785539 ) ) ;
#28808 = CARTESIAN_POINT ( 'NONE',  ( 5.153168895494497193, -30.14292259869292678, 7.707984471951054850 ) ) ;
#28809 = CARTESIAN_POINT ( 'NONE',  ( 24.50968518362478576, 2.239917399590349856, 4.180759367608843924 ) ) ;
#28811 = ORIENTED_EDGE ( 'NONE', *, *, #18929, .T. ) ;
#28810 = ORIENTED_EDGE ( 'NONE', *, *, #1697, .T. ) ;
#28812 = CARTESIAN_POINT ( 'NONE',  ( 11.65737507970504616, -30.94667987854474234, 6.800000000000000711 ) ) ;
#28813 = CIRCLE ( 'NONE', #35387, 3.000000000000002665 ) ;
#28815 = FACE_OUTER_BOUND ( 'NONE', #17739, .T. ) ;
#28814 = CARTESIAN_POINT ( 'NONE',  ( 4.538070851940716466, -31.44278039407777214, 6.988553391373220514 ) ) ;
#28816 = CARTESIAN_POINT ( 'NONE',  ( -7.078675913592194391, -26.64985754041175525, 6.700000000000000178 ) ) ;
#28817 = CARTESIAN_POINT ( 'NONE',  ( -64.08758708074093136, 43.50509228929546879, -1.592748447102107390 ) ) ;
#28818 = CARTESIAN_POINT ( 'NONE',  ( 72.29787722903529357, 59.46803282872462404, 3.909340765805334961 ) ) ;
#28819 = CARTESIAN_POINT ( 'NONE',  ( 22.78500653003857934, 3.697042830259541724, -3.776378161709064152 ) ) ;
#28820 = ORIENTED_EDGE ( 'NONE', *, *, #23889, .F. ) ;
#28821 = ORIENTED_EDGE ( 'NONE', *, *, #38805, .T. ) ;
#28822 = CIRCLE ( 'NONE', #11029, 0.9999999999999998890 ) ;
#28823 = CARTESIAN_POINT ( 'NONE',  ( 21.85643539959773207, -8.152057848754798997, -9.377623736650162911 ) ) ;
#28824 = CARTESIAN_POINT ( 'NONE',  ( 21.87751110072621685, 4.134169920257987130, -2.121951800785348841 ) ) ;
#28825 = DIRECTION ( 'NONE',  ( 1.000000000000000000, 0.000000000000000000, 0.000000000000000000 ) ) ;
#28826 = CARTESIAN_POINT ( 'NONE',  ( 81.36150051721972432, 64.03901721960635030, 3.243459512806143419 ) ) ;
#28827 = CARTESIAN_POINT ( 'NONE',  ( 88.47081344899795852, -1.206222823704210301, -3.524641158899461058 ) ) ;
#28828 = ORIENTED_EDGE ( 'NONE', *, *, #22395, .T. ) ;
#28829 = CARTESIAN_POINT ( 'NONE',  ( 14.77315594796436926, 13.19392823276591464, 2.499999999999996891 ) ) ;
#28830 = VECTOR ( 'NONE', #1152, 1000.000000000000000 ) ;
#28831 = CARTESIAN_POINT ( 'NONE',  ( 28.89967557733805137, -2.887797800998441744, 4.716891333775404149 ) ) ;
#28832 = CARTESIAN_POINT ( 'NONE',  ( 29.11494709149169324, -3.933151727299639244, 4.208129513927731935 ) ) ;
#28833 = CARTESIAN_POINT ( 'NONE',  ( 29.10199195035972153, 0.3604134132878261121, -4.748467696825394491 ) ) ;
#28834 = CARTESIAN_POINT ( 'NONE',  ( 0.5687451785976556096, -32.77607959874935517, 7.670860738520328681 ) ) ;
#28835 = DIRECTION ( 'NONE',  ( 0.000000000000000000, 0.000000000000000000, 1.000000000000000000 ) ) ;
#28836 = CARTESIAN_POINT ( 'NONE',  ( -63.99293516169446150, 35.89893413629672381, -7.506047544094577084 ) ) ;
#28837 = ADVANCED_FACE ( 'NONE', ( #36710 ), #24981, .F. ) ;
#28838 = ADVANCED_FACE ( 'NONE', ( #21277, #12200 ), #28056, .F. ) ;
#28839 = PLANE ( 'NONE',  #23067 ) ;
#28840 = ADVANCED_FACE ( 'NONE', ( #40604 ), #34467, .F. ) ;
#28841 = CARTESIAN_POINT ( 'NONE',  ( 31.99136750572645482, -3.506164123272953681, 5.093361180844341085 ) ) ;
#28842 = EDGE_LOOP ( 'NONE', ( #34032, #18975, #39506, #22651 ) ) ;
#28843 = ORIENTED_EDGE ( 'NONE', *, *, #29933, .T. ) ;
#28844 = CARTESIAN_POINT ( 'NONE',  ( 33.68505034223440475, -3.839218838710527049, 5.138863580400442110 ) ) ;
#28845 = VECTOR ( 'NONE', #35913, 1000.000000000000000 ) ;
#28846 = CARTESIAN_POINT ( 'NONE',  ( 1.649030408997186781, -33.05491794072131739, 7.785344483711591934 ) ) ;
#28847 = CARTESIAN_POINT ( 'NONE',  ( 66.57374945270225908, 57.82325632336715415, -3.999874661881728688 ) ) ;
#28848 = CARTESIAN_POINT ( 'NONE',  ( -0.4524766833400662436, -26.81037104761097112, 7.751599049952197618 ) ) ;
#28849 = ORIENTED_EDGE ( 'NONE', *, *, #22441, .F. ) ;
#28850 = LINE ( 'NONE', #38100, #1792 ) ;
#28851 = ORIENTED_EDGE ( 'NONE', *, *, #27568, .T. ) ;
#28852 = CARTESIAN_POINT ( 'NONE',  ( -62.92837670882106238, 0.7293679304675904085, 6.000000000000000000 ) ) ;
#28853 = PRESENTATION_STYLE_ASSIGNMENT (( #31741 ) ) ;
#28854 = VERTEX_POINT ( 'NONE', #15702 ) ;
#28855 = CARTESIAN_POINT ( 'NONE',  ( 82.56043351944043707, 63.54438683934779419, -1.421283058691077850 ) ) ;
#28856 = CIRCLE ( 'NONE', #13745, 0.1000000000000028644 ) ;
#28857 = CARTESIAN_POINT ( 'NONE',  ( -1.751191296394976060, -28.98974609548212555, 7.733670252284493785 ) ) ;
#28858 = EDGE_LOOP ( 'NONE', ( #10074, #6568, #33566, #35536 ) ) ;
#28859 = EDGE_LOOP ( 'NONE', ( #829, #3939, #35218, #17248, #19169 ) ) ;
#28860 = CARTESIAN_POINT ( 'NONE',  ( 75.21236926079949114, 60.63031288236823002, -3.833662259905124436 ) ) ;
#28862 = CARTESIAN_POINT ( 'NONE',  ( 1.300000000000000044, 0.5999999999999995337, -4.030609108440248889 ) ) ;
#28861 = CARTESIAN_POINT ( 'NONE',  ( -42.24874870218063450, -25.49307895267003587, 6.700000000000000178 ) ) ;
#28863 = CARTESIAN_POINT ( 'NONE',  ( 16.14962678690648090, 10.32852357150096090, -2.711842976054151144 ) ) ;
#28864 = CARTESIAN_POINT ( 'NONE',  ( 75.90485726080819973, 62.11260916716570080, 3.867068906737703760 ) ) ;
#28865 = ORIENTED_EDGE ( 'NONE', *, *, #30751, .F. ) ;
#28866 = DIRECTION ( 'NONE',  ( 0.000000000000000000, 1.000000000000000000, 0.000000000000000000 ) ) ;
#28867 = CYLINDRICAL_SURFACE ( 'NONE', #21485, 24.28220113893567600 ) ;
#28868 = CARTESIAN_POINT ( 'NONE',  ( 22.63302891745040668, 3.893813116402496277, -3.738829563077739504 ) ) ;
#28869 = CARTESIAN_POINT ( 'NONE',  ( 81.60411730068159386, 64.94496191031764454, 2.665107514500538066 ) ) ;
#28871 = CARTESIAN_POINT ( 'NONE',  ( 12.97258478262502202, 9.268119072443660400, 3.480631332370867970 ) ) ;
#28870 = CARTESIAN_POINT ( 'NONE',  ( -0.2075784994539575656, -32.50415316031815394, 6.989977667959447416 ) ) ;
#28872 = B_SPLINE_CURVE_WITH_KNOTS ( 'NONE', 3,
 ( #14042, #39152, #1121, #4991, #16716, #36095, #29306, #14443, #27014, #23127, #4787, #1921, #4404, #8257, #7873, #13652, #17124, #26817, #39560, #11343, #26223, #4198, #20420, #35894, #23909, #38757, #39355, #1713, #14243, #20026, #11147 ),
 .UNSPECIFIED., .F., .F.,
 ( 4, 3, 3, 3, 3, 3, 3, 3, 3, 3, 4 ),
 ( 6.484403375995018940E-05, 8.983333709522135736E-05, 0.0001203539973219361814, 0.0001514144607149705657, 0.0001828916862241641026, 0.0002144221682127259491, 0.0002455195857862198022, 0.0002758614570916272644, 0.0003055381793602568452, 0.0003350143730643693964, 0.0003497271997307906436 ),
 .UNSPECIFIED. ) ;
#28873 = CARTESIAN_POINT ( 'NONE',  ( 28.93850508814251299, -1.888738275646064668, -5.863986819262115624 ) ) ;
#28874 = CARTESIAN_POINT ( 'NONE',  ( 2.255350295996689347, -26.21552723005750352, 7.695279973900954751 ) ) ;
#28875 = CARTESIAN_POINT ( 'NONE',  ( -12.99139449055068241, -10.90558813203967148, 6.000000000000000000 ) ) ;
#28876 = DIRECTION ( 'NONE',  ( 1.000000000000000000, 0.000000000000000000, 0.000000000000000000 ) ) ;
#28877 = VERTEX_POINT ( 'NONE', #11573 ) ;
#28878 = DIRECTION ( 'NONE',  ( -0.000000000000000000, -0.000000000000000000, -1.000000000000000000 ) ) ;
#28879 = DIRECTION ( 'NONE',  ( 0.9267318687906771491, -0.3757233601570964532, 0.000000000000000000 ) ) ;
#28880 = CARTESIAN_POINT ( 'NONE',  ( 33.66554628656592030, -3.445943206981954443, -5.444051220130533331 ) ) ;
#28881 = CARTESIAN_POINT ( 'NONE',  ( -24.97867591359219475, -26.64985754041175525, 6.700000000000000178 ) ) ;
#28882 = CARTESIAN_POINT ( 'NONE',  ( -0.9667203403901262204, -31.67862831489078701, 7.774064877406526186 ) ) ;
#28883 = CARTESIAN_POINT ( 'NONE',  ( -73.07498068578524908, 39.58105274722134936, 9.800414904976365804 ) ) ;
#28884 = CARTESIAN_POINT ( 'NONE',  ( 2.083546779805665494, -32.94827274467561296, 6.939395833800443114 ) ) ;
#28885 = B_SPLINE_CURVE_WITH_KNOTS ( 'NONE', 3,
 ( #10129, #16314, #6459, #9737, #691, #19011, #15913, #31775, #28064, #31986 ),
 .UNSPECIFIED., .F., .F.,
 ( 4, 3, 3, 4 ),
 ( 0.0001585009270395754794, 0.0001815657551981846279, 0.0002118214035944119905, 0.0002170292169044786025 ),
 .UNSPECIFIED. ) ;
#28886 = DIRECTION ( 'NONE',  ( -0.000000000000000000, 0.000000000000000000, 1.000000000000000000 ) ) ;
#28887 = AXIS2_PLACEMENT_3D ( 'NONE', #4766, #29879, #36460 ) ;
#28888 = CARTESIAN_POINT ( 'NONE',  ( 21.85955896937255716, -14.20251193623180441, 2.500000000000000444 ) ) ;
#28889 = ADVANCED_FACE ( 'NONE', ( #37318 ), #8493, .T. ) ;
#28890 = CARTESIAN_POINT ( 'NONE',  ( 31.70306142352022505, -2.958976183629556278, 5.154427495215030852 ) ) ;
#28891 = ORIENTED_EDGE ( 'NONE', *, *, #23445, .T. ) ;
#28892 = ORIENTED_EDGE ( 'NONE', *, *, #9898, .T. ) ;
#28893 = LINE ( 'NONE', #35290, #11287 ) ;
#28894 = CARTESIAN_POINT ( 'NONE',  ( 67.78936902810559673, 58.13140593263176470, -3.993918888840292780 ) ) ;
#28895 = VERTEX_POINT ( 'NONE', #15086 ) ;
#28896 = CARTESIAN_POINT ( 'NONE',  ( -0.9779184174635926485, -27.32182954066626834, 7.767720160662275219 ) ) ;
#28897 = CARTESIAN_POINT ( 'NONE',  ( -64.08758708074093136, 38.13199975834322686, 3.043809435734686097 ) ) ;
#28898 = CARTESIAN_POINT ( 'NONE',  ( 22.39762075202990133, 3.875352353137541339, 3.942491037406270049 ) ) ;
#28899 = CARTESIAN_POINT ( 'NONE',  ( 5.048260384636090059, -28.54926152416005181, 6.921725064902950031 ) ) ;
#28900 = CARTESIAN_POINT ( 'NONE',  ( 1.104640146243424548, -26.22252062316335852, 7.763628509615288387 ) ) ;
#28901 = CARTESIAN_POINT ( 'NONE',  ( -2.348748702180637693, -25.49307895267003587, 6.700000000000000178 ) ) ;
#28902 = ORIENTED_EDGE ( 'NONE', *, *, #23184, .T. ) ;
#28903 = CARTESIAN_POINT ( 'NONE',  ( 22.61545699184745217, 4.619227728608865213, 3.050121107112468977 ) ) ;
#28904 = DIRECTION ( 'NONE',  ( -0.05950379560742589252, 0.006463183370434484251, 0.9982071556390637035 ) ) ;
#28905 = CARTESIAN_POINT ( 'NONE',  ( 81.26478070948648735, 61.47323240028521241, 1.804401104814719270 ) ) ;
#28906 = DIRECTION ( 'NONE',  ( 0.000000000000000000, 0.000000000000000000, 1.000000000000000000 ) ) ;
#28907 = ORIENTED_EDGE ( 'NONE', *, *, #12980, .T. ) ;
#28908 = CARTESIAN_POINT ( 'NONE',  ( 78.30161670990426614, 64.30707665991987199, -3.470679136763274109 ) ) ;
#28910 = CARTESIAN_POINT ( 'NONE',  ( -1.740904132959085304, -28.93157757802832819, 6.894806418505347700 ) ) ;
#28909 = CARTESIAN_POINT ( 'NONE',  ( 23.07063981287367582, 0.3569738237481424048, 5.941516061105353685 ) ) ;
#28911 = CARTESIAN_POINT ( 'NONE',  ( 78.85932765206329975, 66.13466208586149264, -1.358900964588049431 ) ) ;
#28912 = EDGE_CURVE ( 'NONE', #9101, #6453, #510, .T. ) ;
#28913 = CARTESIAN_POINT ( 'NONE',  ( 80.39617744327613025, 62.02891139109912899, 3.151254463355007918 ) ) ;
#28914 = EDGE_LOOP ( 'NONE', ( #37845, #22724, #37175, #31834 ) ) ;
#28915 = AXIS2_PLACEMENT_3D ( 'NONE', #26281, #13106, #34957 ) ;
#28916 = DIRECTION ( 'NONE',  ( -0.000000000000000000, 1.000000000000000000, 0.000000000000000000 ) ) ;
#28917 = CARTESIAN_POINT ( 'NONE',  ( 78.99916064199126708, 66.21331998952631182, 1.048259027381037267 ) ) ;
#28919 = ORIENTED_EDGE ( 'NONE', *, *, #17327, .F. ) ;
#28918 = CARTESIAN_POINT ( 'NONE',  ( -63.70768059418392681, 44.39675795296274430, 1.227925197078028052 ) ) ;
#28920 = DIRECTION ( 'NONE',  ( 0.000000000000000000, 0.000000000000000000, 1.000000000000000000 ) ) ;
#28921 = CARTESIAN_POINT ( 'NONE',  ( 23.93232801731964443, 3.995115622954060530, -2.300403959411237320 ) ) ;
#28922 = PLANE ( 'NONE',  #18693 ) ;
#28923 = ORIENTED_EDGE ( 'NONE', *, *, #5875, .T. ) ;
#28924 = CARTESIAN_POINT ( 'NONE',  ( -76.80627534794649591, -4.528701127649712888, 9.610004701533378935 ) ) ;
#28925 = CARTESIAN_POINT ( 'NONE',  ( -17.27251170661583402, -8.656638842136340273, 6.000000000000000000 ) ) ;
#28926 = ADVANCED_FACE ( 'NONE', ( #5422 ), #30545, .T. ) ;
#28927 = CARTESIAN_POINT ( 'NONE',  ( -0.03448549664302677509, -32.60970101154014600, 7.750000000000000000 ) ) ;
#28928 = CARTESIAN_POINT ( 'NONE',  ( -8.348748702180635917, -26.64985754041175525, 6.700000000000000178 ) ) ;
#28929 = AXIS2_PLACEMENT_3D ( 'NONE', #17680, #36640, #33377 ) ;
#28930 = CARTESIAN_POINT ( 'NONE',  ( 28.79870369017745446, -3.878292931925462650, -4.349375427024083862 ) ) ;
#28931 = CARTESIAN_POINT ( 'NONE',  ( 37.00971988778469068, -2.249531826949414892, -5.913225602219081445 ) ) ;
#28932 = DIRECTION ( 'NONE',  ( -1.682730792515357087E-16, 1.000000000000000000, 0.000000000000000000 ) ) ;
#28933 = CARTESIAN_POINT ( 'NONE',  ( 18.48730018318043022, 7.939472255012167246, 3.062856037497708073 ) ) ;
#28934 = CARTESIAN_POINT ( 'NONE',  ( 1.011962798722023882, -33.78603799583471101, 7.695279973900954751 ) ) ;
#28935 = FACE_OUTER_BOUND ( 'NONE', #10844, .T. ) ;
#28936 = DIRECTION ( 'NONE',  ( 0.000000000000000000, -0.7071067811865474617, -0.7071067811865474617 ) ) ;
#28937 = CARTESIAN_POINT ( 'NONE',  ( -17.69482985384421880, -29.56993018339339940, -6.000000000000000000 ) ) ;
#28938 = CARTESIAN_POINT ( 'NONE',  ( 25.45843029652522205, 1.868879512192637593, -4.233311170609479035 ) ) ;
#28939 = CARTESIAN_POINT ( 'NONE',  ( 36.01008099166774201, -1.464911901215198764, -5.613471295053200194 ) ) ;
#28940 = LINE ( 'NONE', #38589, #30832 ) ;
#28941 = EDGE_CURVE ( 'NONE', #33366, #36200, #2563, .T. ) ;
#28942 = VERTEX_POINT ( 'NONE', #21486 ) ;
#28943 = CARTESIAN_POINT ( 'NONE',  ( 66.68811621373450294, 57.96620201306357956, 3.998609561968404336 ) ) ;
#28944 = AXIS2_PLACEMENT_3D ( 'NONE', #11427, #17004, #23791 ) ;
#28945 = CARTESIAN_POINT ( 'NONE',  ( -64.08758708074093136, 38.60011822860882802, 4.018727294472848044 ) ) ;
#28946 = B_SPLINE_CURVE_WITH_KNOTS ( 'NONE', 3,
 ( #13763, #818, #35410, #7579, #4698, #20132, #11052, #35998, #29014, #3924, #16438, #35803, #20326, #19740, #7778, #16831, #22840, #4309, #6981, #26725, #17232, #23235, #29805, #1617, #26329 ),
 .UNSPECIFIED., .F., .F.,
 ( 4, 3, 3, 3, 3, 3, 3, 3, 4 ),
 ( 6.468151674593822101E-05, 9.076621574722248736E-05, 0.0001210204262067999181, 0.0001512763324577458420, 0.0001815301820994231650, 0.0002117781465860723591, 0.0002420274594459760750, 0.0002722905548971156801, 0.0002816827545175590048 ),
 .UNSPECIFIED. ) ;
#28947 = CARTESIAN_POINT ( 'NONE',  ( 86.42019152727894493, 0.2271775462534226520, 6.017476335466618309 ) ) ;
#28948 = CARTESIAN_POINT ( 'NONE',  ( 5.651251297819362307, -25.49307895267003587, 6.800000000000000711 ) ) ;
#28949 = ORIENTED_EDGE ( 'NONE', *, *, #22649, .T. ) ;
#28950 = CARTESIAN_POINT ( 'NONE',  ( -73.96100403028097503, 6.544720006936636025, -10.78617274266811776 ) ) ;
#28951 = CARTESIAN_POINT ( 'NONE',  ( 2.973605180254018432, -26.32071758304399012, 7.780491323090171996 ) ) ;
#28952 = CARTESIAN_POINT ( 'NONE',  ( 14.61802081865033642, 12.33286846116140900, 3.500000000000000444 ) ) ;
#28953 = ADVANCED_FACE ( 'NONE', ( #15292 ), #34268, .F. ) ;
#28954 = EDGE_LOOP ( 'NONE', ( #13588, #30210, #9862, #36183, #40592, #37535 ) ) ;
#28955 = DIRECTION ( 'NONE',  ( -0.000000000000000000, -0.000000000000000000, -1.000000000000000000 ) ) ;
#28956 = AXIS2_PLACEMENT_3D ( 'NONE', #9366, #38183, #32038 ) ;
#28957 = ORIENTED_EDGE ( 'NONE', *, *, #18673, .F. ) ;
#28958 = CARTESIAN_POINT ( 'NONE',  ( 78.60455099833406223, 65.79598288722390009, -2.095806625474251117 ) ) ;
#28959 = CARTESIAN_POINT ( 'NONE',  ( -1.720974470195171024, -28.90632690787352033, 7.785593909369613819 ) ) ;
#28960 = CARTESIAN_POINT ( 'NONE',  ( 79.35276748299807537, 64.76637986602914054, 3.438247877890458160 ) ) ;
#28961 = DIRECTION ( 'NONE',  ( -0.9949204587440765302, -0.1006641980670203163, -0.000000000000000000 ) ) ;
#28962 = DIRECTION ( 'NONE',  ( -0.000000000000000000, -0.000000000000000000, 1.000000000000000000 ) ) ;
#28963 = CARTESIAN_POINT ( 'NONE',  ( 0.9231601816174473951, -32.98254913520433007, 6.898188844117810525 ) ) ;
#28964 = CARTESIAN_POINT ( 'NONE',  ( -1.797258899342013549, -29.44812577374269580, 7.754798119455333705 ) ) ;
#28965 = EDGE_CURVE ( 'NONE', #9636, #34839, #38594, .T. ) ;
#28966 = EDGE_CURVE ( 'NONE', #7534, #5389, #39783, .T. ) ;
#28967 = CARTESIAN_POINT ( 'NONE',  ( 33.72876834755415842, -4.609435595580992029, -3.994862081233153006 ) ) ;
#28968 = CARTESIAN_POINT ( 'NONE',  ( 22.88108605422135966, 4.308698648288653565, -3.098481689044433551 ) ) ;
#28969 = CARTESIAN_POINT ( 'NONE',  ( -63.08758708074093136, 41.04287353446839148, 4.000000000000000000 ) ) ;
#28970 = EDGE_CURVE ( 'NONE', #40686, #9974, #16694, .T. ) ;
#28971 = VERTEX_POINT ( 'NONE', #15907 ) ;
#28972 = AXIS2_PLACEMENT_3D ( 'NONE', #33805, #27804, #36667 ) ;
#28973 = CARTESIAN_POINT ( 'NONE',  ( -0.9631319970678871023, -31.68316142368188082, 6.866852738645443210 ) ) ;
#28974 = CARTESIAN_POINT ( 'NONE',  ( -63.03213158086148837, 38.26878225442760595, -4.032857076800604901 ) ) ;
#28975 = CARTESIAN_POINT ( 'NONE',  ( -72.64415850718684453, -1.673418234781224534, -9.853848402383640348 ) ) ;
#28976 = CARTESIAN_POINT ( 'NONE',  ( 3.198709474042557233, -25.09719924859204454, 7.754798119455333705 ) ) ;
#28977 = CARTESIAN_POINT ( 'NONE',  ( -0.7036529332303063100, -33.97746366811107777, 7.754798119455333705 ) ) ;
#28978 = CARTESIAN_POINT ( 'NONE',  ( 80.35608454708177817, 64.67152608030556848, 3.471690071579478953 ) ) ;
#28979 = CARTESIAN_POINT ( 'NONE',  ( 84.10435792013542766, 3.012680099502687892, -0.4953216543819284889 ) ) ;
#28980 =( BOUNDED_CURVE ( )  B_SPLINE_CURVE ( 3, ( #20015, #39345, #1912, #33413 ),
 .UNSPECIFIED., .F., .T. ) 
 B_SPLINE_CURVE_WITH_KNOTS ( ( 4, 4 ),
 ( 4.712388980384691450, 4.860526820865776365 ),
 .UNSPECIFIED. ) 
 CURVE ( )  GEOMETRIC_REPRESENTATION_ITEM ( )  RATIONAL_B_SPLINE_CURVE ( ( 1.000000000000000000, 0.9981721009331622207, 0.9981721009331622207, 1.000000000000000000 ) ) 
 REPRESENTATION_ITEM ( '' )  );
#28981 = CARTESIAN_POINT ( 'NONE',  ( -69.92837670882107659, -65.19654454972992141, 5.916079783099617906 ) ) ;
#28982 = CARTESIAN_POINT ( 'NONE',  ( -1.273915598905741353, -27.73393014892116071, 7.771081512783704071 ) ) ;
#28983 = CARTESIAN_POINT ( 'NONE',  ( 1.700390093233090871, -29.56993018339339940, 27.90461065042423527 ) ) ;
#28984 = CARTESIAN_POINT ( 'NONE',  ( 32.83305986583096114, -0.9452946091439576870, 5.330791081253222430 ) ) ;
#28985 = CARTESIAN_POINT ( 'NONE',  ( 1.664433243520564876, -26.17012032033359148, 7.695279973900954751 ) ) ;
#28986 = CARTESIAN_POINT ( 'NONE',  ( -0.3287281863750422528, -26.84180003047303487, 6.997764925645181933 ) ) ;
#28987 = CARTESIAN_POINT ( 'NONE',  ( 2.976970822604137368, -26.41868572423151207, 7.754798119455333705 ) ) ;
#28988 = CARTESIAN_POINT ( 'NONE',  ( -1.711592984601793876, -28.75984001168768245, 7.387053503561888057 ) ) ;
#28989 = EDGE_CURVE ( 'NONE', #6547, #33368, #25384, .T. ) ;
#28990 = EDGE_LOOP ( 'NONE', ( #4561, #30593, #23846, #23275, #7173 ) ) ;
#28991 = CARTESIAN_POINT ( 'NONE',  ( 34.92978150137876270, -1.709224254641393159, 5.658035201884869636 ) ) ;
#28992 = CARTESIAN_POINT ( 'NONE',  ( -38.44874870218063734, -26.64985754041175525, 6.700000000000000178 ) ) ;
#28993 = CARTESIAN_POINT ( 'NONE',  ( 88.42181306311033495, -0.9618525881974497871, -1.725133412809377598 ) ) ;
#28994 = VERTEX_POINT ( 'NONE', #38129 ) ;
#28996 = CARTESIAN_POINT ( 'NONE',  ( -0.4155527668808552955, -26.78195783641919903, 7.011627023500181188 ) ) ;
#28995 = CARTESIAN_POINT ( 'NONE',  ( 79.68007496026339709, 65.35156779369863500, -3.108243619504652333 ) ) ;
#28997 = CARTESIAN_POINT ( 'NONE',  ( 17.97454669799173033, 51.66243977840390755, -1.000000000000000000 ) ) ;
#28998 = ORIENTED_EDGE ( 'NONE', *, *, #18334, .F. ) ;
#28999 = AXIS2_PLACEMENT_3D ( 'NONE', #7456, #26409, #20407 ) ;
#29000 = LINE ( 'NONE', #17019, #8905 ) ;
#29001 = ORIENTED_EDGE ( 'NONE', *, *, #30981, .F. ) ;
#29002 = CARTESIAN_POINT ( 'NONE',  ( -80.87788611484333501, -6.601209159344090693, 1.087894082802069562 ) ) ;
#29004 = ORIENTED_EDGE ( 'NONE', *, *, #21868, .T. ) ;
#29003 = VERTEX_POINT ( 'NONE', #3983 ) ;
#29005 = CARTESIAN_POINT ( 'NONE',  ( 81.11523045952515076, 61.59071516775626520, -2.202709653501093712 ) ) ;
#29006 = AXIS2_PLACEMENT_3D ( 'NONE', #32520, #35811, #19748 ) ;
#29007 = DIRECTION ( 'NONE',  ( 0.000000000000000000, 1.000000000000000000, 0.000000000000000000 ) ) ;
#29008 = CARTESIAN_POINT ( 'NONE',  ( 24.02675112551502323, 1.887447688529081402, 4.512062677995031024 ) ) ;
#29010 = ORIENTED_EDGE ( 'NONE', *, *, #18030, .T. ) ;
#29009 = ORIENTED_EDGE ( 'NONE', *, *, #13822, .T. ) ;
#29011 = EDGE_CURVE ( 'NONE', #4935, #36016, #24134, .T. ) ;
#29012 = ADVANCED_FACE ( 'NONE', ( #35472 ), #19005, .F. ) ;
#29013 = AXIS2_PLACEMENT_3D ( 'NONE', #14469, #30547, #2565 ) ;
#29014 = CARTESIAN_POINT ( 'NONE',  ( 0.005087639750836099595, -32.51713536024735163, 7.763628509615288387 ) ) ;
#29016 = CARTESIAN_POINT ( 'NONE',  ( 3.972814594200666960, -32.23190212178483449, 7.660770905198785563 ) ) ;
#29015 = CARTESIAN_POINT ( 'NONE',  ( 4.534317637064775752, -31.44845478432683450, 6.959317978105160840 ) ) ;
#29017 = DIRECTION ( 'NONE',  ( -0.000000000000000000, -0.000000000000000000, 1.000000000000000000 ) ) ;
#29018 = CARTESIAN_POINT ( 'NONE',  ( -64.08758708074093136, 43.24969657044037064, -2.909329950559495614 ) ) ;
#29019 = CARTESIAN_POINT ( 'NONE',  ( 72.08456622119051360, 59.97905947476213839, 3.962431611483851146 ) ) ;
#29020 = CARTESIAN_POINT ( 'NONE',  ( 22.56869731596198392, 3.964702178913764641, -3.727352237020760573 ) ) ;
#29021 = ORIENTED_EDGE ( 'NONE', *, *, #39294, .F. ) ;
#29022 = EDGE_CURVE ( 'NONE', #23047, #9808, #26794, .T. ) ;
#29023 = ORIENTED_EDGE ( 'NONE', *, *, #9203, .T. ) ;
#29024 = CARTESIAN_POINT ( 'NONE',  ( 21.85643539959778892, 8.438975622634238505, -5.206363084432100052 ) ) ;
#29025 = CARTESIAN_POINT ( 'NONE',  ( 21.86257038569385003, 3.862145465805826738, 3.386728275820227729 ) ) ;
#29026 = ORIENTED_EDGE ( 'NONE', *, *, #14099, .T. ) ;
#29027 = CARTESIAN_POINT ( 'NONE',  ( 0.4306841250506159291, -32.72395091166418979, 6.864276522220859711 ) ) ;
#29028 = CARTESIAN_POINT ( 'NONE',  ( 79.28168835805398373, 66.11151980550600626, 1.907437723464478152 ) ) ;
#29029 = CARTESIAN_POINT ( 'NONE',  ( 86.54367451126900335, 1.050056116286632646, -5.670096781828877219 ) ) ;
#29030 = VERTEX_POINT ( 'NONE', #29079 ) ;
#29031 = DIRECTION ( 'NONE',  ( -0.000000000000000000, -0.000000000000000000, -1.000000000000000000 ) ) ;
#29032 = CARTESIAN_POINT ( 'NONE',  ( -70.92837670882107659, -27.85319909218681644, 0.000000000000000000 ) ) ;
#29033 = CARTESIAN_POINT ( 'NONE',  ( 35.95092945659100536, -2.121302639717296046, 5.817410036852332489 ) ) ;
#29034 = CARTESIAN_POINT ( 'NONE',  ( 5.074422016658271417, -29.15051561556369819, 6.882085323592685988 ) ) ;
#29035 = CARTESIAN_POINT ( 'NONE',  ( 35.33511003955339902, -3.170233155793333868, -5.721296523174722815 ) ) ;
#29036 = DIRECTION ( 'NONE',  ( -0.9396926207859104263, 0.3420201433256631063, -0.000000000000000000 ) ) ;
#29037 = CARTESIAN_POINT ( 'NONE',  ( 84.10567841564332525, 3.011090578911546967, -0.2542956616254711255 ) ) ;
#29038 = CARTESIAN_POINT ( 'NONE',  ( 4.400089692731897983, -31.79740006477585368, 7.730015791551948290 ) ) ;
#29039 = CARTESIAN_POINT ( 'NONE',  ( 5.021324086407805254, -26.64985754041175525, 6.800000000000000711 ) ) ;
#29040 = CARTESIAN_POINT ( 'NONE',  ( 3.430943829990005245, -32.49656374204088394, 7.680992449362118002 ) ) ;
#29041 = AXIS2_PLACEMENT_3D ( 'NONE', #20768, #33364, #20562 ) ;
#29042 = CARTESIAN_POINT ( 'NONE',  ( 29.48001143125632240, -3.085193311930952031, 4.807466779239847554 ) ) ;
#29043 = VERTEX_POINT ( 'NONE', #19808 ) ;
#29044 = EDGE_LOOP ( 'NONE', ( #32254, #13251, #20140, #27149 ) ) ;
#29045 = CARTESIAN_POINT ( 'NONE',  ( 35.36813255412664603, -3.791872901862796130, 5.511222840556704305 ) ) ;
#29046 = CARTESIAN_POINT ( 'NONE',  ( 4.911690090265110165, -28.45299136274915952, 6.894806418505345924 ) ) ;
#29047 = CARTESIAN_POINT ( 'NONE',  ( 66.67928806435183731, 57.99078996168128697, -3.997717836774547617 ) ) ;
#29048 = ADVANCED_FACE ( 'NONE', ( #22512 ), #28465, .T. ) ;
#29049 = ORIENTED_EDGE ( 'NONE', *, *, #5523, .F. ) ;
#29050 = CARTESIAN_POINT ( 'NONE',  ( 4.959102621865235427, -28.59998551706655334, 6.988553391373221402 ) ) ;
#29051 = CARTESIAN_POINT ( 'NONE',  ( 2.281019115899110439, -26.11842600667238301, 7.655937882338900380 ) ) ;
#29052 = EDGE_LOOP ( 'NONE', ( #6736, #12328, #8676, #14847 ) ) ;
#29053 = FACE_BOUND ( 'NONE', #35117, .T. ) ;
#29054 = CARTESIAN_POINT ( 'NONE',  ( 3.852393986429853090, -32.33018136787153907, 6.867199677474203234 ) ) ;
#29055 = ORIENTED_EDGE ( 'NONE', *, *, #29741, .F. ) ;
#29056 = ADVANCED_FACE ( 'NONE', ( #3583 ), #25992, .F. ) ;
#29057 = CARTESIAN_POINT ( 'NONE',  ( 21.88221554822858295, 5.657183511159394662, 3.265289024689040254 ) ) ;
#29058 = CARTESIAN_POINT ( 'NONE',  ( 81.16398582655315863, 65.83200543430099572, -2.021051955677195533 ) ) ;
#29059 = ADVANCED_FACE ( 'NONE', ( #485 ), #6652, .F. ) ;
#29060 = CARTESIAN_POINT ( 'NONE',  ( 2.976970822604137368, -26.41868572423151207, 7.754798119455333705 ) ) ;
#29061 = VERTEX_POINT ( 'NONE', #35276 ) ;
#29062 = CARTESIAN_POINT ( 'NONE',  ( 75.58676173236689522, 62.77776356238130973, -3.642592851537363341 ) ) ;
#29064 = CARTESIAN_POINT ( 'NONE',  ( 4.379420427854822329, -27.32268977692216438, 7.767720160662274331 ) ) ;
#29063 = DIRECTION ( 'NONE',  ( -1.000000000000000000, -0.000000000000000000, -0.000000000000000000 ) ) ;
#29065 = DIRECTION ( 'NONE',  ( -0.3754033771448275214, -0.6502177225477910882, -0.6605219282605403475 ) ) ;
#29066 = CARTESIAN_POINT ( 'NONE',  ( 76.11285053945339030, 63.10974250081548576, 3.590981437842967861 ) ) ;
#29067 = ORIENTED_EDGE ( 'NONE', *, *, #36767, .T. ) ;
#29068 = CARTESIAN_POINT ( 'NONE',  ( 4.428676815068841144, -27.54101827131068347, 6.911401339314951819 ) ) ;
#29069 = EDGE_CURVE ( 'NONE', #9639, #19833, #34552, .T. ) ;
#29070 = DIRECTION ( 'NONE',  ( -0.000000000000000000, -0.000000000000000000, -1.000000000000000000 ) ) ;
#29071 = ADVANCED_FACE ( 'NONE', ( #26198 ), #30091, .F. ) ;
#29072 = CARTESIAN_POINT ( 'NONE',  ( 22.77354003839862884, 3.736677582877315995, -3.760759721776010700 ) ) ;
#29073 = CARTESIAN_POINT ( 'NONE',  ( 80.42596214810052402, 66.05751922670457077, 2.080779877698174296 ) ) ;
#29074 = CARTESIAN_POINT ( 'NONE',  ( 86.13511395365257783, 1.606676384832600224, -4.558527568769633831 ) ) ;
#29075 = CARTESIAN_POINT ( 'NONE',  ( 27.17726507492083599, 0.7866376163037266389, 5.581651230154481169 ) ) ;
#29076 = LINE ( 'NONE', #35869, #17473 ) ;
#29077 = DIRECTION ( 'NONE',  ( 1.000000000000000000, 0.000000000000000000, 0.000000000000000000 ) ) ;
#29078 = AXIS2_PLACEMENT_3D ( 'NONE', #31326, #37073, #34230 ) ;
#29079 = CARTESIAN_POINT ( 'NONE',  ( 3.419158195859356653, -26.52102280379090971, 7.695279973900954751 ) ) ;
#29080 = ORIENTED_EDGE ( 'NONE', *, *, #19715, .F. ) ;
#29081 = CARTESIAN_POINT ( 'NONE',  ( 0.7215495951242570927, -26.31387869742729890, 6.903372536218458144 ) ) ;
#29082 = CARTESIAN_POINT ( 'NONE',  ( 3.927318322983230470, -26.86978234060347503, 7.660770905198783787 ) ) ;
#29083 = CARTESIAN_POINT ( 'NONE',  ( -39.07867591359219261, -26.64985754041175525, 6.800000000000000711 ) ) ;
#29084 = CARTESIAN_POINT ( 'NONE',  ( 34.12028950839226127, -3.462206709392819715, -5.516488667911798593 ) ) ;
#29085 = CARTESIAN_POINT ( 'NONE',  ( 1.128478239259624205, -32.92148457371509807, 7.748216051605118615 ) ) ;
#29086 = CARTESIAN_POINT ( 'NONE',  ( -1.761293926603614501, -29.00920416086214360, 7.255881584735162981 ) ) ;
#29087 = CARTESIAN_POINT ( 'NONE',  ( 3.330199591572231999, -32.55385491381601071, 7.782034975670475418 ) ) ;
#29088 = DIRECTION ( 'NONE',  ( -0.5000000000000008882, 0.000000000000000000, -0.8660254037844382635 ) ) ;
#29089 = DIRECTION ( 'NONE',  ( -1.000000000000000000, 0.000000000000000000, 0.000000000000000000 ) ) ;
#29090 = CARTESIAN_POINT ( 'NONE',  ( -1.505427669403690327, -28.43735238352157424, 7.721096864323901521 ) ) ;
#29091 = CARTESIAN_POINT ( 'NONE',  ( 31.96342931950348643, -2.972543090938732036, 5.195064202404578779 ) ) ;
#29092 = ORIENTED_EDGE ( 'NONE', *, *, #27405, .F. ) ;
#29093 = CARTESIAN_POINT ( 'NONE',  ( 22.97035745888615565, 2.781248465002744474, 3.791477840290978563 ) ) ;
#29094 = LINE ( 'NONE', #25401, #20520 ) ;
#29095 = CARTESIAN_POINT ( 'NONE',  ( 68.48614864092384380, 58.93304109727553453, -3.970924506823389599 ) ) ;
#29096 = CARTESIAN_POINT ( 'NONE',  ( 3.005221404606187807, -26.32225174351355790, 6.865482280155367434 ) ) ;
#29097 = ORIENTED_EDGE ( 'NONE', *, *, #15351, .F. ) ;
#29098 = PLANE ( 'NONE',  #19326 ) ;
#29099 = DIRECTION ( 'NONE',  ( -1.000000000000000000, 0.000000000000000000, 0.000000000000000000 ) ) ;
#29100 = CARTESIAN_POINT ( 'NONE',  ( 23.92691214014465473, 2.953265760775589666, 3.829296936384404049 ) ) ;
#29101 = CARTESIAN_POINT ( 'NONE',  ( 0.9256524183181416010, -32.88049123692185560, 6.895222827070021765 ) ) ;
#29102 = CARTESIAN_POINT ( 'NONE',  ( 1.700390093233090871, -29.56993018339339940, 7.750000000000000888 ) ) ;
#29103 = CIRCLE ( 'NONE', #31109, 1.000000000000002220 ) ;
#29104 = CARTESIAN_POINT ( 'NONE',  ( -3.033070997534465185, -27.73041033019772428, 7.013842709614101167 ) ) ;
#29105 = ORIENTED_EDGE ( 'NONE', *, *, #3155, .F. ) ;
#29106 = CARTESIAN_POINT ( 'NONE',  ( 22.61499008964769430, 4.623430995783932573, 3.044749204892538863 ) ) ;
#29107 = CARTESIAN_POINT ( 'NONE',  ( 81.96779975749585390, 61.96402392828839822, -1.000000000000000000 ) ) ;
#29108 = CARTESIAN_POINT ( 'NONE',  ( 16.07163779223724731, -3.513190516767646709, 2.694550467567401686 ) ) ;
#29109 = CARTESIAN_POINT ( 'NONE',  ( 79.47520324823358351, 65.51774519012143116, 2.899379378185759748 ) ) ;
#29110 = CARTESIAN_POINT ( 'NONE',  ( -70.92837670882107659, -60.53509472482660669, 0.000000000000000000 ) ) ;
#29111 = ORIENTED_EDGE ( 'NONE', *, *, #36561, .F. ) ;
#29112 = CARTESIAN_POINT ( 'NONE',  ( 79.93789898034924590, 60.96822905336945553, -2.313798345564227255 ) ) ;
#29114 = CARTESIAN_POINT ( 'NONE',  ( 5.152478333118308385, -28.99279347164636889, 6.894806418505347700 ) ) ;
#29113 = CARTESIAN_POINT ( 'NONE',  ( 22.30438977958806035, 0.2664073136237887218, 7.087798616884243508 ) ) ;
#29115 = CARTESIAN_POINT ( 'NONE',  ( 81.20219841817447559, 64.34456771238251349, -3.243459512787965959 ) ) ;
#29116 = CARTESIAN_POINT ( 'NONE',  ( 78.12595179671936307, 65.55859174716130156, 2.108843360059416749 ) ) ;
#29117 = B_SPLINE_CURVE_WITH_KNOTS ( 'NONE', 3,
 ( #17064, #10891, #11087, #29642, #4731, #7411, #35839, #14383, #26760, #33360, #17265, #1861, #26165, #20766, #29839, #1654, #23659, #36226, #4926, #33144, #13986, #1454, #23848, #38696, #30048, #8196, #26559, #35641, #19967, #32546, #23466 ),
 .UNSPECIFIED., .F., .F.,
 ( 4, 3, 3, 3, 3, 3, 3, 3, 3, 3, 4 ),
 ( 9.697399036122160616E-19, 3.077658087705748496E-05, 6.152638666999462756E-05, 9.267501192706795166E-05, 0.0001241882240135198760, 0.0001556618703051706218, 0.0001866161554452250683, 0.0002167966385861010473, 0.0002463805737537809589, 0.0002758761370306560680, 0.0002847094172290131806 ),
 .UNSPECIFIED. ) ;
#29118 = ORIENTED_EDGE ( 'NONE', *, *, #16861, .F. ) ;
#29119 = EDGE_CURVE ( 'NONE', #16957, #23963, #8463, .T. ) ;
#29120 = DIRECTION ( 'NONE',  ( -0.000000000000000000, -1.000000000000000000, -0.000000000000000000 ) ) ;
#29121 = ADVANCED_FACE ( 'NONE', ( #14019 ), #23303, .F. ) ;
#29122 = CARTESIAN_POINT ( 'NONE',  ( 81.03660848153769791, 66.10018949144995304, 1.263752851812355305 ) ) ;
#29123 = CARTESIAN_POINT ( 'NONE',  ( -64.08758708074093136, 43.38479242966779736, 2.769427336171834675 ) ) ;
#29124 = CARTESIAN_POINT ( 'NONE',  ( 25.48535437492803624, -4.309695067542732794, -2.926019122942394191 ) ) ;
#29125 = CARTESIAN_POINT ( 'NONE',  ( -22.87867591359218977, -24.55319635012989110, 6.700000000000000178 ) ) ;
#29126 = ORIENTED_EDGE ( 'NONE', *, *, #14061, .F. ) ;
#29127 = AXIS2_PLACEMENT_3D ( 'NONE', #27274, #39416, #36348 ) ;
#29128 = CARTESIAN_POINT ( 'NONE',  ( -79.66837676813406688, -6.645208303062806188, 4.876177452525313427 ) ) ;
#29129 = CARTESIAN_POINT ( 'NONE',  ( 21.77775980223391628, 0.1997282058778115377, -8.433602713107923421 ) ) ;
#29130 = DIRECTION ( 'NONE',  ( -0.000000000000000000, -0.000000000000000000, 1.000000000000000000 ) ) ;
#29131 = CARTESIAN_POINT ( 'NONE',  ( 20.91912229527441269, 4.580706636100547513, -2.655338311533547380 ) ) ;
#29132 = CARTESIAN_POINT ( 'NONE',  ( 6.074096823854431726, -32.03256286660679564, 7.695279973900954751 ) ) ;
#29133 = CARTESIAN_POINT ( 'NONE',  ( 3.729302005315832336, -32.29821690522913258, 6.911401339314957148 ) ) ;
#29134 = DIRECTION ( 'NONE',  ( 0.000000000000000000, 0.000000000000000000, 1.000000000000000000 ) ) ;
#29135 = DIRECTION ( 'NONE',  ( 0.000000000000000000, 0.000000000000000000, 1.000000000000000000 ) ) ;
#29136 = CARTESIAN_POINT ( 'NONE',  ( 6.160593259708746494, -32.30254410566374190, 7.013842709614101167 ) ) ;
#29137 = PLANE ( 'NONE',  #13194 ) ;
#29138 = AXIS2_PLACEMENT_3D ( 'NONE', #4702, #17237, #29810 ) ;
#29139 = FACE_OUTER_BOUND ( 'NONE', #18917, .T. ) ;
#29140 = CARTESIAN_POINT ( 'NONE',  ( 22.13241655903548377, 0.4569658243204014481, -7.207667138002770812 ) ) ;
#29141 = CARTESIAN_POINT ( 'NONE',  ( 35.56739675845194881, -1.226987158729853533, -5.500502591869192770 ) ) ;
#29142 = DIRECTION ( 'NONE',  ( 0.7508067542896647018, 2.621427771679746855E-15, 0.6605219282605379050 ) ) ;
#29143 = ORIENTED_EDGE ( 'NONE', *, *, #1308, .F. ) ;
#29144 = ORIENTED_EDGE ( 'NONE', *, *, #37878, .F. ) ;
#29145 = CARTESIAN_POINT ( 'NONE',  ( 66.86134338034700875, 57.94508673653880493, 3.999594749380241510 ) ) ;
#29146 = ADVANCED_FACE ( 'NONE', ( #39131 ), #38730, .T. ) ;
#29147 = CARTESIAN_POINT ( 'NONE',  ( -72.95330471031414277, 33.71485196875532608, 21.52833696633422988 ) ) ;
#29148 = CARTESIAN_POINT ( 'NONE',  ( 84.54687988124997844, 2.467165036067117789, -3.672804150685311964 ) ) ;
#29149 = VERTEX_POINT ( 'NONE', #10526 ) ;
#29150 = CARTESIAN_POINT ( 'NONE',  ( -77.82107608900516027, 9.895938843071389712, -8.879257655445593755 ) ) ;
#29151 = B_SPLINE_CURVE_WITH_KNOTS ( 'NONE', 3,
 ( #24525, #36474, #21654, #37076, #27006, #8456, #15257, #30301, #39552, #20819 ),
 .UNSPECIFIED., .F., .F.,
 ( 4, 2, 2, 2, 4 ),
 ( 0.000000000000000000, 0.0003911417017416531365, 0.0007822834034833063815, 0.001173425105224959681, 0.001564566806966613197 ),
 .UNSPECIFIED. ) ;
#29152 = DIRECTION ( 'NONE',  ( -0.2567910337120365427, 0.7055275666422146097, 0.6605219282605377940 ) ) ;
#29153 = CARTESIAN_POINT ( 'NONE',  ( 1.075454873741154005, -26.12617409861640638, 7.750000000000000888 ) ) ;
#29154 = ORIENTED_EDGE ( 'NONE', *, *, #27798, .F. ) ;
#29155 = EDGE_CURVE ( 'NONE', #4065, #32844, #20002, .T. ) ;
#29156 = ORIENTED_EDGE ( 'NONE', *, *, #25453, .T. ) ;
#29157 = CARTESIAN_POINT ( 'NONE',  ( 80.53463578537552792, 62.06606814882641743, -3.115013800517337117 ) ) ;
#29158 = CARTESIAN_POINT ( 'NONE',  ( 37.19747299874393320, -2.841585884120807481, 5.999818732555961098 ) ) ;
#29159 = CARTESIAN_POINT ( 'NONE',  ( 79.88928440695138988, 63.65969051258275613, 3.720735635808744668 ) ) ;
#29162 = EDGE_LOOP ( 'NONE', ( #26020, #37219, #28173, #32395 ) ) ;
#29161 = CARTESIAN_POINT ( 'NONE',  ( -1.322949708848405237, -31.12539950468849526, 6.876076431790004051 ) ) ;
#29160 = MECHANICAL_DESIGN_GEOMETRIC_PRESENTATION_REPRESENTATION (  '', ( #34437 ), #25810 ) ;
#29163 = LINE ( 'NONE', #3875, #6112 ) ;
#29164 = ADVANCED_FACE ( 'NONE', ( #1293 ), #13831, .F. ) ;
#29165 = CARTESIAN_POINT ( 'NONE',  ( 0.9303581240408361763, -32.98417252488322049, 6.890920332093119605 ) ) ;
#29166 = CARTESIAN_POINT ( 'NONE',  ( 5.897691494960017877, -28.77484643370537754, 7.695279973900954751 ) ) ;
#29167 = CARTESIAN_POINT ( 'NONE',  ( 21.85643539959779247, -15.31483402087699197, 0.9306824932977513232 ) ) ;
#29168 = CARTESIAN_POINT ( 'NONE',  ( 3.378963426318634777, -26.61317069598981533, 7.740055089680407008 ) ) ;
#29169 = ORIENTED_EDGE ( 'NONE', *, *, #25587, .F. ) ;
#29170 = CARTESIAN_POINT ( 'NONE',  ( 68.47051737416747130, 59.12915321841263960, -3.950001462127424645 ) ) ;
#29171 = ORIENTED_EDGE ( 'NONE', *, *, #37500, .T. ) ;
#29172 = CARTESIAN_POINT ( 'NONE',  ( -0.9570137182916693686, -31.69082739506907842, 6.870716933885666400 ) ) ;
#29173 = LINE ( 'NONE', #38024, #35344 ) ;
#29174 = AXIS2_PLACEMENT_3D ( 'NONE', #5890, #18426, #2819 ) ;
#29175 = CARTESIAN_POINT ( 'NONE',  ( -71.81612654988926181, 3.537828150600389687, -9.960561527263866566 ) ) ;
#29176 = CARTESIAN_POINT ( 'NONE',  ( 4.713366678454989689, -27.78892706510198707, 7.698786668945011513 ) ) ;
#29177 = FACE_OUTER_BOUND ( 'NONE', #35328, .T. ) ;
#29178 = CARTESIAN_POINT ( 'NONE',  ( 80.98576866654177309, 63.46339031992857826, 3.471690071579480286 ) ) ;
#29179 = CARTESIAN_POINT ( 'NONE',  ( 86.38407091574619301, -0.4420343715668084150, 5.843987706619403255 ) ) ;
#29180 = DIRECTION ( 'NONE',  ( 1.000000000000000000, 0.000000000000000000, 0.000000000000000000 ) ) ;
#29181 = CARTESIAN_POINT ( 'NONE',  ( 2.930491328958202857, -32.84664367347161829, 7.710604733652629328 ) ) ;
#29182 = CARTESIAN_POINT ( 'NONE',  ( -2.227706725756020578, -32.93668375692303130, 7.695279973900954751 ) ) ;
#29183 = CIRCLE ( 'NONE', #16663, 0.9999999999999998890 ) ;
#29184 = CARTESIAN_POINT ( 'NONE',  ( -63.71117060422361078, 35.77969396829419679, 7.174848616057642126 ) ) ;
#29185 = CARTESIAN_POINT ( 'NONE',  ( -0.3196854658041705100, -26.83510019752340625, 6.949473656533217358 ) ) ;
#29186 = DIRECTION ( 'NONE',  ( -0.000000000000000000, -0.000000000000000000, -1.000000000000000000 ) ) ;
#29187 = FACE_OUTER_BOUND ( 'NONE', #18347, .T. ) ;
#29188 = VERTEX_POINT ( 'NONE', #15443 ) ;
#29189 = CARTESIAN_POINT ( 'NONE',  ( 32.78089741354497022, -0.9280409695437186191, 5.322649869020279922 ) ) ;
#29190 = ADVANCED_FACE ( 'NONE', ( #21637 ), #3177, .F. ) ;
#29191 = CARTESIAN_POINT ( 'NONE',  ( 4.945445480008764605, -30.88065529806472043, 7.754798119455333705 ) ) ;
#29192 = CARTESIAN_POINT ( 'NONE',  ( 86.85660104221420852, 0.7962678431171816840, 5.176869783008884340 ) ) ;
#29194 = CARTESIAN_POINT ( 'NONE',  ( -0.3987955896700752234, -26.76931963055061559, 6.951256099901585550 ) ) ;
#29193 = CARTESIAN_POINT ( 'NONE',  ( 81.18881611591316982, 61.34569122823198484, -1.520709669156494748 ) ) ;
#29195 = EDGE_CURVE ( 'NONE', #8844, #16031, #37060, .T. ) ;
#29196 = CARTESIAN_POINT ( 'NONE',  ( -1.298113860838788547, -27.76464493488661134, 6.870737987065012931 ) ) ;
#29197 = VERTEX_POINT ( 'NONE', #11726 ) ;
#29198 = CARTESIAN_POINT ( 'NONE',  ( -60.66839582778040807, 24.84364830758653397, -8.800414904976364028 ) ) ;
#29199 = ORIENTED_EDGE ( 'NONE', *, *, #33812, .F. ) ;
#29200 = CARTESIAN_POINT ( 'NONE',  ( -72.37627261349332741, -1.026670002906238333, 9.895491078337210311 ) ) ;
#29201 = EDGE_CURVE ( 'NONE', #16761, #17469, #18843, .T. ) ;
#29202 = VECTOR ( 'NONE', #16414, 1000.000000000000114 ) ;
#29203 = AXIS2_PLACEMENT_3D ( 'NONE', #11915, #2281, #14806 ) ;
#29204 = VERTEX_POINT ( 'NONE', #21224 ) ;
#29205 = CARTESIAN_POINT ( 'NONE',  ( 79.55117250774208060, 64.91534908514013580, -3.386558198656252738 ) ) ;
#29206 = DIRECTION ( 'NONE',  ( -0.000000000000000000, -0.000000000000000000, 1.000000000000000000 ) ) ;
#29207 = CARTESIAN_POINT ( 'NONE',  ( 24.35809287307254323, 1.975542649453049693, 4.376866090386280383 ) ) ;
#29208 = VERTEX_POINT ( 'NONE', #24302 ) ;
#29209 = AXIS2_PLACEMENT_3D ( 'NONE', #2434, #12056, #18241 ) ;
#29210 = DIRECTION ( 'NONE',  ( 1.000000000000000000, 0.000000000000000000, -0.000000000000000000 ) ) ;
#29211 = ADVANCED_FACE ( 'NONE', ( #15239 ), #36866, .F. ) ;
#29212 = VECTOR ( 'NONE', #7921, 1000.000000000000000 ) ;
#29213 =( BOUNDED_CURVE ( )  B_SPLINE_CURVE ( 3, ( #1946, #11166, #39583, #30131 ),
 .UNSPECIFIED., .F., .T. ) 
 B_SPLINE_CURVE_WITH_KNOTS ( ( 4, 4 ),
 ( 4.748221474220557958, 4.941946782021392259 ),
 .UNSPECIFIED. ) 
 CURVE ( )  GEOMETRIC_REPRESENTATION_ITEM ( )  RATIONAL_B_SPLINE_CURVE ( ( 1.000000000000000000, 0.9968749865767494445, 0.9968749865767494445, 1.000000000000000000 ) ) 
 REPRESENTATION_ITEM ( '' )  );
#29215 = DIRECTION ( 'NONE',  ( 1.000000000000000000, 0.000000000000000000, 0.000000000000000000 ) ) ;
#29214 = CARTESIAN_POINT ( 'NONE',  ( 4.534007133228977970, -31.44892320798883745, 6.949473656533214694 ) ) ;
#29216 = CARTESIAN_POINT ( 'NONE',  ( -1.258633014711773468, -27.89535841845185615, 7.730758795053805699 ) ) ;
#29217 = CARTESIAN_POINT ( 'NONE',  ( 72.17048485476517783, 59.77360812419138369, 3.955776929930288510 ) ) ;
#29218 = CARTESIAN_POINT ( 'NONE',  ( 22.80705867304895307, 3.513075761590381152, -3.907165907269140703 ) ) ;
#29219 = VERTEX_POINT ( 'NONE', #2098 ) ;
#29220 = CARTESIAN_POINT ( 'NONE',  ( 2.325325312725053717, -33.01368626817038887, 7.750000000000001776 ) ) ;
#29221 = ORIENTED_EDGE ( 'NONE', *, *, #35353, .F. ) ;
#29222 = CARTESIAN_POINT ( 'NONE',  ( 21.85643539959780313, 0.1435845899245215551, -12.62009698158557747 ) ) ;
#29223 = CARTESIAN_POINT ( 'NONE',  ( 20.05068032855264448, 11.88301801997804397, 1.993596777106166673 ) ) ;
#29224 = VERTEX_POINT ( 'NONE', #11933 ) ;
#29225 = CARTESIAN_POINT ( 'NONE',  ( 0.4019100156039143723, -32.71221430294721699, 6.868387053540520704 ) ) ;
#29226 = CARTESIAN_POINT ( 'NONE',  ( 80.36688112369847659, 65.40474626847709771, 3.015199126130975404 ) ) ;
#29227 = CARTESIAN_POINT ( 'NONE',  ( 86.10913233486274976, 1.283334762834210441, -5.698406565159564785 ) ) ;
#29228 = CARTESIAN_POINT ( 'NONE',  ( -1.784555172093402531, -29.51764096169078755, 7.785373291296188825 ) ) ;
#29229 = ORIENTED_EDGE ( 'NONE', *, *, #26554, .T. ) ;
#29230 = B_SPLINE_CURVE_WITH_KNOTS ( 'NONE', 3,
 ( #37471, #4535, #38891, #35435, #35631, #38485, #35831, #10288, #17258, #17058 ),
 .UNSPECIFIED., .F., .F.,
 ( 4, 3, 3, 4 ),
 ( 1.939479807224432123E-18, 3.025570593002944284E-05, 6.051145698343964594E-05, 6.468151674593845140E-05 ),
 .UNSPECIFIED. ) ;
#29231 = EDGE_CURVE ( 'NONE', #6802, #32211, #4798, .T. ) ;
#29232 = CARTESIAN_POINT ( 'NONE',  ( 21.52073695273352882, -2.639896720919388873, 3.565229501100848353 ) ) ;
#29233 = AXIS2_PLACEMENT_3D ( 'NONE', #8459, #36479, #14843 ) ;
#29234 = CIRCLE ( 'NONE', #29892, 3.000000000000002665 ) ;
#29235 = CARTESIAN_POINT ( 'NONE',  ( 32.03545946682555723, -3.767761596829544146, 4.810237983490988967 ) ) ;
#29236 = CARTESIAN_POINT ( 'NONE',  ( 14.78316203198160039, -5.958431814372524116, -2.513667985851932407 ) ) ;
#29237 = CARTESIAN_POINT ( 'NONE',  ( 35.78601669305616184, -3.163418368850383189, -5.791671411672478342 ) ) ;
#29238 =( REPRESENTATION_RELATIONSHIP ('NONE','NONE', #24012, #28236 ) REPRESENTATION_RELATIONSHIP_WITH_TRANSFORMATION ( #39612 )SHAPE_REPRESENTATION_RELATIONSHIP( ) );
#29239 = CARTESIAN_POINT ( 'NONE',  ( 84.59056625886891823, 2.408269107882004878, 3.818220528950529324 ) ) ;
#29240 = CARTESIAN_POINT ( 'NONE',  ( -42.83131703149249603, -27.06993018339339585, 6.000000000000000000 ) ) ;
#29241 = AXIS2_PLACEMENT_3D ( 'NONE', #19156, #5993, #22266 ) ;
#29242 = DIRECTION ( 'NONE',  ( -0.7660444431189725734, -0.6427876096865456912, -0.000000000000000000 ) ) ;
#29243 = DIRECTION ( 'NONE',  ( -0.000000000000000000, -0.000000000000000000, -1.000000000000000000 ) ) ;
#29244 = ORIENTED_EDGE ( 'NONE', *, *, #35911, .T. ) ;
#29245 = EDGE_LOOP ( 'NONE', ( #18775, #40071, #11694, #23585, #843, #6717 ) ) ;
#29246 = CARTESIAN_POINT ( 'NONE',  ( 37.18669192317609884, -2.963439294260284296, 6.000022183381657825 ) ) ;
#29247 = DIRECTION ( 'NONE',  ( 0.6427876096865379196, 0.7660444431189792347, -0.000000000000000000 ) ) ;
#29248 = EDGE_CURVE ( 'NONE', #908, #1323, #9499, .T. ) ;
#29249 = EDGE_CURVE ( 'NONE', #33448, #11999, #33063, .T. ) ;
#29250 = CARTESIAN_POINT ( 'NONE',  ( 66.27376694609004915, 57.73522568913436004, -4.000000000000000000 ) ) ;
#29251 = CARTESIAN_POINT ( 'NONE',  ( 87.38843002206890276, -1.854803145455693913, 3.937212981888271734 ) ) ;
#29252 = ADVANCED_FACE ( 'NONE', ( #3734 ), #20069, .F. ) ;
#29253 = ORIENTED_EDGE ( 'NONE', *, *, #26189, .F. ) ;
#29254 = CARTESIAN_POINT ( 'NONE',  ( 4.926049798472932117, -28.49512058795590264, 6.866852738645443210 ) ) ;
#29255 = ORIENTED_EDGE ( 'NONE', *, *, #20360, .T. ) ;
#29256 = CARTESIAN_POINT ( 'NONE',  ( 33.45749450797183044, -3.829747548865578555, 5.093667367007288505 ) ) ;
#29257 = ORIENTED_EDGE ( 'NONE', *, *, #30318, .T. ) ;
#29258 = CARTESIAN_POINT ( 'NONE',  ( 82.20862031248746860, 64.47799227860153337, -2.164558651854042282 ) ) ;
#29259 = VECTOR ( 'NONE', #32835, 1000.000000000000000 ) ;
#29260 = AXIS2_PLACEMENT_3D ( 'NONE', #36014, #1631, #14171 ) ;
#29261 = CARTESIAN_POINT ( 'NONE',  ( -1.314126787848640898, -31.34832920763589570, 7.720710062488891801 ) ) ;
#29262 = VERTEX_POINT ( 'NONE', #18737 ) ;
#29263 = CARTESIAN_POINT ( 'NONE',  ( 74.98537949548503434, 62.60475170799649192, -3.615102801931181276 ) ) ;
#29264 = VECTOR ( 'NONE', #2573, 1000.000000000000000 ) ;
#29266 = CARTESIAN_POINT ( 'NONE',  ( 1.651251297819358754, -25.49307895267003587, 6.800000000000000711 ) ) ;
#29265 = CARTESIAN_POINT ( 'NONE',  ( 2.405371579693568407, -26.14164967438523135, 6.863654226668488789 ) ) ;
#29267 = CARTESIAN_POINT ( 'NONE',  ( 4.273337484900067373, -31.79252814967387053, 6.894806418505345036 ) ) ;
#29268 = CARTESIAN_POINT ( 'NONE',  ( 75.18153624412201452, 63.60369824193129773, 2.950589020697209186 ) ) ;
#29269 = ORIENTED_EDGE ( 'NONE', *, *, #8966, .F. ) ;
#29270 = FACE_OUTER_BOUND ( 'NONE', #4677, .T. ) ;
#29271 = CIRCLE ( 'NONE', #11486, 7.999999999999992895 ) ;
#29272 = CARTESIAN_POINT ( 'NONE',  ( 1.759798022315843147, -26.08531033596018389, 7.785593909369613819 ) ) ;
#29273 = CARTESIAN_POINT ( 'NONE',  ( 1.433369704655312438, -26.07330752179259292, 7.501983001166817822 ) ) ;
#29274 = CARTESIAN_POINT ( 'NONE',  ( -70.92837670882107659, 26.72470171467712063, -6.406751979251626317 ) ) ;
#29275 = CARTESIAN_POINT ( 'NONE',  ( 80.02452723347246888, 66.12521016146376951, 2.110636331688408696 ) ) ;
#29276 = CARTESIAN_POINT ( 'NONE',  ( -0.2125075820087856115, -32.50094215169137613, 6.971170733404105313 ) ) ;
#29277 = CARTESIAN_POINT ( 'NONE',  ( 27.90799128822289177, 2.452171383980988661, -2.014541967423249424 ) ) ;
#29278 = CARTESIAN_POINT ( 'NONE',  ( 2.649739443830540608, -24.89739049809065818, 6.954324564059724878 ) ) ;
#29279 = CARTESIAN_POINT ( 'NONE',  ( 3.576146456961454057, -26.73416960394870046, 6.929923840112063971 ) ) ;
#29280 = CARTESIAN_POINT ( 'NONE',  ( -79.82037350764412054, -5.590114488123880676, -6.712154371197549985 ) ) ;
#29281 = CARTESIAN_POINT ( 'NONE',  ( 0.7014528802153003895, -26.31998796168418053, 6.882085323592685100 ) ) ;
#29282 = CARTESIAN_POINT ( 'NONE',  ( 3.936673369916530607, -26.87752597194292647, 7.640616322432101981 ) ) ;
#29283 = CARTESIAN_POINT ( 'NONE',  ( 35.80541780769373617, -3.523238331632154274, -5.749476952422626574 ) ) ;
#29284 = CARTESIAN_POINT ( 'NONE',  ( 1.030866757825423585, -32.90337049350075915, 7.782034975670476307 ) ) ;
#29285 = CARTESIAN_POINT ( 'NONE',  ( 4.981688893911533356, -28.35210424544084518, 7.743886751744251562 ) ) ;
#29286 = DIRECTION ( 'NONE',  ( -0.4826092789263555782, -0.5751513419797993354, 0.6605219282605380160 ) ) ;
#29287 = CARTESIAN_POINT ( 'NONE',  ( 2.227179720685508180, -32.92888163115070199, 6.880147297696980857 ) ) ;
#29288 = EDGE_CURVE ( 'NONE', #7364, #6802, #26186, .T. ) ;
#29289 = CARTESIAN_POINT ( 'NONE',  ( 22.04556973325361113, -11.44728196981451696, -2.500000000000000000 ) ) ;
#29290 = AXIS2_PLACEMENT_3D ( 'NONE', #18071, #30239, #14777 ) ;
#29291 = CYLINDRICAL_SURFACE ( 'NONE', #18459, 0.1000000000000028644 ) ;
#29292 = CIRCLE ( 'NONE', #18096, 7.744449365083023729 ) ;
#29293 = EDGE_CURVE ( 'NONE', #14158, #9863, #25195, .T. ) ;
#29294 = LINE ( 'NONE', #38742, #36050 ) ;
#29295 = ORIENTED_EDGE ( 'NONE', *, *, #26328, .T. ) ;
#29296 = CARTESIAN_POINT ( 'NONE',  ( 34.77027720814614042, -3.601453098587749313, 5.565789519727438517 ) ) ;
#29297 = LINE ( 'NONE', #1111, #8682 ) ;
#29298 = CARTESIAN_POINT ( 'NONE',  ( 67.11883677231543288, 58.14904800069622581, -3.997022163556062324 ) ) ;
#29299 = EDGE_CURVE ( 'NONE', #6054, #17262, #32742, .T. ) ;
#29300 = FACE_BOUND ( 'NONE', #38400, .T. ) ;
#29301 = ORIENTED_EDGE ( 'NONE', *, *, #40713, .T. ) ;
#29302 = LINE ( 'NONE', #1115, #27891 ) ;
#29303 = CARTESIAN_POINT ( 'NONE',  ( -1.600641465967917121, -28.40666295028739796, 7.698786668945015066 ) ) ;
#29304 = CARTESIAN_POINT ( 'NONE',  ( 23.70161070757133359, 3.021634694769598450, 3.856184811640798848 ) ) ;
#29305 = CARTESIAN_POINT ( 'NONE',  ( 0.9326639148157755965, -32.88212908196953776, 6.887945620086118659 ) ) ;
#29306 = CARTESIAN_POINT ( 'NONE',  ( 0.4300623547519256684, -32.83125927393997046, 6.866770815808350470 ) ) ;
#29307 = CARTESIAN_POINT ( 'NONE',  ( -55.62677557291493713, 30.95433239688069804, 1.979412988903658022 ) ) ;
#29308 = VERTEX_POINT ( 'NONE', #31717 ) ;
#29309 = CARTESIAN_POINT ( 'NONE',  ( 4.945063611787737123, -30.88201195410851696, 7.753200566781576875 ) ) ;
#29310 = CARTESIAN_POINT ( 'NONE',  ( 81.23328907848380709, 61.46306935600725296, 1.830101370957705642 ) ) ;
#29311 = CARTESIAN_POINT ( 'NONE',  ( -36.87867591359218977, -26.64985754041175525, 6.700000000000000178 ) ) ;
#29312 = VERTEX_POINT ( 'NONE', #3338 ) ;
#29313 = CARTESIAN_POINT ( 'NONE',  ( 78.12595179671936307, 65.55859174716130156, -2.108843360059416749 ) ) ;
#29315 = CARTESIAN_POINT ( 'NONE',  ( 14.61802081865040748, -4.461995682952455411, -2.500000000000015987 ) ) ;
#29314 = CARTESIAN_POINT ( 'NONE',  ( 27.42275297525273814, 1.007386247029351978, 4.486341073878296726 ) ) ;
#29316 = CARTESIAN_POINT ( 'NONE',  ( 80.45827632841502464, 65.09029793562378075, -3.202775791559303808 ) ) ;
#29317 = CARTESIAN_POINT ( 'NONE',  ( 78.47217392918747692, 65.00024052541876074, 3.055712048904924760 ) ) ;
#29318 = CIRCLE ( 'NONE', #7587, 7.999999999999986677 ) ;
#29319 = CARTESIAN_POINT ( 'NONE',  ( -12.99139449055068241, 13.37661300689600097, 6.000000000000000000 ) ) ;
#29320 = AXIS2_PLACEMENT_3D ( 'NONE', #11955, #24117, #20827 ) ;
#29321 = CARTESIAN_POINT ( 'NONE',  ( 79.00097698949592484, 66.21430696267364624, 1.024355359505926488 ) ) ;
#29322 = DIRECTION ( 'NONE',  ( 0.000000000000000000, 0.000000000000000000, 1.000000000000000000 ) ) ;
#29323 = CARTESIAN_POINT ( 'NONE',  ( 22.37806265499392566, 3.168015787195890720, 7.828147373443384183 ) ) ;
#29324 = CARTESIAN_POINT ( 'NONE',  ( -64.43126815475758917, 34.69310041339028317, -5.627269573384313439 ) ) ;
#29325 = ORIENTED_EDGE ( 'NONE', *, *, #19143, .T. ) ;
#29326 = CARTESIAN_POINT ( 'NONE',  ( -80.34222039028743723, -6.644459708051462243, 3.397825296345740043 ) ) ;
#29327 = CARTESIAN_POINT ( 'NONE',  ( 0.06066625181903905623, -26.47779407321028700, 7.750000000000000888 ) ) ;
#29328 = AXIS2_PLACEMENT_3D ( 'NONE', #14463, #39582, #23934 ) ;
#29329 = CARTESIAN_POINT ( 'NONE',  ( -0.07364990749213512489, -32.57193750258057463, 7.783750581861597517 ) ) ;
#29330 = CYLINDRICAL_SURFACE ( 'NONE', #31532, 3.399999999999999911 ) ;
#29331 = CARTESIAN_POINT ( 'NONE',  ( 34.14217736537160164, -3.847370433800512135, -5.235592723209181898 ) ) ;
#29332 = CARTESIAN_POINT ( 'NONE',  ( 30.73796255296185365, -3.302600333584832626, -4.965265549407608781 ) ) ;
#29333 = CARTESIAN_POINT ( 'NONE',  ( 3.287517435274415423, -32.68939094274560375, 6.989977667959440311 ) ) ;
#29334 = CARTESIAN_POINT ( 'NONE',  ( -1.010232243575984068, -31.78411342390880634, 6.880608371227946662 ) ) ;
#29335 = CARTESIAN_POINT ( 'NONE',  ( 5.196998877152752883, -29.72423992874466947, 6.880828092187092793 ) ) ;
#29336 = CARTESIAN_POINT ( 'NONE',  ( -0.4475183596422435683, -26.93431084857535751, 6.894806418505348589 ) ) ;
#29337 = FACE_OUTER_BOUND ( 'NONE', #30922, .T. ) ;
#29338 = CARTESIAN_POINT ( 'NONE',  ( 1.881046931064791927, -26.07459083023339019, 6.998987538705434552 ) ) ;
#29339 = CARTESIAN_POINT ( 'NONE',  ( 14.77315594796849574, 13.19392823276453441, -2.500000000000005773 ) ) ;
#29340 = ORIENTED_EDGE ( 'NONE', *, *, #14720, .T. ) ;
#29341 = ORIENTED_EDGE ( 'NONE', *, *, #11596, .F. ) ;
#29342 = CARTESIAN_POINT ( 'NONE',  ( 66.81810912255278367, 58.06508983445694128, 3.996770903032645261 ) ) ;
#29343 = EDGE_CURVE ( 'NONE', #17770, #1874, #35227, .T. ) ;
#29344 = EDGE_CURVE ( 'NONE', #13934, #28626, #28413, .T. ) ;
#29345 = CARTESIAN_POINT ( 'NONE',  ( 21.73878006178032507, 6.093844739303823310, -3.276015879424795330 ) ) ;
#29346 = CARTESIAN_POINT ( 'NONE',  ( 85.28131701390645958, 1.700283277630491030, -5.218886290300497777 ) ) ;
#29347 = EDGE_CURVE ( 'NONE', #23963, #2909, #33594, .T. ) ;
#29348 = AXIS2_PLACEMENT_3D ( 'NONE', #24850, #8360, #33520 ) ;
#29349 = ORIENTED_EDGE ( 'NONE', *, *, #7219, .T. ) ;
#29350 = CARTESIAN_POINT ( 'NONE',  ( -78.73873693005447194, 10.21307840320916860, -8.022592256280697498 ) ) ;
#29351 = DIRECTION ( 'NONE',  ( 0.000000000000000000, 0.000000000000000000, 1.000000000000000000 ) ) ;
#29352 = CARTESIAN_POINT ( 'NONE',  ( 2.926185339781475658, -26.30547128762431441, 7.783750581861601070 ) ) ;
#29353 = CYLINDRICAL_SURFACE ( 'NONE', #16099, 0.09010775117052885475 ) ;
#29354 = ORIENTED_EDGE ( 'NONE', *, *, #32103, .F. ) ;
#29355 = CARTESIAN_POINT ( 'NONE',  ( 5.909439403370450705, -28.84147213309200808, 7.635761828346577573 ) ) ;
#29356 = VERTEX_POINT ( 'NONE', #9685 ) ;
#29357 = AXIS2_PLACEMENT_3D ( 'NONE', #4166, #35662, #20584 ) ;
#29358 = CARTESIAN_POINT ( 'NONE',  ( 79.98443850338786376, 63.35773072451035404, -3.725738571856551662 ) ) ;
#29359 = CARTESIAN_POINT ( 'NONE',  ( 14.72270832792595030, 13.21629034704322336, -2.500000000000005773 ) ) ;
#29360 = CARTESIAN_POINT ( 'NONE',  ( 80.35827824124314134, 62.85331387716630758, 3.547878946066059136 ) ) ;
#29361 = DIRECTION ( 'NONE',  ( 0.1006641980670203301, -0.9949204587440765302, 0.000000000000000000 ) ) ;
#29362 = CARTESIAN_POINT ( 'NONE',  ( 3.462070670749302970, -32.59424523688933562, 7.635761828346575797 ) ) ;
#29363 = CARTESIAN_POINT ( 'NONE',  ( 1.050200036002242765, -33.00901471541564547, 6.883108633650832253 ) ) ;
#29364 = CARTESIAN_POINT ( 'NONE',  ( -1.784512137809761700, -29.51577928193536593, 7.785387725071483800 ) ) ;
#29365 = CARTESIAN_POINT ( 'NONE',  ( 33.84040353105311283, -5.117034793841976459, -2.696338666777271076 ) ) ;
#29366 = CARTESIAN_POINT ( 'NONE',  ( 3.395692546715378679, -26.62272500653946850, 7.763628509615292828 ) ) ;
#29367 = CARTESIAN_POINT ( 'NONE',  ( 21.83032690866058800, 5.963236517223874600, -3.135749234919836148 ) ) ;
#29368 = VERTEX_POINT ( 'NONE', #19572 ) ;
#29369 = CARTESIAN_POINT ( 'NONE',  ( 78.69038500580364826, 66.05859403932464602, -1.083708649521440526 ) ) ;
#29370 = ORIENTED_EDGE ( 'NONE', *, *, #37764, .T. ) ;
#29371 = CARTESIAN_POINT ( 'NONE',  ( -1.772710793196472290, -30.00307800544500125, 6.903112506833892326 ) ) ;
#29372 = CARTESIAN_POINT ( 'NONE',  ( -0.6241997385101580864, -32.18023142865752817, 7.771081512783688972 ) ) ;
#29373 = CARTESIAN_POINT ( 'NONE',  ( -74.60868374468475395, -4.441676580721787282, -9.303113757966089636 ) ) ;
#29374 = CARTESIAN_POINT ( 'NONE',  ( -0.01129010125266571157, -26.63221833370405633, 7.635761828346577573 ) ) ;
#29375 = LINE ( 'NONE', #7146, #12925 ) ;
#29376 = CARTESIAN_POINT ( 'NONE',  ( 79.60946285158566127, 65.60230831631017168, 2.836177733672696988 ) ) ;
#29377 = CARTESIAN_POINT ( 'NONE',  ( 17.04338035915418459, 48.81061067247630092, 1.000000000000000000 ) ) ;
#29378 = CARTESIAN_POINT ( 'NONE',  ( 3.931771986221714421, -27.00459690141179436, 7.785172627573962778 ) ) ;
#29379 = CARTESIAN_POINT ( 'NONE',  ( -80.19065981525227471, 31.27226540113728248, 8.800414904976364028 ) ) ;
#29380 = CARTESIAN_POINT ( 'NONE',  ( -32.24874870218063450, -26.64985754041175525, 6.700000000000000178 ) ) ;
#29381 = AXIS2_PLACEMENT_3D ( 'NONE', #25006, #25816, #34704 ) ;
#29382 = VECTOR ( 'NONE', #31663, 1000.000000000000114 ) ;
#29383 = AXIS2_PLACEMENT_3D ( 'NONE', #33497, #20491, #23782 ) ;
#29384 = ORIENTED_EDGE ( 'NONE', *, *, #29155, .T. ) ;
#29385 = CARTESIAN_POINT ( 'NONE',  ( -63.84700662236109281, 35.83977057131359345, 7.343444254794666115 ) ) ;
#29386 = DIRECTION ( 'NONE',  ( -1.000000000000000000, 0.000000000000000000, 0.000000000000000000 ) ) ;
#29387 = DIRECTION ( 'NONE',  ( 1.000000000000000000, 0.000000000000000000, 0.000000000000000000 ) ) ;
#29388 = DIRECTION ( 'NONE',  ( 0.7660444431189800119, -0.6427876096865369204, 0.000000000000000000 ) ) ;
#29389 = FACE_OUTER_BOUND ( 'NONE', #13781, .T. ) ;
#29390 = CARTESIAN_POINT ( 'NONE',  ( 69.27779986746136842, 58.60568623525134768, 3.981537309218750487 ) ) ;
#29391 = CARTESIAN_POINT ( 'NONE',  ( 36.78945405456298801, -3.041985858871208315, 5.948282080159894569 ) ) ;
#29392 = DIRECTION ( 'NONE',  ( 0.000000000000000000, 0.000000000000000000, 1.000000000000000000 ) ) ;
#29393 = CARTESIAN_POINT ( 'NONE',  ( 85.75411537215676105, 2.034632074852215311, 4.270953678727185121 ) ) ;
#29394 = EDGE_CURVE ( 'NONE', #4265, #20273, #22055, .T. ) ;
#29396 = CARTESIAN_POINT ( 'NONE',  ( -0.4678273493351438606, -26.82239709254809412, 6.863784140767622333 ) ) ;
#29395 = CARTESIAN_POINT ( 'NONE',  ( 78.85897125043997846, 66.02047811250265852, -1.830101370957685880 ) ) ;
#29397 = DIRECTION ( 'NONE',  ( 7.051707954578238605E-15, 0.9905719730872860618, 0.1369933068947565835 ) ) ;
#29398 = CARTESIAN_POINT ( 'NONE',  ( 2.301917618511796437, -26.12340203079047285, 7.762796336881262249 ) ) ;
#29399 = ORIENTED_EDGE ( 'NONE', *, *, #29643, .T. ) ;
#29400 = LINE ( 'NONE', #3359, #33804 ) ;
#29401 = CARTESIAN_POINT ( 'NONE',  ( -6.878675913592188884, -26.64985754041175525, 6.700000000000000178 ) ) ;
#29402 = VERTEX_POINT ( 'NONE', #6610 ) ;
#29403 = DIRECTION ( 'NONE',  ( 0.000000000000000000, 1.000000000000000000, 0.000000000000000000 ) ) ;
#29404 = CIRCLE ( 'NONE', #11617, 3.499999999999999556 ) ;
#29405 = VERTEX_POINT ( 'NONE', #19365 ) ;
#29406 = B_SPLINE_CURVE_WITH_KNOTS ( 'NONE', 3,
 ( #19968, #4146, #1060, #16661 ),
 .UNSPECIFIED., .F., .F.,
 ( 4, 4 ),
 ( 0.000000000000000000, 6.391136169993149426E-06 ),
 .UNSPECIFIED. ) ;
#29407 = EDGE_LOOP ( 'NONE', ( #27971, #19974, #4943, #34828, #1162 ) ) ;
#29408 = CARTESIAN_POINT ( 'NONE',  ( 81.06165217645960297, 61.41816154915739645, -1.973779052376056775 ) ) ;
#29409 = CIRCLE ( 'NONE', #23501, 6.329987104167475565 ) ;
#29410 = CARTESIAN_POINT ( 'NONE',  ( -14.44874870218064089, -26.64985754041175525, 6.800000000000000711 ) ) ;
#29411 = AXIS2_PLACEMENT_3D ( 'NONE', #25790, #16503, #35077 ) ;
#29412 = CARTESIAN_POINT ( 'NONE',  ( 78.67172310627759657, 65.99640245491993085, 1.621665796799045101 ) ) ;
#29413 = CARTESIAN_POINT ( 'NONE',  ( 21.86392410096259198, 0.3939289551572383030, 7.936696350653804188 ) ) ;
#29414 = EDGE_LOOP ( 'NONE', ( #37459, #20996, #22289, #25903 ) ) ;
#29415 = VECTOR ( 'NONE', #14846, 1000.000000000000000 ) ;
#29416 = DIRECTION ( 'NONE',  ( 0.000000000000000000, -0.000000000000000000, -1.000000000000000000 ) ) ;
#29418 = CARTESIAN_POINT ( 'NONE',  ( 3.969400716823472841, -32.23481756830559419, 7.651421919295147589 ) ) ;
#29417 = CARTESIAN_POINT ( 'NONE',  ( -58.80557074721224353, 28.82763571155858173, -5.859597094982712306 ) ) ;
#29419 = LINE ( 'NONE', #16441, #5375 ) ;
#29420 = DIRECTION ( 'NONE',  ( 1.000000000000000000, 0.000000000000000000, 0.000000000000000000 ) ) ;
#29421 = EDGE_CURVE ( 'NONE', #12828, #30228, #40027, .T. ) ;
#29422 = CARTESIAN_POINT ( 'NONE',  ( 24.24423223564896546, 3.110186912964516548, -3.522988159190304280 ) ) ;
#29423 = ORIENTED_EDGE ( 'NONE', *, *, #23032, .T. ) ;
#29424 = DIRECTION ( 'NONE',  ( -1.000000000000000000, 0.000000000000000000, 0.000000000000000000 ) ) ;
#29425 = CARTESIAN_POINT ( 'NONE',  ( 22.33830324658017830, 5.012815666754769417, -5.469126444728273029 ) ) ;
#29426 = CARTESIAN_POINT ( 'NONE',  ( 21.85970433026865223, 3.598116536247359498, -3.919871293595560413 ) ) ;
#29427 = CARTESIAN_POINT ( 'NONE',  ( 4.041943119853272037, -26.96886997397920638, 7.754798119455333705 ) ) ;
#29428 = CARTESIAN_POINT ( 'NONE',  ( 79.25461589594502243, 66.09583247779279702, 1.930361577756013691 ) ) ;
#29429 = B_SPLINE_CURVE_WITH_KNOTS ( 'NONE', 3,
 ( #29774, #39434, #24207, #1796, #1591, #36769, #21133, #14122, #14941, #33700, #5479, #40058, #26699, #39235, #11023, #11225, #23792, #36367, #8136, #20706, #5075, #17604, #2004, #14524, #27810, #37287, #37678, #31736, #2736, #12379, #22071, #21658, #12165, #37892, #12779, #10445, #1009, #31534, #34642, #18969, #19921, #31127, #28432, #22278, #34847, #24738, #15875, #7363, #6007, #28643, #240, #9080, #6416 ),
 .UNSPECIFIED., .F., .F.,
 ( 4, 1, 2, 2, 1, 1, 1, 1, 2, 2, 1, 1, 1, 1, 1, 2, 2, 1, 1, 1, 1, 2, 2, 1, 1, 1, 1, 1, 2, 2, 1, 1, 1, 1, 1, 1, 2, 2, 4 ),
 ( 0.5000000000000000000, 0.5312500000000078826, 0.5351562500000083267, 0.5390625000000087708, 0.5468750000000084377, 0.5546875000000081046, 0.5585937500000075495, 0.5605468750000069944, 0.5615234375000062172, 0.5625000000000054401, 0.5937500000000077716, 0.6093750000000086597, 0.6171875000000089928, 0.6210937500000092149, 0.6230468750000091038, 0.6240234375000089928, 0.6250000000000089928, 0.6875000000000114353, 0.7187500000000128786, 0.7343750000000134337, 0.7421875000000137668, 0.7460937500000138778, 0.7500000000000139888, 0.8125000000000164313, 0.8437500000000177636, 0.8593750000000184297, 0.8671875000000188738, 0.8710937500000190958, 0.8730468750000193179, 0.8750000000000196509, 0.9062500000000235367, 0.9218750000000255351, 0.9296875000000268674, 0.9335937500000273115, 0.9355468750000275335, 0.9365234375000272005, 0.9370117187500273115, 0.9375000000000275335, 1.000000000000000000 ),
 .UNSPECIFIED. ) ;
#29430 = DIRECTION ( 'NONE',  ( 0.000000000000000000, 0.000000000000000000, 1.000000000000000000 ) ) ;
#29431 = ORIENTED_EDGE ( 'NONE', *, *, #9953, .T. ) ;
#29432 = FACE_OUTER_BOUND ( 'NONE', #10401, .T. ) ;
#29433 = EDGE_CURVE ( 'NONE', #38404, #1672, #15863, .T. ) ;
#29434 = AXIS2_PLACEMENT_3D ( 'NONE', #3079, #34974, #9406 ) ;
#29435 = CARTESIAN_POINT ( 'NONE',  ( 32.47467932546493330, -3.787890779724774948, 4.892967751047994973 ) ) ;
#29436 = FACE_OUTER_BOUND ( 'NONE', #37494, .T. ) ;
#29437 = CARTESIAN_POINT ( 'NONE',  ( 33.62755378216321844, -1.232175040594724713, -5.454791071804911518 ) ) ;
#29438 = DIRECTION ( 'NONE',  ( 0.000000000000000000, 0.000000000000000000, 1.000000000000000000 ) ) ;
#29439 = CARTESIAN_POINT ( 'NONE',  ( -58.99872204295123623, 28.48507918597134037, -46.17089178453873188 ) ) ;
#29440 = PRODUCT_DEFINITION_FORMATION_WITH_SPECIFIED_SOURCE ( 'ANY', '', #30290, .NOT_KNOWN. ) ;
#29441 = CARTESIAN_POINT ( 'NONE',  ( 30.20718958106393615, -3.692124001418715551, -4.611238308815850395 ) ) ;
#29442 = DIRECTION ( 'NONE',  ( 0.000000000000000000, 0.000000000000000000, 1.000000000000000000 ) ) ;
#29443 = CARTESIAN_POINT ( 'NONE',  ( -1.643585222189360984, -30.18463677254168331, 7.740055089680399014 ) ) ;
#29444 = CARTESIAN_POINT ( 'NONE',  ( -26.24874870218063450, -26.64985754041175525, 6.700000000000000178 ) ) ;
#29445 = EDGE_CURVE ( 'NONE', #29149, #39054, #37667, .T. ) ;
#29446 = EDGE_LOOP ( 'NONE', ( #23463, #12358, #22267, #40434 ) ) ;
#29447 = ORIENTED_EDGE ( 'NONE', *, *, #9667, .F. ) ;
#29448 = CARTESIAN_POINT ( 'NONE',  ( 35.22017179206324755, -1.048857254921915949, 5.412365112790203270 ) ) ;
#29449 = CARTESIAN_POINT ( 'NONE',  ( 15.01262998282573946, -3.946207525411958184, 2.549482009284877115 ) ) ;
#29450 = CARTESIAN_POINT ( 'NONE',  ( 2.926619159346142141, -26.29176571567377607, 6.894806418505347700 ) ) ;
#29451 = CARTESIAN_POINT ( 'NONE',  ( 86.73589842370522263, -0.9811105784606377611, 5.402284631838752738 ) ) ;
#29452 = EDGE_LOOP ( 'NONE', ( #15444, #39629 ) ) ;
#29453 = DIRECTION ( 'NONE',  ( -0.000000000000000000, -0.000000000000000000, -1.000000000000000000 ) ) ;
#29454 = CARTESIAN_POINT ( 'NONE',  ( -32.34874870218063592, -26.64985754041175525, 6.700000000000000178 ) ) ;
#29455 =( BOUNDED_CURVE ( )  B_SPLINE_CURVE ( 3, ( #31267, #12920, #25486, #40299 ),
 .UNSPECIFIED., .F., .T. ) 
 B_SPLINE_CURVE_WITH_KNOTS ( ( 4, 4 ),
 ( 4.712388980384689674, 5.617490880575807033 ),
 .UNSPECIFIED. ) 
 CURVE ( )  GEOMETRIC_REPRESENTATION_ITEM ( )  RATIONAL_B_SPLINE_CURVE ( ( 1.000000000000000000, 0.9328897322841716022, 0.9328897322841716022, 1.000000000000000000 ) ) 
 REPRESENTATION_ITEM ( '' )  );
#29456 = CARTESIAN_POINT ( 'NONE',  ( -57.29470892912325297, 33.22074752690817689, -3.999999999999999112 ) ) ;
#29457 = CARTESIAN_POINT ( 'NONE',  ( 3.892870342314429521, -32.29814067960646895, 6.867280401193707640 ) ) ;
#29458 = ORIENTED_EDGE ( 'NONE', *, *, #30973, .T. ) ;
#29459 = CARTESIAN_POINT ( 'NONE',  ( 22.30551760662672223, 4.735879390933545707, 3.387776000085759964 ) ) ;
#29460 = CARTESIAN_POINT ( 'NONE',  ( 80.25084519670726024, 66.24728552308208407, -1.725837398063457373 ) ) ;
#29461 = EDGE_CURVE ( 'NONE', #5814, #26604, #15852, .T. ) ;
#29462 = AXIS2_PLACEMENT_3D ( 'NONE', #37810, #15803, #31661 ) ;
#29463 = CARTESIAN_POINT ( 'NONE',  ( 14.72123706662768505, -4.461995682952463405, -2.504003097347854645 ) ) ;
#29464 = VERTEX_POINT ( 'NONE', #16064 ) ;
#29466 = DIRECTION ( 'NONE',  ( 1.000000000000000000, -0.000000000000000000, 0.000000000000000000 ) ) ;
#29465 = CARTESIAN_POINT ( 'NONE',  ( -1.597074440709042475, -28.39657532162993192, 7.651421919295147589 ) ) ;
#29467 = CARTESIAN_POINT ( 'NONE',  ( -70.31379738671766688, 0.01634305466338900267, 5.969163363928942090 ) ) ;
#29468 = CARTESIAN_POINT ( 'NONE',  ( 76.89779646338298846, 61.47851784853087054, 3.801074476324135087 ) ) ;
#29469 = VECTOR ( 'NONE', #25667, 1000.000000000000227 ) ;
#29470 = CARTESIAN_POINT ( 'NONE',  ( 24.20640518876499669, 2.566492102625094418, -4.042989007339715890 ) ) ;
#29471 = FACE_OUTER_BOUND ( 'NONE', #34400, .T. ) ;
#29472 = DIRECTION ( 'NONE',  ( 0.000000000000000000, 0.000000000000000000, 1.000000000000000000 ) ) ;
#29473 = PLANE ( 'NONE',  #17698 ) ;
#29474 = DIRECTION ( 'NONE',  ( -0.000000000000000000, -0.000000000000000000, -1.000000000000000000 ) ) ;
#29475 = CARTESIAN_POINT ( 'NONE',  ( 81.93064166251132008, 62.10341262211382229, 1.859759604986720438 ) ) ;
#29476 = CARTESIAN_POINT ( 'NONE',  ( -0.9582821081414136799, -31.84621386888283823, 7.678495282201405203 ) ) ;
#29477 = CARTESIAN_POINT ( 'NONE',  ( 32.63594197759655913, -2.548278591510585667, -5.894033951951210604 ) ) ;
#29478 = EDGE_CURVE ( 'NONE', #2897, #37746, #39906, .T. ) ;
#29479 = EDGE_CURVE ( 'NONE', #10139, #32700, #30778, .T. ) ;
#29480 = CARTESIAN_POINT ( 'NONE',  ( 2.360030607804072922, -26.23451782836966473, 7.784476445165072533 ) ) ;
#29481 = CARTESIAN_POINT ( 'NONE',  ( 22.82081674902891066, -6.972797972010963186, 0.5552882429563011923 ) ) ;
#29482 = EDGE_CURVE ( 'NONE', #13676, #38902, #20904, .T. ) ;
#29483 = DIRECTION ( 'NONE',  ( 0.6427876096865481337, -0.7660444431189706860, -0.000000000000000000 ) ) ;
#29484 = ORIENTED_EDGE ( 'NONE', *, *, #27148, .F. ) ;
#29485 = CARTESIAN_POINT ( 'NONE',  ( 0.7160520742141273098, -26.31553137280090127, 6.895222827070022653 ) ) ;
#29486 = CARTESIAN_POINT ( 'NONE',  ( -1.360749241107399587, -27.85905441312543473, 7.255881584735163869 ) ) ;
#29487 = CARTESIAN_POINT ( 'NONE',  ( 36.94812879981065379, -2.593733626342286769, -5.973047111718997826 ) ) ;
#29488 = CARTESIAN_POINT ( 'NONE',  ( 0.9969205846672903881, -32.89635929740111919, 7.761597726988852308 ) ) ;
#29489 = B_SPLINE_CURVE_WITH_KNOTS ( 'NONE', 3,
 ( #19829, #7871, #4197, #4403, #35893, #1315, #38754, #16924, #16715, #33000, #4784, #16525, #29505, #29101, #29305, #7670, #13242, #1118, #26420, #17515, #20616, #11746, #15626, #25103, #11146, #17933, #30111, #1920, #17318, #14242, #39770 ),
 .UNSPECIFIED., .F., .F.,
 ( 4, 3, 3, 3, 3, 3, 3, 3, 3, 3, 4 ),
 ( 1.084202172485504434E-19, 2.999644130997740433E-05, 6.002588995694861873E-05, 8.960886084588098833E-05, 0.0001190604700446487542, 0.0001489538463052730486, 0.0001796139255493964726, 0.0002109707048517068617, 0.0002426195318110357631, 0.0002740640997890045577, 0.0002849778069099846906 ),
 .UNSPECIFIED. ) ;
#29490 = CARTESIAN_POINT ( 'NONE',  ( 4.460814650971867579, -27.41817363093848314, 7.750000000000000888 ) ) ;
#29491 = AXIS2_PLACEMENT_3D ( 'NONE', #23826, #20537, #8174 ) ;
#29492 = CARTESIAN_POINT ( 'NONE',  ( -1.799453152388704957, -29.60305503924953996, 7.717693117505774580 ) ) ;
#29493 = CARTESIAN_POINT ( 'NONE',  ( 2.237702017751752592, -32.92720639772907987, 6.889465824494256374 ) ) ;
#29494 = DIRECTION ( 'NONE',  ( 1.000000000000000000, 0.000000000000000000, 0.000000000000000000 ) ) ;
#29495 = ORIENTED_EDGE ( 'NONE', *, *, #24174, .T. ) ;
#29496 = CARTESIAN_POINT ( 'NONE',  ( 36.18524227031805651, -3.553218394490209597, 5.771100729284209585 ) ) ;
#29497 = CARTESIAN_POINT ( 'NONE',  ( -69.92837670882107659, -0.7829914368874777431, 3.916079783099610800 ) ) ;
#29498 = CARTESIAN_POINT ( 'NONE',  ( 67.20767295658653495, 57.90495500903578829, -3.994504660676310603 ) ) ;
#29499 = AXIS2_PLACEMENT_3D ( 'NONE', #20866, #39595, #8909 ) ;
#29500 = CARTESIAN_POINT ( 'NONE',  ( -0.9128197825508301833, -27.39481314169073300, 7.635761828346577573 ) ) ;
#29501 = ORIENTED_EDGE ( 'NONE', *, *, #3054, .T. ) ;
#29502 = DIRECTION ( 'NONE',  ( -0.6605219282605402364, 0.000000000000000000, 0.7508067542896625923 ) ) ;
#29503 = CARTESIAN_POINT ( 'NONE',  ( 30.87059228904019648, -3.396537768743968844, 4.950897058115855565 ) ) ;
#29504 = DIRECTION ( 'NONE',  ( -0.9848077530122092416, 0.1736481776669241694, -0.000000000000000000 ) ) ;
#29505 = CARTESIAN_POINT ( 'NONE',  ( 0.9200650878653321429, -32.87917373532453524, 6.903372536218457256 ) ) ;
#29506 = LINE ( 'NONE', #20618, #37853 ) ;
#29507 = CARTESIAN_POINT ( 'NONE',  ( -58.92473026143653669, 13.37661300689600274, -2.500000000000000000 ) ) ;
#29508 = ORIENTED_EDGE ( 'NONE', *, *, #4806, .F. ) ;
#29509 = CARTESIAN_POINT ( 'NONE',  ( 21.71254722604186327, 6.323917084280038736, 3.194779952286587399 ) ) ;
#29510 = EDGE_CURVE ( 'NONE', #39459, #1323, #7436, .T. ) ;
#29511 = CARTESIAN_POINT ( 'NONE',  ( 81.02539575022784391, 62.78269734341446195, 3.300462285847920008 ) ) ;
#29512 = AXIS2_PLACEMENT_3D ( 'NONE', #2982, #12614, #6245 ) ;
#29513 = CARTESIAN_POINT ( 'NONE',  ( -63.63873222603260160, 44.01641787740143030, 2.404113166277060731 ) ) ;
#29514 = VERTEX_POINT ( 'NONE', #26548 ) ;
#29515 = CARTESIAN_POINT ( 'NONE',  ( 80.27394690667868815, 60.98324426164374046, -1.908681007153611553 ) ) ;
#29517 = CARTESIAN_POINT ( 'NONE',  ( -8.248748702180632719, -26.64985754041175525, 6.700000000000000178 ) ) ;
#29516 = CARTESIAN_POINT ( 'NONE',  ( 26.73338393872905527, 0.9282423383602553812, 4.382137618851254857 ) ) ;
#29518 = CARTESIAN_POINT ( 'NONE',  ( 81.21919753141084186, 63.96565923610828008, -3.341858160548294876 ) ) ;
#29519 = CARTESIAN_POINT ( 'NONE',  ( 79.36252896413687097, 63.71833510339342155, 3.756013696796373758 ) ) ;
#29520 = ADVANCED_FACE ( 'NONE', ( #23840 ), #5126, .F. ) ;
#29521 = LINE ( 'NONE', #10373, #14201 ) ;
#29522 = EDGE_CURVE ( 'NONE', #24427, #5530, #11007, .T. ) ;
#29523 = CARTESIAN_POINT ( 'NONE',  ( 82.58199242721491373, 63.55547749749371178, 1.287552078897677976 ) ) ;
#29524 = CARTESIAN_POINT ( 'NONE',  ( -63.55813210593559859, 43.57418346405783183, 2.980081600457315183 ) ) ;
#29525 = CARTESIAN_POINT ( 'NONE',  ( 26.57131730419879290, 2.962615056577905026, -1.092182624680714254 ) ) ;
#29526 = CARTESIAN_POINT ( 'NONE',  ( -62.74303057475820111, 35.98358351542150046, -5.167368988332354363 ) ) ;
#29527 = ORIENTED_EDGE ( 'NONE', *, *, #28469, .T. ) ;
#29528 = CARTESIAN_POINT ( 'NONE',  ( -79.67547651979579371, -5.606679663933569202, 4.861676929742372089 ) ) ;
#29529 = CARTESIAN_POINT ( 'NONE',  ( 23.06098311254805466, 0.3526106142807417521, -5.951280228554626461 ) ) ;
#29530 = ADVANCED_FACE ( 'NONE', ( #23263 ), #1643, .T. ) ;
#29531 = LINE ( 'NONE', #13878, #22198 ) ;
#29532 = FACE_OUTER_BOUND ( 'NONE', #23327, .T. ) ;
#29533 = ORIENTED_EDGE ( 'NONE', *, *, #23741, .T. ) ;
#29534 = CARTESIAN_POINT ( 'NONE',  ( 37.17621594122605444, -2.565172031526568919, -5.981066268316136636 ) ) ;
#29535 = DIRECTION ( 'NONE',  ( 0.9848077530122103518, -0.1736481776669172583, -0.000000000000000000 ) ) ;
#29536 = FACE_OUTER_BOUND ( 'NONE', #26212, .T. ) ;
#29537 = CARTESIAN_POINT ( 'NONE',  ( -1.027820402979995995, -31.76241043247472717, 6.867280401193706751 ) ) ;
#29538 = CARTESIAN_POINT ( 'NONE',  ( 5.121324086407808451, -26.64985754041175525, 6.700000000000000178 ) ) ;
#29539 = CARTESIAN_POINT ( 'NONE',  ( 5.077466957584408469, -30.51492847852392742, 7.501983001166816933 ) ) ;
#29540 = CARTESIAN_POINT ( 'NONE',  ( 1.886314362785468601, -26.07487193409462378, 6.921725064902949143 ) ) ;
#29541 = CARTESIAN_POINT ( 'NONE',  ( 25.62812034757272173, 2.162893437960721865, -4.131162739758373448 ) ) ;
#29542 = ORIENTED_EDGE ( 'NONE', *, *, #34503, .F. ) ;
#29543 = CARTESIAN_POINT ( 'NONE',  ( 66.86920591220189181, 57.92326096844472261, 3.999524142429984330 ) ) ;
#29544 = CARTESIAN_POINT ( 'NONE',  ( 73.12040677118544352, 60.72248633788713335, -3.934110468535476191 ) ) ;
#29545 = CARTESIAN_POINT ( 'NONE',  ( 84.33668400229728945, 2.728897857615574019, 2.746074863882507877 ) ) ;
#29546 = B_SPLINE_CURVE_WITH_KNOTS ( 'NONE', 3,
 ( #15540, #25019, #40239, #317 ),
 .UNSPECIFIED., .F., .F.,
 ( 4, 4 ),
 ( 0.000000000000000000, 6.391136169899991049E-06 ),
 .UNSPECIFIED. ) ;
#29547 = ORIENTED_EDGE ( 'NONE', *, *, #2406, .T. ) ;
#29548 = CARTESIAN_POINT ( 'NONE',  ( 26.60736997101286505, 1.631599532540721542, 4.332120141861649287 ) ) ;
#29549 = PRODUCT_CONTEXT ( 'NONE', #26585, 'mechanical' ) ;
#29550 = CARTESIAN_POINT ( 'NONE',  ( -22.34874870218063947, -26.64985754041175525, 6.700000000000000178 ) ) ;
#29551 = CARTESIAN_POINT ( 'NONE',  ( 1.129730468697653256, -26.12992822677308169, 7.783750581861600182 ) ) ;
#29552 = CARTESIAN_POINT ( 'NONE',  ( 5.067738213087761068, -29.09985929542945371, 7.754798119455333705 ) ) ;
#29553 = ORIENTED_EDGE ( 'NONE', *, *, #24649, .F. ) ;
#29554 = CARTESIAN_POINT ( 'NONE',  ( 80.91431153141793686, 61.21107275232141376, -1.487544896896259239 ) ) ;
#29555 = CARTESIAN_POINT ( 'NONE',  ( 5.166671796352685142, -29.08527243180875743, 7.751599049952198506 ) ) ;
#29556 = CARTESIAN_POINT ( 'NONE',  ( 78.85101321104561123, 65.59805058642720610, 2.603857329607151883 ) ) ;
#29557 = CARTESIAN_POINT ( 'NONE',  ( 1.587289166052635148, -33.88748355710808369, 6.894806418505347700 ) ) ;
#29558 = CARTESIAN_POINT ( 'NONE',  ( -16.87867591359218977, -26.64985754041175525, 6.700000000000000178 ) ) ;
#29559 = AXIS2_PLACEMENT_3D ( 'NONE', #12136, #9878, #16050 ) ;
#29560 = CARTESIAN_POINT ( 'NONE',  ( 18.96853221647454646, 7.708738308554112351, -3.077308032275870797 ) ) ;
#29561 = CARTESIAN_POINT ( 'NONE',  ( -1.796843176524750341, -29.45368158032236749, 7.761113333117551250 ) ) ;
#29562 = FACE_OUTER_BOUND ( 'NONE', #39912, .T. ) ;
#29563 = CARTESIAN_POINT ( 'NONE',  ( 23.14181338739152238, 4.049881389590580305, -3.073623331090673538 ) ) ;
#29564 = ORIENTED_EDGE ( 'NONE', *, *, #13822, .F. ) ;
#29565 = LINE ( 'NONE', #39220, #27490 ) ;
#29566 = EDGE_CURVE ( 'NONE', #40275, #16672, #37984, .T. ) ;
#29567 = ORIENTED_EDGE ( 'NONE', *, *, #7328, .F. ) ;
#29568 = ADVANCED_FACE ( 'NONE', ( #26751 ), #35830, .F. ) ;
#29569 = CARTESIAN_POINT ( 'NONE',  ( 14.61802081865032932, -4.461849342347350422, 2.499999999999997780 ) ) ;
#29570 = EDGE_CURVE ( 'NONE', #1634, #22687, #33424, .T. ) ;
#29571 = CARTESIAN_POINT ( 'NONE',  ( -74.03934154708541371, -3.833512911058256645, -9.504820148027839366 ) ) ;
#29572 = CARTESIAN_POINT ( 'NONE',  ( -0.03062609074085211741, -26.64357016194428951, 7.692469944509195301 ) ) ;
#29573 = CYLINDRICAL_SURFACE ( 'NONE', #10268, 0.09010775117053060335 ) ;
#29574 = CARTESIAN_POINT ( 'NONE',  ( 81.05462132553121535, 63.14435662960352147, 3.368075118064897566 ) ) ;
#29575 = CARTESIAN_POINT ( 'NONE',  ( -1.508037414099143714, -30.69513570029197425, 7.784838882742139532 ) ) ;
#29576 = CARTESIAN_POINT ( 'NONE',  ( -2.759813073242583847, -26.83731626112308533, 7.013842709614101167 ) ) ;
#29577 = CARTESIAN_POINT ( 'NONE',  ( -0.8809668920273273640, -31.78275555260969654, 7.691066658568952441 ) ) ;
#29578 = FACE_OUTER_BOUND ( 'NONE', #40420, .T. ) ;
#29579 = AXIS2_PLACEMENT_3D ( 'NONE', #20941, #29802, #14542 ) ;
#29580 = CARTESIAN_POINT ( 'NONE',  ( -64.78468263673624961, 34.77444586572286767, 6.350676759654645842 ) ) ;
#29581 = CARTESIAN_POINT ( 'NONE',  ( -17.27251170661583402, -8.656638842136340273, -6.000000000000000000 ) ) ;
#29582 = CARTESIAN_POINT ( 'NONE',  ( -10.87867591359219155, -24.55319635012989110, 6.700000000000000178 ) ) ;
#29583 = CARTESIAN_POINT ( 'NONE',  ( -4.248748702180636272, -25.49307895267003587, 6.700000000000000178 ) ) ;
#29584 = CARTESIAN_POINT ( 'NONE',  ( 68.99357861020946814, 59.34113723602050783, 3.933428174212677320 ) ) ;
#29585 = CARTESIAN_POINT ( 'NONE',  ( 29.10122315827134898, 0.3582907782008117326, 4.748347708226712705 ) ) ;
#29586 = ORIENTED_EDGE ( 'NONE', *, *, #9436, .F. ) ;
#29587 = CARTESIAN_POINT ( 'NONE',  ( -64.08758708074094557, 43.59023632408901960, -1.301703141159380017 ) ) ;
#29588 = CARTESIAN_POINT ( 'NONE',  ( 85.02879235234962607, 2.798117532367836446, 2.624272742801059710 ) ) ;
#29589 = AXIS2_PLACEMENT_3D ( 'NONE', #34524, #13079, #135 ) ;
#29591 = CARTESIAN_POINT ( 'NONE',  ( -0.3990770562238331598, -26.76953060260428430, 6.941203072598471024 ) ) ;
#29590 = CARTESIAN_POINT ( 'NONE',  ( 79.25894186866878499, 65.67357942822117423, -2.700485128497464249 ) ) ;
#29592 = CARTESIAN_POINT ( 'NONE',  ( -1.376785424038392325, -31.22775445417016371, 7.771081512783700518 ) ) ;
#29593 = CARTESIAN_POINT ( 'NONE',  ( -1.241488500120730754, -27.67378822227167134, 7.011627023500182077 ) ) ;
#29594 = CARTESIAN_POINT ( 'NONE',  ( 4.944078209288079506, -30.88464969939810345, 7.750000000000000888 ) ) ;
#29595 = ORIENTED_EDGE ( 'NONE', *, *, #8404, .F. ) ;
#29596 = CARTESIAN_POINT ( 'NONE',  ( 4.993907954365692348, -30.75430347691218813, 7.635761828346578461 ) ) ;
#29597 = DIRECTION ( 'NONE',  ( 1.000000000000000000, -0.000000000000000000, 0.000000000000000000 ) ) ;
#29598 = ORIENTED_EDGE ( 'NONE', *, *, #21243, .F. ) ;
#29599 = CARTESIAN_POINT ( 'NONE',  ( -71.87291851043532631, -21.11138264414386612, 5.937231121521803878 ) ) ;
#29600 = CARTESIAN_POINT ( 'NONE',  ( 81.02780191652712460, 61.56951766280579363, -2.259810845157016246 ) ) ;
#29601 = CARTESIAN_POINT ( 'NONE',  ( 24.90975462926189010, 3.541767663397652033, 0.6518453417789448201 ) ) ;
#29602 = CARTESIAN_POINT ( 'NONE',  ( 78.68112288793685138, 66.00442204571392324, 1.607835478472332547 ) ) ;
#29603 = CARTESIAN_POINT ( 'NONE',  ( 23.61787448442827753, 0.7654929067543206900, 5.373130871398858588 ) ) ;
#29604 = ORIENTED_EDGE ( 'NONE', *, *, #40064, .T. ) ;
#29605 = CARTESIAN_POINT ( 'NONE',  ( 4.934953675687837382, -28.52226686387824373, 7.754798119455333705 ) ) ;
#29607 = CARTESIAN_POINT ( 'NONE',  ( -64.08758708074093136, 38.76906266698303227, -3.999999999999999556 ) ) ;
#29606 = CARTESIAN_POINT ( 'NONE',  ( 14.69558838330753936, -3.003688195628454238, 6.000000000000001776 ) ) ;
#29608 = CARTESIAN_POINT ( 'NONE',  ( -1.261910041069868260, -27.90116479715461750, 7.695279973900954751 ) ) ;
#29609 = DIRECTION ( 'NONE',  ( -0.000000000000000000, -0.000000000000000000, -1.000000000000000000 ) ) ;
#29610 = CARTESIAN_POINT ( 'NONE',  ( 22.91810752083389602, 4.152906525941994609, -3.257904903544968978 ) ) ;
#29611 = ORIENTED_EDGE ( 'NONE', *, *, #6814, .F. ) ;
#29612 = CARTESIAN_POINT ( 'NONE',  ( -71.90221254882203539, -0.5206366332505392158, 5.920661432671355584 ) ) ;
#29613 = ORIENTED_EDGE ( 'NONE', *, *, #20485, .T. ) ;
#29614 = EDGE_CURVE ( 'NONE', #28877, #7270, #13882, .T. ) ;
#29615 = CARTESIAN_POINT ( 'NONE',  ( 22.32365817596653557, 5.835156701882857178, 3.488260158266504263 ) ) ;
#29616 = VECTOR ( 'NONE', #36873, 1000.000000000000000 ) ;
#29618 = ADVANCED_FACE ( 'NONE', ( #24462 ), #21595, .F. ) ;
#29617 = CARTESIAN_POINT ( 'NONE',  ( 21.85643539959776760, 3.765123657700408355, 3.918568846604040257 ) ) ;
#29619 = CARTESIAN_POINT ( 'NONE',  ( -44.23414840393349579, -23.60493063168010153, 6.000000000000000000 ) ) ;
#29620 = ORIENTED_EDGE ( 'NONE', *, *, #39239, .F. ) ;
#29621 = CARTESIAN_POINT ( 'NONE',  ( 0.4895345795279826828, -32.74700981117575793, 6.892063359921932530 ) ) ;
#29622 = CARTESIAN_POINT ( 'NONE',  ( 79.20630559137210014, 66.06758606029012526, 1.969816429103250055 ) ) ;
#29623 = CARTESIAN_POINT ( 'NONE',  ( 85.16823716249373888, 2.433965874742513247, 4.055466505201608562 ) ) ;
#29624 = DIRECTION ( 'NONE',  ( -1.000000000000000000, 0.000000000000000000, 0.000000000000000000 ) ) ;
#29625 = ORIENTED_EDGE ( 'NONE', *, *, #4448, .F. ) ;
#29626 = CARTESIAN_POINT ( 'NONE',  ( -80.66010496297788279, -5.648439302891065772, 5.209062318100336597 ) ) ;
#29627 = DIRECTION ( 'NONE',  ( 0.000000000000000000, 0.000000000000000000, 1.000000000000000000 ) ) ;
#29628 = DIRECTION ( 'NONE',  ( -0.000000000000000000, -1.000000000000000000, -0.000000000000000000 ) ) ;
#29629 = CARTESIAN_POINT ( 'NONE',  ( 21.50482873268578743, -2.719662516908865069, -3.562746638620634343 ) ) ;
#29630 = CARTESIAN_POINT ( 'NONE',  ( 32.77912487546454656, -0.9333593928079626512, -5.322373221583833747 ) ) ;
#29631 = DIRECTION ( 'NONE',  ( -1.000000000000000000, -1.165409145176969993E-16, 0.000000000000000000 ) ) ;
#29632 = CYLINDRICAL_SURFACE ( 'NONE', #32540, 0.09010775117052602368 ) ;
#29633 = DIRECTION ( 'NONE',  ( -0.000000000000000000, -0.000000000000000000, -1.000000000000000000 ) ) ;
#29634 = VERTEX_POINT ( 'NONE', #20974 ) ;
#29635 = DIRECTION ( 'NONE',  ( -0.000000000000000000, -0.000000000000000000, 1.000000000000000000 ) ) ;
#29636 = CIRCLE ( 'NONE', #14487, 0.1000000000000028644 ) ;
#29637 = CARTESIAN_POINT ( 'NONE',  ( -18.48280404870591553, -63.98126818465317456, 2.500000000000000000 ) ) ;
#29638 = CARTESIAN_POINT ( 'NONE',  ( 4.987105146749665430, -28.38306410523611945, 7.773839561854631874 ) ) ;
#29639 = ORIENTED_EDGE ( 'NONE', *, *, #15939, .T. ) ;
#29640 = ORIENTED_EDGE ( 'NONE', *, *, #21939, .T. ) ;
#29641 = CARTESIAN_POINT ( 'NONE',  ( 34.79231454646104993, -3.833543758068950869, 5.378533583580677124 ) ) ;
#29642 = CARTESIAN_POINT ( 'NONE',  ( -1.606999173425283756, -30.71499622462987489, 6.875671892026064214 ) ) ;
#29643 = EDGE_CURVE ( 'NONE', #7364, #16945, #36990, .T. ) ;
#29644 = CARTESIAN_POINT ( 'NONE',  ( 33.43971231075012440, -3.588053834546123255, 5.336497937005737491 ) ) ;
#29645 = CARTESIAN_POINT ( 'NONE',  ( 86.83589974223885122, -1.124279187257583912, 5.239974236049660838 ) ) ;
#29646 = VERTEX_POINT ( 'NONE', #39907 ) ;
#29647 = CIRCLE ( 'NONE', #28331, 0.1000000000000028644 ) ;
#29648 = CARTESIAN_POINT ( 'NONE',  ( 4.913358501582978377, -28.45779633779761397, 6.889465824494254598 ) ) ;
#29649 = ORIENTED_EDGE ( 'NONE', *, *, #14086, .T. ) ;
#29650 = CARTESIAN_POINT ( 'NONE',  ( -56.58158928110403707, 30.30283765713063815, -3.953813256333429837 ) ) ;
#29652 = DIRECTION ( 'NONE',  ( 1.000000000000000000, 9.912705577010326536E-16, 0.000000000000000000 ) ) ;
#29651 = CARTESIAN_POINT ( 'NONE',  ( -60.15914593959029588, -52.45670913645259503, -2.307692307692302158 ) ) ;
#29653 = ORIENTED_EDGE ( 'NONE', *, *, #20123, .F. ) ;
#29654 = CARTESIAN_POINT ( 'NONE',  ( 22.97383871700119684, 3.759880532170991607, 3.599142388413823390 ) ) ;
#29655 = CARTESIAN_POINT ( 'NONE',  ( 82.33210628740326342, 64.54215504103264323, -1.775718711110015224 ) ) ;
#29656 = CARTESIAN_POINT ( 'NONE',  ( 3.300479879060630228, -34.00561972003898603, 7.635761828346577573 ) ) ;
#29657 = EDGE_LOOP ( 'NONE', ( #5131, #7383, #31939, #12372, #6792 ) ) ;
#29658 = DIRECTION ( 'NONE',  ( -0.000000000000000000, 1.000000000000000000, -0.000000000000000000 ) ) ;
#29659 = CARTESIAN_POINT ( 'NONE',  ( -51.21549048184568420, -38.28842912540938670, 6.000000000000000000 ) ) ;
#29660 = CARTESIAN_POINT ( 'NONE',  ( 74.65712387123647886, 61.84722771748617731, 3.833662259905226133 ) ) ;
#29661 = CARTESIAN_POINT ( 'NONE',  ( 22.26111053501417913, 2.653359810932870211, -4.982668050499428958 ) ) ;
#29662 = CARTESIAN_POINT ( 'NONE',  ( -89.00859394718983708, 2.429809908903242555, 12.50000000000000000 ) ) ;
#29663 = CARTESIAN_POINT ( 'NONE',  ( -56.59682361629209879, 30.63869417066593925, -3.015094993620159425 ) ) ;
#29665 = EDGE_CURVE ( 'NONE', #14626, #37912, #27553, .T. ) ;
#29664 = CARTESIAN_POINT ( 'NONE',  ( 26.91150311004617990, 1.351951412127374130, -4.406588936121679900 ) ) ;
#29666 = CARTESIAN_POINT ( 'NONE',  ( -62.76709047716261125, 35.75517504125645729, 5.477639365100117175 ) ) ;
#29667 = CARTESIAN_POINT ( 'NONE',  ( -59.87552183813137674, 24.84364830758654108, -9.800414904976365804 ) ) ;
#29668 = CARTESIAN_POINT ( 'NONE',  ( 78.91303721271685845, 66.16570306020605585, 1.285939662725142485 ) ) ;
#29669 = CARTESIAN_POINT ( 'NONE',  ( 88.32659454254844889, -0.8548986265586405731, 1.105665148257566566 ) ) ;
#29670 = CARTESIAN_POINT ( 'NONE',  ( 33.51852797086635150, -3.949141208872448683, 4.993608438669980387 ) ) ;
#29671 = CARTESIAN_POINT ( 'NONE',  ( 2.350156857115043074, -26.23259544552930933, 7.785172627573962778 ) ) ;
#29672 = CARTESIAN_POINT ( 'NONE',  ( -72.41861705067529442, -46.92014984782673537, 9.888354608821900982 ) ) ;
#29673 = DIRECTION ( 'NONE',  ( 0.3420201433256748746, -0.9396926207859060964, 0.000000000000000000 ) ) ;
#29674 = ORIENTED_EDGE ( 'NONE', *, *, #38567, .F. ) ;
#29675 = CARTESIAN_POINT ( 'NONE',  ( 8.290806648384990041, -35.94265729135299381, 6.000000000000000000 ) ) ;
#29676 = CARTESIAN_POINT ( 'NONE',  ( 0.03282529437175818465, -26.49270213989298384, 6.863805608295728611 ) ) ;
#29677 = AXIS2_PLACEMENT_3D ( 'NONE', #23286, #17085, #38717 ) ;
#29678 = CARTESIAN_POINT ( 'NONE',  ( 36.80679559313785632, -3.101469264525490654, -5.950988646661206083 ) ) ;
#29679 = DIRECTION ( 'NONE',  ( 1.000000000000000000, 0.000000000000000000, 0.000000000000000000 ) ) ;
#29680 = CARTESIAN_POINT ( 'NONE',  ( 4.976860739914288345, -28.33918239773801417, 7.698786668945014178 ) ) ;
#29681 = CARTESIAN_POINT ( 'NONE',  ( -63.38664175810290402, 42.64173782962942028, -3.644997060774788800 ) ) ;
#29682 = CARTESIAN_POINT ( 'NONE',  ( -63.08758708074093136, 38.76906266698301806, -4.000000000000000000 ) ) ;
#29683 = DIRECTION ( 'NONE',  ( -0.6502177225477896449, 0.3754033771448298529, -0.6605219282605402364 ) ) ;
#29684 = VERTEX_POINT ( 'NONE', #27143 ) ;
#29685 = CARTESIAN_POINT ( 'NONE',  ( 35.97282836976979326, -1.842333002647675633, 5.810885693563370147 ) ) ;
#29686 =( BOUNDED_CURVE ( )  B_SPLINE_CURVE ( 3, ( #27045, #5019, #36920, #8699 ),
 .UNSPECIFIED., .F., .T. ) 
 B_SPLINE_CURVE_WITH_KNOTS ( ( 4, 4 ),
 ( 4.886921905584129533, 4.941946782021394924 ),
 .UNSPECIFIED. ) 
 CURVE ( )  GEOMETRIC_REPRESENTATION_ITEM ( )  RATIONAL_B_SPLINE_CURVE ( ( 1.000000000000000000, 0.9997477044959499626, 0.9997477044959499626, 1.000000000000000000 ) ) 
 REPRESENTATION_ITEM ( '' )  );
#29687 = CYLINDRICAL_SURFACE ( 'NONE', #10016, 0.09010775117052950700 ) ;
#29688 = CARTESIAN_POINT ( 'NONE',  ( 67.10107710889761279, 58.19782780592215943, -3.994504660676309271 ) ) ;
#29689 = DIRECTION ( 'NONE',  ( 1.047444401652940007E-14, -1.000000000000000000, -0.000000000000000000 ) ) ;
#29690 = ORIENTED_EDGE ( 'NONE', *, *, #16673, .T. ) ;
#29691 = DIRECTION ( 'NONE',  ( -0.9995570907297058882, -0.02975940812527359119, -0.000000000000000000 ) ) ;
#29692 = CARTESIAN_POINT ( 'NONE',  ( 3.910420815644036097, -32.15368021116306352, 7.721096864323906850 ) ) ;
#29693 = CARTESIAN_POINT ( 'NONE',  ( -59.87552183813137674, 24.84364830758654108, 9.800414904976365804 ) ) ;
#29694 = CARTESIAN_POINT ( 'NONE',  ( 0.4851296283628217521, -26.28768369622591194, 7.643192810543818716 ) ) ;
#29695 = ADVANCED_FACE ( 'NONE', ( #2471 ), #12095, .F. ) ;
#29696 = CARTESIAN_POINT ( 'NONE',  ( 0.6783104270758654186, -48.60743831809499227, 6.000000000000000000 ) ) ;
#29697 = CARTESIAN_POINT ( 'NONE',  ( -1.699306555046655731, -29.52380873363099312, 7.785387725071483800 ) ) ;
#29698 = ORIENTED_EDGE ( 'NONE', *, *, #35409, .F. ) ;
#29699 = EDGE_CURVE ( 'NONE', #6547, #14780, #3134, .T. ) ;
#29700 = CARTESIAN_POINT ( 'NONE',  ( 23.14061585149417510, 4.042732116653498409, 3.088342274992314618 ) ) ;
#29701 = CARTESIAN_POINT ( 'NONE',  ( 4.944078209288079506, -30.88464969939810345, 7.750000000000000888 ) ) ;
#29702 = CARTESIAN_POINT ( 'NONE',  ( 17.93706920410982875, -3.171549663534191321, 2.963851838818105211 ) ) ;
#29703 = CARTESIAN_POINT ( 'NONE',  ( 81.21856020378538688, 61.45841878490982424, 1.842213953838256257 ) ) ;
#29704 = AXIS2_PLACEMENT_3D ( 'NONE', #22444, #28610, #27986 ) ;
#29705 = CARTESIAN_POINT ( 'NONE',  ( 5.618319323718388603, -33.03553571191711313, 7.013842709614101167 ) ) ;
#29706 = ORIENTED_EDGE ( 'NONE', *, *, #8071, .T. ) ;
#29707 = CARTESIAN_POINT ( 'NONE',  ( 79.14505932034367675, 62.66850290118683375, -3.750642650174860204 ) ) ;
#29708 = B_SPLINE_CURVE_WITH_KNOTS ( 'NONE', 3,
 ( #30986, #40026, #30785, #14902, #17570, #30153, #36533, #1973, #20885, #24178, #18398, #5039, #24379, #33473, #5240, #11192, #20670, #33669, #14492, #27670, #34087, #36938, #2792, #36735, #18193, #23763, #36333, #8517, #5447, #27259, #24586 ),
 .UNSPECIFIED., .F., .F.,
 ( 4, 3, 3, 3, 3, 3, 3, 3, 3, 3, 4 ),
 ( 0.000000000000000000, 2.999644130997572382E-05, 6.002588995694619961E-05, 8.960886084587850822E-05, 0.0001190604700446468297, 0.0001489538463052692810, 0.0001796139255493974483, 0.0002109707048517052354, 0.0002426195318110341910, 0.0002740640997890042866, 0.0002849778069099884853 ),
 .UNSPECIFIED. ) ;
#29710 = CARTESIAN_POINT ( 'NONE',  ( 14.77222812468959035, -4.461995682952466957, -2.511961485181824383 ) ) ;
#29709 = CARTESIAN_POINT ( 'NONE',  ( 21.73424372594157816, 0.2275660760974567987, 9.075264012513089895 ) ) ;
#29711 = CARTESIAN_POINT ( 'NONE',  ( 80.50924551448741795, 65.11801186547818077, -3.171364025122248353 ) ) ;
#29712 = CARTESIAN_POINT ( 'NONE',  ( 77.45101235711661047, 65.18271368322074011, 2.178915381671227891 ) ) ;
#29713 = CARTESIAN_POINT ( 'NONE',  ( -0.8649431887485288240, -27.33854829040479473, 7.785172627573962778 ) ) ;
#29714 = EDGE_CURVE ( 'NONE', #26905, #28895, #16928, .T. ) ;
#29715 = CARTESIAN_POINT ( 'NONE',  ( 81.47320529907104003, 61.46857867680783016, 1.048259027381037489 ) ) ;
#29716 = CARTESIAN_POINT ( 'NONE',  ( 91.69672933337632514, -4.640393979863029372, 6.000000000000001776 ) ) ;
#29717 = CARTESIAN_POINT ( 'NONE',  ( 27.13744335700502219, 0.8961374054434056990, -5.485310518450965844 ) ) ;
#29718 = CARTESIAN_POINT ( 'NONE',  ( -64.25913952751385239, 36.58001704789106867, -5.467911005455038165 ) ) ;
#29719 = ORIENTED_EDGE ( 'NONE', *, *, #21310, .F. ) ;
#29720 = CARTESIAN_POINT ( 'NONE',  ( -79.44656165559027272, -5.517286240398389552, 7.192311668639653988 ) ) ;
#29721 = CARTESIAN_POINT ( 'NONE',  ( 22.61462763620000160, 0.2954212214349751786, -6.495682540442993869 ) ) ;
#29722 = B_SPLINE_CURVE_WITH_KNOTS ( 'NONE', 3,
 ( #37018, #34374, #17861, #18687 ),
 .UNSPECIFIED., .F., .F.,
 ( 4, 4 ),
 ( 1.939479807224432123E-18, 6.391136169993889733E-06 ),
 .UNSPECIFIED. ) ;
#29723 = LINE ( 'NONE', #10974, #626 ) ;
#29724 = ORIENTED_EDGE ( 'NONE', *, *, #7770, .F. ) ;
#29725 = CARTESIAN_POINT ( 'NONE',  ( 25.73195067821911763, 2.635022193550605074, -3.526316274269030160 ) ) ;
#29726 = CARTESIAN_POINT ( 'NONE',  ( 4.588767459758324848E-15, -39.37473357531881391, 6.000000000000000000 ) ) ;
#29727 = CARTESIAN_POINT ( 'NONE',  ( 3.296802056245847545, -32.68464828369553743, 7.006908160621408754 ) ) ;
#29728 = CARTESIAN_POINT ( 'NONE',  ( 5.109556576806802752, -30.36213210669178153, 6.980586498568967180 ) ) ;
#29729 = CARTESIAN_POINT ( 'NONE',  ( -72.46964309959683703, 39.11862660440054640, 15.50000000000000000 ) ) ;
#29730 = CARTESIAN_POINT ( 'NONE',  ( -66.99872204295122913, 28.48507918597134037, 12.49999999999999645 ) ) ;
#29731 = CARTESIAN_POINT ( 'NONE',  ( 2.105750943142600029, -32.94567937155306225, 7.013842709614101167 ) ) ;
#29732 = CARTESIAN_POINT ( 'NONE',  ( 4.562230772466533857, -27.72120552588419784, 7.139196562012274150 ) ) ;
#29733 = ORIENTED_EDGE ( 'NONE', *, *, #7068, .T. ) ;
#29734 = CARTESIAN_POINT ( 'NONE',  ( 66.41604928081299875, 57.80773248233388983, 4.000000000000020428 ) ) ;
#29735 = CARTESIAN_POINT ( 'NONE',  ( 72.38109545502503295, 59.26788356430734694, -3.856543183738433633 ) ) ;
#29736 = AXIS2_PLACEMENT_3D ( 'NONE', #25347, #37886, #235 ) ;
#29737 = VERTEX_POINT ( 'NONE', #9807 ) ;
#29738 = CARTESIAN_POINT ( 'NONE',  ( 85.17103880321602105, 1.638380925414154587, -5.247232096711407223 ) ) ;
#29739 = FACE_OUTER_BOUND ( 'NONE', #21708, .T. ) ;
#29740 = VECTOR ( 'NONE', #15309, 1000.000000000000000 ) ;
#29741 = EDGE_CURVE ( 'NONE', #5741, #28543, #14573, .T. ) ;
#29742 = CARTESIAN_POINT ( 'NONE',  ( 2.863609035986292461, -26.26888160889163615, 7.697032948437507294 ) ) ;
#29743 = SHAPE_DEFINITION_REPRESENTATION ( #25745, #23772 ) ;
#29744 = CARTESIAN_POINT ( 'NONE',  ( -4.890026461918809630, -25.50263309590217276, 6.000000000000001776 ) ) ;
#29745 = ADVANCED_FACE ( 'NONE', ( #23664 ), #26963, .F. ) ;
#29746 = LINE ( 'NONE', #1558, #29212 ) ;
#29747 = DIRECTION ( 'NONE',  ( 0.000000000000000000, 0.000000000000000000, 1.000000000000000000 ) ) ;
#29748 = ORIENTED_EDGE ( 'NONE', *, *, #37145, .T. ) ;
#29749 = VERTEX_POINT ( 'NONE', #39509 ) ;
#29750 = CARTESIAN_POINT ( 'NONE',  ( 80.87678155331657592, 61.19751495238254790, -1.521414672925269995 ) ) ;
#29751 = CYLINDRICAL_SURFACE ( 'NONE', #40105, 0.1000000000000028644 ) ;
#29752 = CARTESIAN_POINT ( 'NONE',  ( 80.95922275190024209, 61.28229338972336393, 1.760837461004386428 ) ) ;
#29753 = ADVANCED_FACE ( 'NONE', ( #32061 ), #6321, .F. ) ;
#29754 = DIRECTION ( 'NONE',  ( 0.000000000000000000, 0.000000000000000000, -1.000000000000000000 ) ) ;
#29755 = FACE_BOUND ( 'NONE', #20776, .T. ) ;
#29756 = CARTESIAN_POINT ( 'NONE',  ( -0.5390062018526512455, -32.25974509032589310, 7.635761828346574021 ) ) ;
#29757 = FACE_OUTER_BOUND ( 'NONE', #26767, .T. ) ;
#29758 = CARTESIAN_POINT ( 'NONE',  ( 21.85643539959775694, 3.570402768353612810, -13.15459721397892423 ) ) ;
#29759 = CYLINDRICAL_SURFACE ( 'NONE', #8153, 3.399999999999999911 ) ;
#29760 = ORIENTED_EDGE ( 'NONE', *, *, #11518, .T. ) ;
#29761 = CARTESIAN_POINT ( 'NONE',  ( -20.44874870218064444, -26.64985754041175525, 6.700000000000000178 ) ) ;
#29762 = AXIS2_PLACEMENT_3D ( 'NONE', #35099, #22933, #35895 ) ;
#29763 = CARTESIAN_POINT ( 'NONE',  ( 14.75543128875859722, -5.142877266070694731, 2.500000000018098856 ) ) ;
#29764 = CARTESIAN_POINT ( 'NONE',  ( -72.95888282680236614, 1.037983118628833745, -10.95077940476028644 ) ) ;
#29765 = CARTESIAN_POINT ( 'NONE',  ( 1.545182540459093978, -32.96639982778489752, 6.871394612369935651 ) ) ;
#29766 = CARTESIAN_POINT ( 'NONE',  ( 2.392808652600788122, -26.24116651948626000, 6.864651958020304257 ) ) ;
#29767 = CARTESIAN_POINT ( 'NONE',  ( 80.38786582577540685, 64.30167536105096815, 3.588566286536285510 ) ) ;
#29768 = CARTESIAN_POINT ( 'NONE',  ( -70.92837670882107659, -27.85319909218681644, 0.000000000000000000 ) ) ;
#29769 = CYLINDRICAL_SURFACE ( 'NONE', #9531, 2.500000000000002220 ) ;
#29770 = LINE ( 'NONE', #7076, #20598 ) ;
#29771 = CARTESIAN_POINT ( 'NONE',  ( 27.43879754216082389, 0.9604377377020558715, 4.488885984917203587 ) ) ;
#29772 = DIRECTION ( 'NONE',  ( 0.000000000000000000, 0.000000000000000000, 1.000000000000000000 ) ) ;
#29773 = AXIS2_PLACEMENT_3D ( 'NONE', #33319, #5101, #17632 ) ;
#29774 = CARTESIAN_POINT ( 'NONE',  ( 86.46043323462474461, 1.241262327860113590, 4.894917242394325463 ) ) ;
#29775 = CARTESIAN_POINT ( 'NONE',  ( -26.24874870218063450, -26.64985754041175525, 6.700000000000000178 ) ) ;
#29776 = LINE ( 'NONE', #14324, #482 ) ;
#29777 = CARTESIAN_POINT ( 'NONE',  ( 67.65011695904739497, 58.50773134691538502, 3.985511447369839644 ) ) ;
#29778 = CARTESIAN_POINT ( 'NONE',  ( 35.33524896685774053, -3.237440951119502142, 5.721318206140924900 ) ) ;
#29779 = AXIS2_PLACEMENT_3D ( 'NONE', #12697, #27934, #40475 ) ;
#29780 = EDGE_CURVE ( 'NONE', #22791, #6415, #18249, .T. ) ;
#29781 = VERTEX_POINT ( 'NONE', #26469 ) ;
#29782 = CARTESIAN_POINT ( 'NONE',  ( -56.59682361629209879, 30.63869417066593925, 4.000000000000000000 ) ) ;
#29784 = EDGE_CURVE ( 'NONE', #11160, #13150, #1641, .T. ) ;
#29783 = CARTESIAN_POINT ( 'NONE',  ( 87.25532471891827413, 0.3484024848758522364, -5.186905954794287510 ) ) ;
#29786 = CARTESIAN_POINT ( 'NONE',  ( -0.4920901558482355109, -26.84171968718031209, 6.867280401193709416 ) ) ;
#29785 = CARTESIAN_POINT ( 'NONE',  ( 79.12779906683437048, 65.83686883797783196, -2.419967184825690953 ) ) ;
#29787 = CARTESIAN_POINT ( 'NONE',  ( 4.362362031624546610, -27.29750568242585018, 7.660770905198782899 ) ) ;
#29788 = PRESENTATION_LAYER_ASSIGNMENT (  '', '', ( #15334 ) ) ;
#29789 = CARTESIAN_POINT ( 'NONE',  ( 2.427704393887406109, -26.14656945195773119, 7.754798119455333705 ) ) ;
#29790 = VERTEX_POINT ( 'NONE', #30316 ) ;
#29791 = CARTESIAN_POINT ( 'NONE',  ( 0.8619263339206710839, -26.26760762817584549, 7.505001789837626447 ) ) ;
#29792 = PLANE ( 'NONE',  #40458 ) ;
#29793 = EDGE_CURVE ( 'NONE', #5201, #2909, #39778, .T. ) ;
#29794 = ORIENTED_EDGE ( 'NONE', *, *, #40215, .F. ) ;
#29795 = CYLINDRICAL_SURFACE ( 'NONE', #30750, 2.500000000000002220 ) ;
#29796 = EDGE_CURVE ( 'NONE', #35457, #37237, #18147, .T. ) ;
#29797 = CARTESIAN_POINT ( 'NONE',  ( 79.10907727509470533, 65.55534887285777756, -2.778975589575376937 ) ) ;
#29798 = SHAPE_REPRESENTATION ( 'Hinge', ( #30744 ), #31385 ) ;
#29799 = CARTESIAN_POINT ( 'NONE',  ( 8.290806648384990041, -25.50263309590217276, 27.90461065042423527 ) ) ;
#29800 = CARTESIAN_POINT ( 'NONE',  ( 80.85530923529174174, 62.40557805022640991, 3.206617288017366452 ) ) ;
#29801 = CARTESIAN_POINT ( 'NONE',  ( 22.17211141822430420, 0.6012630956800495419, 7.008217722012737738 ) ) ;
#29803 = VERTEX_POINT ( 'NONE', #31957 ) ;
#29802 = DIRECTION ( 'NONE',  ( -0.000000000000000000, 1.000000000000000000, -0.000000000000000000 ) ) ;
#29804 = AXIS2_PLACEMENT_3D ( 'NONE', #32478, #13737, #32878 ) ;
#29805 = CARTESIAN_POINT ( 'NONE',  ( -0.1003419751943278176, -32.45391518135897968, 7.759451378593096749 ) ) ;
#29807 = DIRECTION ( 'NONE',  ( 0.000000000000000000, -0.000000000000000000, -1.000000000000000000 ) ) ;
#29806 = CARTESIAN_POINT ( 'NONE',  ( 82.38753728249152175, 5.816132372599501110, -6.000000000000000888 ) ) ;
#29808 = CARTESIAN_POINT ( 'NONE',  ( -70.92837670882107659, -27.85319909218681644, 4.357836081054403010 ) ) ;
#29809 = CARTESIAN_POINT ( 'NONE',  ( -10.24874870218063450, -25.49307895267003587, 6.700000000000000178 ) ) ;
#29810 = DIRECTION ( 'NONE',  ( 0.4582725098355734938, -0.8888117386314180468, 0.000000000000000000 ) ) ;
#29811 = CARTESIAN_POINT ( 'NONE',  ( 23.41598892685735578, 3.603782756865482106, -3.423970361731152323 ) ) ;
#29812 = ORIENTED_EDGE ( 'NONE', *, *, #5823, .T. ) ;
#29813 = FACE_OUTER_BOUND ( 'NONE', #6838, .T. ) ;
#29814 = CARTESIAN_POINT ( 'NONE',  ( 21.85643539959775694, 0.06084538214464753347, 12.63034898425695296 ) ) ;
#29815 = CARTESIAN_POINT ( 'NONE',  ( 21.86951112228125282, 3.097095171886816711, 3.923778634572944846 ) ) ;
#29816 = CARTESIAN_POINT ( 'NONE',  ( 16.63788116708428078, 9.878167618073407041, 2.500000000000023537 ) ) ;
#29817 = CARTESIAN_POINT ( 'NONE',  ( 0.3451799453360092085, -32.68817016762459104, 6.979335674598003969 ) ) ;
#29818 = CARTESIAN_POINT ( 'NONE',  ( 85.76120202873109122, 1.723374722402979620, 5.285180586055219898 ) ) ;
#29819 = CARTESIAN_POINT ( 'NONE',  ( -0.5124851502560604510, -26.98861595202439290, 7.692469944509195301 ) ) ;
#29820 = ORIENTED_EDGE ( 'NONE', *, *, #19158, .T. ) ;
#29821 = DIRECTION ( 'NONE',  ( -0.000000000000000000, -0.000000000000000000, -1.000000000000000000 ) ) ;
#29822 = CARTESIAN_POINT ( 'NONE',  ( -81.51102537425536809, -5.630155644727341979, 2.768663238321263265 ) ) ;
#29823 = ADVANCED_FACE ( 'NONE', ( #9090 ), #2954, .F. ) ;
#29824 = CARTESIAN_POINT ( 'NONE',  ( 21.78047233922835346, 5.616103166486084319, -3.473245622192032034 ) ) ;
#29825 = CARTESIAN_POINT ( 'NONE',  ( 19.67202969158519821, -2.692786188159640659, -3.276694021844582583 ) ) ;
#29826 = CARTESIAN_POINT ( 'NONE',  ( 36.79718629682508180, -2.556927207590028672, -5.949488883569893360 ) ) ;
#29827 = CARTESIAN_POINT ( 'NONE',  ( -22.34874870218063947, -26.64985754041175525, 6.700000000000000178 ) ) ;
#29828 = DIRECTION ( 'NONE',  ( 0.000000000000000000, 0.000000000000000000, 1.000000000000000000 ) ) ;
#29829 = DIRECTION ( 'NONE',  ( 1.000000000000000000, 6.938893903907229167E-15, 0.000000000000000000 ) ) ;
#29830 = ORIENTED_EDGE ( 'NONE', *, *, #23204, .T. ) ;
#29831 = FACE_OUTER_BOUND ( 'NONE', #20667, .T. ) ;
#29832 = DIRECTION ( 'NONE',  ( 0.2666961468790325918, 0.9637806624122924326, 0.000000000000000000 ) ) ;
#29833 = CIRCLE ( 'NONE', #5502, 2.500000000000002220 ) ;
#29834 = AXIS2_PLACEMENT_3D ( 'NONE', #34859, #6635, #31747 ) ;
#29835 = CARTESIAN_POINT ( 'NONE',  ( -1.168676970653521163, -27.74552502474002225, 6.868387053540521592 ) ) ;
#29836 = VERTEX_POINT ( 'NONE', #28442 ) ;
#29837 = ORIENTED_EDGE ( 'NONE', *, *, #39077, .T. ) ;
#29838 = CARTESIAN_POINT ( 'NONE',  ( 32.06910790505158104, 0.2527932190318202266, 4.727196575052298400 ) ) ;
#29839 = CARTESIAN_POINT ( 'NONE',  ( -1.640646438711915733, -30.61277402592531871, 6.887547729233687299 ) ) ;
#29840 = DIRECTION ( 'NONE',  ( 0.000000000000000000, 1.000000000000000000, 0.000000000000000000 ) ) ;
#29841 = CARTESIAN_POINT ( 'NONE',  ( 86.62542987116634663, -0.8173961967003109397, 5.560941923137655785 ) ) ;
#29842 = EDGE_CURVE ( 'NONE', #19316, #1269, #22226, .T. ) ;
#29843 = EDGE_CURVE ( 'NONE', #34207, #17544, #20376, .T. ) ;
#29844 = AXIS2_PLACEMENT_3D ( 'NONE', #11144, #4782, #1710 ) ;
#29845 = ORIENTED_EDGE ( 'NONE', *, *, #27737, .T. ) ;
#29846 = ADVANCED_FACE ( 'NONE', ( #7827 ), #38306, .F. ) ;
#29847 = ORIENTED_EDGE ( 'NONE', *, *, #39545, .F. ) ;
#29848 = LINE ( 'NONE', #1659, #32574 ) ;
#29849 = VECTOR ( 'NONE', #9097, 1000.000000000000000 ) ;
#29850 = SHAPE_REPRESENTATION_RELATIONSHIP ( 'NONE' , 'NONE' ,  #39533, #22994 ) ;
#29851 = EDGE_LOOP ( 'NONE', ( #5918, #34141, #5808 ) ) ;
#29852 = CARTESIAN_POINT ( 'NONE',  ( -57.26775771055921638, 29.21795897888110005, -2.148764163877388444 ) ) ;
#29854 = CARTESIAN_POINT ( 'NONE',  ( 4.289004371442884711, -27.36559100360608454, 7.740055089680401679 ) ) ;
#29853 = SURFACE_SIDE_STYLE ('',( #1664 ) ) ;
#29855 = ORIENTED_EDGE ( 'NONE', *, *, #17452, .F. ) ;
#29856 = CARTESIAN_POINT ( 'NONE',  ( 22.68640543563817857, 4.358088089980108215, 3.272418636457262053 ) ) ;
#29857 = CARTESIAN_POINT ( 'NONE',  ( 82.26850461147272142, 62.50126132183002170, -1.564050819714059681 ) ) ;
#29858 = FACE_OUTER_BOUND ( 'NONE', #35236, .T. ) ;
#29859 = ORIENTED_EDGE ( 'NONE', *, *, #22203, .F. ) ;
#29861 = CARTESIAN_POINT ( 'NONE',  ( 28.29477944214842822, -2.858814435932810483, -4.622482662410751786 ) ) ;
#29860 = DIRECTION ( 'NONE',  ( 0.000000000000000000, 1.000000000000000000, 0.000000000000000000 ) ) ;
#29862 = CARTESIAN_POINT ( 'NONE',  ( 5.401390093233090717, -29.51577928193538369, 7.695279973900954751 ) ) ;
#29863 = CARTESIAN_POINT ( 'NONE',  ( 75.34312381977423456, 60.33875818837522331, 3.724166978290133212 ) ) ;
#29864 = CARTESIAN_POINT ( 'NONE',  ( 24.65008494010616147, 2.678007333153050951, -3.905301012187318843 ) ) ;
#29865 = DIRECTION ( 'NONE',  ( 0.7660444431189857850, -0.6427876096865299260, -0.000000000000000000 ) ) ;
#29866 = CARTESIAN_POINT ( 'NONE',  ( 14.77500745536057813, -5.175466302041957789, 2.500000552286355759 ) ) ;
#29867 = CARTESIAN_POINT ( 'NONE',  ( -60.92837670882106238, -23.80776546975053165, 0.000000000000000000 ) ) ;
#29868 = CARTESIAN_POINT ( 'NONE',  ( -80.92837670882107659, 2.429809908903242555, 12.50000000000000000 ) ) ;
#29869 = CARTESIAN_POINT ( 'NONE',  ( 1.684177654150519787, -26.06996773262067890, 7.638991368224661294 ) ) ;
#29870 = CARTESIAN_POINT ( 'NONE',  ( 81.94417840557107979, 63.58970459987536827, 2.726953404243151358 ) ) ;
#29871 = CARTESIAN_POINT ( 'NONE',  ( 85.27007178914716690, 2.578332801382848594, -1.917248250713118773 ) ) ;
#29872 = CARTESIAN_POINT ( 'NONE',  ( 32.92332271219583362, -2.910100397871670186, 5.759571882993297365 ) ) ;
#29873 = CARTESIAN_POINT ( 'NONE',  ( -0.2487487021806331078, -25.49307895267003587, 6.700000000000000178 ) ) ;
#29874 = CARTESIAN_POINT ( 'NONE',  ( -71.68313049177861274, -45.80610001491483985, 9.973116064590190177 ) ) ;
#29875 = VECTOR ( 'NONE', #26356, 1000.000000000000000 ) ;
#29876 = CARTESIAN_POINT ( 'NONE',  ( -73.47531904699276595, -0.7173371340867340518, -10.88120764735859680 ) ) ;
#29877 = CARTESIAN_POINT ( 'NONE',  ( 14.81039496248155629, -5.583982002385155852, 2.503401465924845137 ) ) ;
#29878 = B_SPLINE_CURVE_WITH_KNOTS ( 'NONE', 3,
 ( #32721, #38465, #29612, #38670, #16636, #17240, #10468, #1431, #20532, #39065 ),
 .UNSPECIFIED., .F., .F.,
 ( 4, 2, 2, 2, 4 ),
 ( 1.084202172485504434E-19, 0.0003915841590506208693, 0.0007831683181012415217, 0.001174752477151862120, 0.001566336636202482393 ),
 .UNSPECIFIED. ) ;
#29879 = DIRECTION ( 'NONE',  ( -1.000000000000000000, 0.000000000000000000, 0.000000000000000000 ) ) ;
#29880 = CARTESIAN_POINT ( 'NONE',  ( 33.45607284416932004, -3.169907100080228801, -5.428027324148745336 ) ) ;
#29881 = CARTESIAN_POINT ( 'NONE',  ( -69.08758708074093136, -65.19654454972992141, 3.800414904976363140 ) ) ;
#29882 = CYLINDRICAL_SURFACE ( 'NONE', #33838, 0.09010775117052746697 ) ;
#29883 = CARTESIAN_POINT ( 'NONE',  ( -1.564068802536003444, -28.34413493684503749, 7.783750581861600182 ) ) ;
#29884 = FACE_OUTER_BOUND ( 'NONE', #38969, .T. ) ;
#29885 = ORIENTED_EDGE ( 'NONE', *, *, #34007, .F. ) ;
#29886 = CARTESIAN_POINT ( 'NONE',  ( 36.47586202471227779, -3.472083087333631468, 5.836410874819898176 ) ) ;
#29887 = DIRECTION ( 'NONE',  ( 1.000000000000000000, 0.000000000000000000, 0.000000000000000000 ) ) ;
#29888 = CARTESIAN_POINT ( 'NONE',  ( 67.41558015167861129, 58.24452080056473591, -3.997009152755513384 ) ) ;
#29889 = CARTESIAN_POINT ( 'NONE',  ( 3.065628457177692390, -26.34717386365430869, 6.998987538705432776 ) ) ;
#29890 = AXIS2_PLACEMENT_3D ( 'NONE', #26801, #5579, #2517 ) ;
#29891 = EDGE_LOOP ( 'NONE', ( #28718, #29640, #19149, #27920, #3825 ) ) ;
#29892 = AXIS2_PLACEMENT_3D ( 'NONE', #16848, #15492, #34464 ) ;
#29893 = FACE_OUTER_BOUND ( 'NONE', #27402, .T. ) ;
#29895 = EDGE_CURVE ( 'NONE', #21734, #301, #33381, .T. ) ;
#29894 = CARTESIAN_POINT ( 'NONE',  ( 5.889993154240193540, -27.29372336251594078, 6.954324564059724878 ) ) ;
#29896 = CARTESIAN_POINT ( 'NONE',  ( 78.56550182460473764, 65.96991646449161806, 1.378756462391438786 ) ) ;
#29897 = FACE_BOUND ( 'NONE', #27809, .T. ) ;
#29898 = CARTESIAN_POINT ( 'NONE',  ( 3.613287768474986450, -26.63891821509542623, 6.971170733404102648 ) ) ;
#29899 = LINE ( 'NONE', #11547, #21876 ) ;
#29900 = EDGE_LOOP ( 'NONE', ( #3999, #10383, #383, #28303, #33129 ) ) ;
#29901 = CARTESIAN_POINT ( 'NONE',  ( 23.43270483355060563, 3.786512555878049024, 3.121339484469592307 ) ) ;
#29902 =( LENGTH_UNIT ( ) NAMED_UNIT ( * ) SI_UNIT ( .MILLI., .METRE. ) );
#29903 = VECTOR ( 'NONE', #12168, 1000.000000000000000 ) ;
#29904 = CARTESIAN_POINT ( 'NONE',  ( 80.06561887301042191, 64.50783488872738758, 3.572022490087454649 ) ) ;
#29905 = CARTESIAN_POINT ( 'NONE',  ( 29.25516034266419396, -9.786766584782256473, -2.500000000000003997 ) ) ;
#29906 = EDGE_LOOP ( 'NONE', ( #28828, #4016 ) ) ;
#29907 = CARTESIAN_POINT ( 'NONE',  ( 78.26672476572068149, 63.69414582742361119, -3.691425412862290756 ) ) ;
#29909 = CARTESIAN_POINT ( 'NONE',  ( 14.75295547215416292, -4.607810090512766799, -2.508621623712387283 ) ) ;
#29908 = CARTESIAN_POINT ( 'NONE',  ( 23.05353214843946574, 0.3448042878357789331, 5.959785611882738365 ) ) ;
#29910 = CARTESIAN_POINT ( 'NONE',  ( 81.16342859511064489, 63.93697670172024061, -3.375310687856056369 ) ) ;
#29911 = CARTESIAN_POINT ( 'NONE',  ( 77.70122879141796091, 65.35873351754847249, 2.061059937946295495 ) ) ;
#29912 = CARTESIAN_POINT ( 'NONE',  ( 37.09585205635672622, -3.161667249977912597, -5.975077866033308815 ) ) ;
#29913 = CARTESIAN_POINT ( 'NONE',  ( 82.47906632153727458, 63.16918237499284317, 1.623788564013678659 ) ) ;
#29914 = CARTESIAN_POINT ( 'NONE',  ( 14.69558838330753936, 10.99631180437154399, -6.000000000000000888 ) ) ;
#29915 = CARTESIAN_POINT ( 'NONE',  ( 27.88065694771982450, 2.580388505813413502, -1.055963728923108524 ) ) ;
#29916 = EDGE_CURVE ( 'NONE', #39584, #10407, #20573, .T. ) ;
#29917 = CARTESIAN_POINT ( 'NONE',  ( -64.12237394559149095, 36.72939681796546552, -5.075523754374912322 ) ) ;
#29918 = ORIENTED_EDGE ( 'NONE', *, *, #25313, .F. ) ;
#29919 = CARTESIAN_POINT ( 'NONE',  ( -81.24448366233951901, -5.645114717358096001, 3.737607825908031867 ) ) ;
#29920 = CARTESIAN_POINT ( 'NONE',  ( 25.40499790527096380, 0.6691154281967053308, -4.599878778758904829 ) ) ;
#29921 = CARTESIAN_POINT ( 'NONE',  ( -0.8954611659357714082, -31.76573441880953297, 7.635761828346577573 ) ) ;
#29922 = CIRCLE ( 'NONE', #16775, 0.1000000000000028644 ) ;
#29923 = VECTOR ( 'NONE', #22186, 1000.000000000000000 ) ;
#29924 = CARTESIAN_POINT ( 'NONE',  ( 5.174635964963624879, -29.14611934969121521, 6.921725064902952695 ) ) ;
#29925 = CARTESIAN_POINT ( 'NONE',  ( 35.82496331154815294, -3.676156692585681895, -5.658730661258451811 ) ) ;
#29926 = CARTESIAN_POINT ( 'NONE',  ( -30.87867591359218977, -24.55319635012989110, 6.700000000000000178 ) ) ;
#29927 = AXIS2_PLACEMENT_3D ( 'NONE', #736, #13273, #38378 ) ;
#29928 = CARTESIAN_POINT ( 'NONE',  ( 3.295286368285633483, -32.68543217743695095, 6.903112506833884332 ) ) ;
#29929 = DIRECTION ( 'NONE',  ( 0.000000000000000000, 0.000000000000000000, 1.000000000000000000 ) ) ;
#29930 = CARTESIAN_POINT ( 'NONE',  ( -75.45330471031414277, 33.71485196875532608, 12.49999999999999645 ) ) ;
#29931 = PLANE ( 'NONE',  #18072 ) ;
#29932 = CARTESIAN_POINT ( 'NONE',  ( 5.094318823446379874, -29.77302566397534278, 6.988553391373226731 ) ) ;
#29933 = EDGE_CURVE ( 'NONE', #16079, #17495, #31092, .T. ) ;
#29934 = DIRECTION ( 'NONE',  ( -0.000000000000000000, -0.000000000000000000, 1.000000000000000000 ) ) ;
#29935 = CARTESIAN_POINT ( 'NONE',  ( 2.124200926935305045, -33.04417605512392697, 6.921725064902950031 ) ) ;
#29936 = ORIENTED_EDGE ( 'NONE', *, *, #30824, .T. ) ;
#29937 = CARTESIAN_POINT ( 'NONE',  ( 66.27376694608996388, 57.73522568913447373, 4.000000000000000000 ) ) ;
#29938 = CARTESIAN_POINT ( 'NONE',  ( 73.18282872914367942, 62.10277071170013841, -3.478821770299028948 ) ) ;
#29939 = ORIENTED_EDGE ( 'NONE', *, *, #39181, .T. ) ;
#29940 = CARTESIAN_POINT ( 'NONE',  ( 85.83023444425720072, 0.8841707150779518631, 5.891289308415252890 ) ) ;
#29942 = EDGE_CURVE ( 'NONE', #2870, #4585, #9446, .T. ) ;
#29941 = DIRECTION ( 'NONE',  ( -7.215117721222287909E-15, -0.8314686954258618812, 0.5555716052200790900 ) ) ;
#29943 = EDGE_CURVE ( 'NONE', #37531, #1662, #15221, .T. ) ;
#29944 = CARTESIAN_POINT ( 'NONE',  ( -1.425774885472621767, -28.23310838303483550, 7.013842709614101167 ) ) ;
#29945 = PLANE ( 'NONE',  #16898 ) ;
#29946 = APPLICATION_PROTOCOL_DEFINITION ( 'draft international standard', 'automotive_design', 1998, #11825 ) ;
#29947 = CARTESIAN_POINT ( 'NONE',  ( 6.017943466947773601, -29.68303111057383248, 6.894806418505347700 ) ) ;
#29948 = CARTESIAN_POINT ( 'NONE',  ( 23.44524387940805354, 3.803759871792764091, 3.069313877683408354 ) ) ;
#29949 = DIRECTION ( 'NONE',  ( -0.000000000000000000, 1.000000000000000000, -0.000000000000000000 ) ) ;
#29950 = VECTOR ( 'NONE', #23600, 1000.000000000000000 ) ;
#29951 = AXIS2_PLACEMENT_3D ( 'NONE', #31283, #34796, #37434 ) ;
#29952 = B_SPLINE_CURVE_WITH_KNOTS ( 'NONE', 3,
 ( #11105, #16881, #29463, #17277 ),
 .UNSPECIFIED., .F., .F.,
 ( 4, 4 ),
 ( 0.000000000000000000, 1.000000000000000000 ),
 .UNSPECIFIED. ) ;
#29953 = ORIENTED_EDGE ( 'NONE', *, *, #10637, .T. ) ;
#29954 = EDGE_LOOP ( 'NONE', ( #27072, #20565, #38110, #9223 ) ) ;
#29955 = CARTESIAN_POINT ( 'NONE',  ( 80.02751534128088906, 63.03952351013455768, -3.681573067026197243 ) ) ;
#29956 = CARTESIAN_POINT ( 'NONE',  ( 37.14378633834282795, -2.493312693697226301, 5.967573678773149481 ) ) ;
#29957 = CARTESIAN_POINT ( 'NONE',  ( 80.85057025077259141, 61.36744894077060763, 2.123311106147461658 ) ) ;
#29959 = ORIENTED_EDGE ( 'NONE', *, *, #12055, .T. ) ;
#29958 = CARTESIAN_POINT ( 'NONE',  ( 0.5480081280804431909, -26.37116720998445984, 7.775108481317162479 ) ) ;
#29960 = VECTOR ( 'NONE', #18859, 1000.000000000000000 ) ;
#29961 = EDGE_CURVE ( 'NONE', #35449, #29634, #39055, .T. ) ;
#29962 = DIRECTION ( 'NONE',  ( -0.000000000000000000, 0.000000000000000000, -1.000000000000000000 ) ) ;
#29963 = CARTESIAN_POINT ( 'NONE',  ( 4.034911153157309194, -27.09807998479585578, 6.911401339314957148 ) ) ;
#29964 = CARTESIAN_POINT ( 'NONE',  ( 17.36972370856863535, 14.26801361678851343, 2.499999999999999112 ) ) ;
#29965 = CARTESIAN_POINT ( 'NONE',  ( 21.85643539959775694, 5.983772091205654675, 13.40455955530236487 ) ) ;
#29966 = DIRECTION ( 'NONE',  ( 0.9267318687906764829, -0.3757233601570978965, 0.000000000000000000 ) ) ;
#29967 = ORIENTED_EDGE ( 'NONE', *, *, #25654, .F. ) ;
#29968 = CARTESIAN_POINT ( 'NONE',  ( -81.79890681550139675, 10.46299657128043492, 0.6911394749367770762 ) ) ;
#29969 = DIRECTION ( 'NONE',  ( 0.000000000000000000, 1.000000000000000000, 0.000000000000000000 ) ) ;
#29970 = CARTESIAN_POINT ( 'NONE',  ( -76.50781846841695710, 9.203653447225347506, -9.788468040724580987 ) ) ;
#29971 = CARTESIAN_POINT ( 'NONE',  ( 37.11062810659152689, -2.402986199528067246, -5.951436016291230757 ) ) ;
#29972 = CARTESIAN_POINT ( 'NONE',  ( 81.06839910345442490, 62.80152057670050425, 3.286127602909470813 ) ) ;
#29973 = CARTESIAN_POINT ( 'NONE',  ( -1.492713901548710531, -30.73790092008425745, 7.763628509615288387 ) ) ;
#29974 = CARTESIAN_POINT ( 'NONE',  ( 3.939361713728871006, -27.01119860913185633, 7.784476445165074310 ) ) ;
#29975 = DIRECTION ( 'NONE',  ( -0.000000000000000000, -0.000000000000000000, -1.000000000000000000 ) ) ;
#29976 = CARTESIAN_POINT ( 'NONE',  ( 31.16472951934800406, -0.3606997634973788669, 5.070407781962654958 ) ) ;
#29977 = EDGE_CURVE ( 'NONE', #10008, #25619, #32314, .T. ) ;
#29978 = ADVANCED_FACE ( 'NONE', ( #20523 ), #30212, .F. ) ;
#29979 = EDGE_CURVE ( 'NONE', #9808, #14204, #11684, .T. ) ;
#29980 = VECTOR ( 'NONE', #31417, 1000.000000000000227 ) ;
#29981 = CARTESIAN_POINT ( 'NONE',  ( 4.447923184078407921, -27.40171274082518238, 6.863784140767622333 ) ) ;
#29982 = CARTESIAN_POINT ( 'NONE',  ( 28.52663967383706023, 50.14399159706753295, 4.000000000000000000 ) ) ;
#29983 = CARTESIAN_POINT ( 'NONE',  ( 1.713892699967802136, -33.06990413752668445, 7.635761828346576685 ) ) ;
#29984 = CARTESIAN_POINT ( 'NONE',  ( 68.00738522489628224, 58.43930376306189345, 3.995571880668716602 ) ) ;
#29985 = CARTESIAN_POINT ( 'NONE',  ( 34.77093152648067331, -3.235628152337162167, 5.633242821496846631 ) ) ;
#29986 = CIRCLE ( 'NONE', #17502, 0.1000000000000028644 ) ;
#29987 = ORIENTED_EDGE ( 'NONE', *, *, #19032, .F. ) ;
#29988 = CARTESIAN_POINT ( 'NONE',  ( 2.307042206337215351, -33.01365871392055595, 7.767720160662275219 ) ) ;
#29989 = CARTESIAN_POINT ( 'NONE',  ( 85.81943862418182789, 1.961257897749014045, -4.406084401447566634 ) ) ;
#29991 = CARTESIAN_POINT ( 'NONE',  ( 27.43879703630890887, 0.9604363013853572939, -4.488885905966782275 ) ) ;
#29990 = CARTESIAN_POINT ( 'NONE',  ( 78.99338515863716736, 65.92867347524024524, -2.125034277891688639 ) ) ;
#29992 = CARTESIAN_POINT ( 'NONE',  ( -1.389564992689783951, -31.21326896663422090, 7.754798119455333705 ) ) ;
#29993 = ADVANCED_FACE ( 'NONE', ( #3272 ), #15989, .T. ) ;
#29994 = CARTESIAN_POINT ( 'NONE',  ( -1.638685409516953406, -28.92916437338612567, 6.892063359921932530 ) ) ;
#29995 = CARTESIAN_POINT ( 'NONE',  ( -58.76908243668979281, 27.83904476269672656, 5.922484465878444126 ) ) ;
#29996 = EDGE_LOOP ( 'NONE', ( #8199, #9907, #15047, #35690, #40462 ) ) ;
#29997 = DIRECTION ( 'NONE',  ( 0.000000000000000000, 0.000000000000000000, 1.000000000000000000 ) ) ;
#29998 = ORIENTED_EDGE ( 'NONE', *, *, #17179, .T. ) ;
#29999 = DIRECTION ( 'NONE',  ( 1.000000000000000000, 0.000000000000000000, 0.000000000000000000 ) ) ;
#30000 = ORIENTED_EDGE ( 'NONE', *, *, #25654, .T. ) ;
#30001 = CARTESIAN_POINT ( 'NONE',  ( 79.70909206056978746, 64.65202245283539639, -3.503057693382717996 ) ) ;
#30002 = DIRECTION ( 'NONE',  ( 0.000000000000000000, 0.000000000000000000, 1.000000000000000000 ) ) ;
#30003 = CARTESIAN_POINT ( 'NONE',  ( 81.09055442218992482, 61.42501475223632923, 1.950029235564090913 ) ) ;
#30004 = CARTESIAN_POINT ( 'NONE',  ( 23.18405951893644001, 0.8525072515736740186, 5.603743966958759870 ) ) ;
#30006 = EDGE_LOOP ( 'NONE', ( #27745, #24194 ) ) ;
#30005 = DIRECTION ( 'NONE',  ( 0.000000000000000000, 0.000000000000000000, 1.000000000000000000 ) ) ;
#30007 = EDGE_CURVE ( 'NONE', #35192, #15748, #9608, .T. ) ;
#30008 = CARTESIAN_POINT ( 'NONE',  ( 76.13754644452941989, 60.10671110989439825, -3.424891502433685453 ) ) ;
#30009 = DIRECTION ( 'NONE',  ( 0.000000000000000000, 0.000000000000000000, 1.000000000000000000 ) ) ;
#30011 = LINE ( 'NONE', #2033, #25602 ) ;
#30010 = CYLINDRICAL_SURFACE ( 'NONE', #30474, 0.1000000000000028644 ) ;
#30012 = DIRECTION ( 'NONE',  ( 1.000000000000000000, -0.000000000000000000, 0.000000000000000000 ) ) ;
#30013 = AXIS2_PLACEMENT_3D ( 'NONE', #37544, #6681, #21919 ) ;
#30014 = DIRECTION ( 'NONE',  ( -1.000000000000000000, 0.000000000000000000, 0.000000000000000000 ) ) ;
#30015 = CARTESIAN_POINT ( 'NONE',  ( 4.661322817598709811, -31.24112487228765289, 7.670860738520325128 ) ) ;
#30016 = CARTESIAN_POINT ( 'NONE',  ( 22.97618870714912731, 3.739651848979420379, -3.615343062961793752 ) ) ;
#30017 = ORIENTED_EDGE ( 'NONE', *, *, #34344, .T. ) ;
#30018 = LINE ( 'NONE', #1836, #17809 ) ;
#30019 = EDGE_CURVE ( 'NONE', #24473, #160, #36296, .T. ) ;
#30020 = CIRCLE ( 'NONE', #35315, 9.804803391925412726 ) ;
#30021 = CARTESIAN_POINT ( 'NONE',  ( 22.49677218534670331, -0.6234722885575160189, 9.207484322151008982 ) ) ;
#30022 = EDGE_CURVE ( 'NONE', #27165, #38247, #28489, .T. ) ;
#30023 = CARTESIAN_POINT ( 'NONE',  ( 21.89858680185338358, 3.819795204994611559, -2.126311674337833413 ) ) ;
#30024 = CARTESIAN_POINT ( 'NONE',  ( -0.9575113486053227208, -31.84711263666175540, 7.697032948437507294 ) ) ;
#30025 = CARTESIAN_POINT ( 'NONE',  ( -70.92837670882107659, 26.72470171467712063, 6.406751979251626317 ) ) ;
#30026 = CARTESIAN_POINT ( 'NONE',  ( 80.50924551447106126, 65.11801186546927056, 3.171364025132954456 ) ) ;
#30027 = CARTESIAN_POINT ( 'NONE',  ( 84.83925925549863223, 2.817044135119172399, -2.844581780382558378 ) ) ;
#30028 = PLANE ( 'NONE',  #4287 ) ;
#30029 = ORIENTED_EDGE ( 'NONE', *, *, #16858, .F. ) ;
#30030 = CARTESIAN_POINT ( 'NONE',  ( 11.65737507970504439, -29.56993018339339940, 6.800000000000000711 ) ) ;
#30031 = EDGE_CURVE ( 'NONE', #39661, #25969, #18949, .T. ) ;
#30032 = ORIENTED_EDGE ( 'NONE', *, *, #30293, .T. ) ;
#30033 = PLANE ( 'NONE',  #19713 ) ;
#30034 = CARTESIAN_POINT ( 'NONE',  ( 31.38022914977189259, -3.594042512269271850, -4.917870897524577067 ) ) ;
#30035 = CARTESIAN_POINT ( 'NONE',  ( 34.33233530168753589, -1.487613377254970226, -5.564789273131927949 ) ) ;
#30036 = CARTESIAN_POINT ( 'NONE',  ( -70.92837670882107659, 28.72470171467712063, 0.000000000000000000 ) ) ;
#30037 = CARTESIAN_POINT ( 'NONE',  ( 22.73363516861961742, 0.4005846852146681680, -6.310066893263544863 ) ) ;
#30038 = CARTESIAN_POINT ( 'NONE',  ( -0.4892492752782273691, -26.96886344085812937, 7.763628509615285722 ) ) ;
#30039 = ORIENTED_EDGE ( 'NONE', *, *, #11072, .F. ) ;
#30040 = CARTESIAN_POINT ( 'NONE',  ( 36.79674047955164440, -2.557473896570829908, 5.949419303002247972 ) ) ;
#30041 = VECTOR ( 'NONE', #14133, 1000.000000000000000 ) ;
#30042 = CARTESIAN_POINT ( 'NONE',  ( 4.985934790884831713, -28.36760422505889068, 7.762796336881261361 ) ) ;
#30043 = ORIENTED_EDGE ( 'NONE', *, *, #26829, .T. ) ;
#30044 = ORIENTED_EDGE ( 'NONE', *, *, #33332, .T. ) ;
#30045 = CARTESIAN_POINT ( 'NONE',  ( 36.71942053932279748, -3.459622343616183038, 5.860272900448393329 ) ) ;
#30046 =( BOUNDED_CURVE ( )  B_SPLINE_CURVE ( 3, ( #38927, #23103, #4573, #32581 ),
 .UNSPECIFIED., .F., .T. ) 
 B_SPLINE_CURVE_WITH_KNOTS ( ( 4, 4 ),
 ( 4.708531083176467291, 4.895802057644188743 ),
 .UNSPECIFIED. ) 
 CURVE ( )  GEOMETRIC_REPRESENTATION_ITEM ( )  RATIONAL_B_SPLINE_CURVE ( ( 1.000000000000000000, 0.9970795998553221295, 0.9970795998553221295, 1.000000000000000000 ) ) 
 REPRESENTATION_ITEM ( '' )  );
#30047 = CARTESIAN_POINT ( 'NONE',  ( 2.118032945466439276, -33.04492290971361257, 6.951256099901589991 ) ) ;
#30048 = CARTESIAN_POINT ( 'NONE',  ( -1.648135648921391416, -30.58844643467698887, 6.980586498568966292 ) ) ;
#30049 = CARTESIAN_POINT ( 'NONE',  ( 16.12381318270590924, -3.547307913324281081, -2.701813617103016263 ) ) ;
#30050 = VECTOR ( 'NONE', #39436, 1000.000000000000000 ) ;
#30051 = CARTESIAN_POINT ( 'NONE',  ( 14.67325355196851255, 12.62073864644707299, -2.499999999995972111 ) ) ;
#30052 = VECTOR ( 'NONE', #695, 1000.000000000000114 ) ;
#30053 = ORIENTED_EDGE ( 'NONE', *, *, #6804, .T. ) ;
#30054 = FACE_OUTER_BOUND ( 'NONE', #28537, .T. ) ;
#30055 = ORIENTED_EDGE ( 'NONE', *, *, #33353, .T. ) ;
#30056 = ORIENTED_EDGE ( 'NONE', *, *, #10684, .F. ) ;
#30057 = CARTESIAN_POINT ( 'NONE',  ( 1.217126534916886937, -26.10345411493373291, 7.750000000000000888 ) ) ;
#30058 = DIRECTION ( 'NONE',  ( 1.000000000000000000, 0.000000000000000000, 0.000000000000000000 ) ) ;
#30059 = DIRECTION ( 'NONE',  ( 1.000000000000000000, 0.000000000000000000, 0.000000000000000000 ) ) ;
#30060 = ORIENTED_EDGE ( 'NONE', *, *, #14385, .F. ) ;
#30062 = CARTESIAN_POINT ( 'NONE',  ( 4.343337730903781058, -27.43104547763413237, 7.785172627573962778 ) ) ;
#30061 = CARTESIAN_POINT ( 'NONE',  ( -60.15914593959029588, -52.45670913645259503, 2.307692307692319478 ) ) ;
#30063 = VERTEX_POINT ( 'NONE', #2548 ) ;
#30064 = CARTESIAN_POINT ( 'NONE',  ( 21.82594131963945827, 4.890129326492636430, 3.822364013852876496 ) ) ;
#30065 = CARTESIAN_POINT ( 'NONE',  ( 80.18989135007151958, 66.21456565649044990, -1.848245342697680815 ) ) ;
#30066 = CARTESIAN_POINT ( 'NONE',  ( -73.07498068578524908, 39.58105274722134226, -46.17089178453873188 ) ) ;
#30067 = VERTEX_POINT ( 'NONE', #40589 ) ;
#30068 = B_SPLINE_CURVE_WITH_KNOTS ( 'NONE', 3,
 ( #29374, #23195, #35767, #25681, #16793, #7741, #6945, #29572, #39015, #20096 ),
 .UNSPECIFIED., .F., .F.,
 ( 4, 3, 3, 4 ),
 ( 1.905904691864261185E-18, 3.025570593002930732E-05, 6.051145698343765372E-05, 6.468151674593734010E-05 ),
 .UNSPECIFIED. ) ;
#30070 = CARTESIAN_POINT ( 'NONE',  ( 1.077348629692890247, -26.22750088404879776, 7.670860738520330457 ) ) ;
#30069 = CARTESIAN_POINT ( 'NONE',  ( -73.16330946177717465, -60.53509472482660669, 0.000000000000000000 ) ) ;
#30071 = CARTESIAN_POINT ( 'NONE',  ( 0.5325725529551263993, -26.27050565893173228, 6.894806418505347700 ) ) ;
#30072 = CARTESIAN_POINT ( 'NONE',  ( 75.57967633106541427, 61.33476069914100748, 3.901127667181007119 ) ) ;
#30073 = CARTESIAN_POINT ( 'NONE',  ( 21.83838922799100146, 2.382728257201017996, -5.693891273926298346 ) ) ;
#30074 = VERTEX_POINT ( 'NONE', #25162 ) ;
#30075 = DIRECTION ( 'NONE',  ( 0.000000000000000000, 1.000000000000000000, 0.000000000000000000 ) ) ;
#30076 = VECTOR ( 'NONE', #20747, 1000.000000000000000 ) ;
#30077 = DIRECTION ( 'NONE',  ( 0.2666961468790325918, 0.9637806624122924326, 0.000000000000000000 ) ) ;
#30078 = CARTESIAN_POINT ( 'NONE',  ( -41.07867591359219972, -26.64985754041175525, 6.700000000000000178 ) ) ;
#30079 = CARTESIAN_POINT ( 'NONE',  ( -75.45330471031414277, 33.71485196875532608, -9.800414904976365804 ) ) ;
#30080 = DIRECTION ( 'NONE',  ( -1.000000000000000000, 0.000000000000000000, 0.000000000000000000 ) ) ;
#30081 = CARTESIAN_POINT ( 'NONE',  ( 79.97870788650307361, 66.10023056730548774, 2.166533184762201358 ) ) ;
#30082 = CARTESIAN_POINT ( 'NONE',  ( 88.26779375368444391, -0.7888507896528732521, -1.681504516799547710 ) ) ;
#30083 = CARTESIAN_POINT ( 'NONE',  ( 32.02118327030063227, -4.941963151977918578, 1.942379491845174444 ) ) ;
#30084 = CARTESIAN_POINT ( 'NONE',  ( -0.5596933955661176352, -26.89747389307597203, 7.635761828346574909 ) ) ;
#30085 = VECTOR ( 'NONE', #23885, 1000.000000000000114 ) ;
#30086 = CARTESIAN_POINT ( 'NONE',  ( 4.651281559046659630, -31.25879804726328004, 7.756377446753162097 ) ) ;
#30087 = AXIS2_PLACEMENT_3D ( 'NONE', #17426, #30014, #26924 ) ;
#30088 = ADVANCED_FACE ( 'NONE', ( #24966 ), #34452, .T. ) ;
#30089 = EDGE_CURVE ( 'NONE', #8440, #2282, #9648, .T. ) ;
#30090 = EDGE_CURVE ( 'NONE', #25861, #6597, #7958, .T. ) ;
#30091 = CYLINDRICAL_SURFACE ( 'NONE', #32073, 0.09010775117052929883 ) ;
#30092 = DIRECTION ( 'NONE',  ( -0.000000000000000000, -0.000000000000000000, 1.000000000000000000 ) ) ;
#30093 = DIRECTION ( 'NONE',  ( -0.000000000000000000, 0.000000000000000000, 1.000000000000000000 ) ) ;
#30094 = EDGE_CURVE ( 'NONE', #6701, #40686, #33090, .T. ) ;
#30095 = CARTESIAN_POINT ( 'NONE',  ( 36.46945287769039368, -2.309416368423244936, -5.898338157251335367 ) ) ;
#30096 = CARTESIAN_POINT ( 'NONE',  ( 4.636318400562632114, -31.47527517604001446, 6.912143950357340749 ) ) ;
#30097 = DIRECTION ( 'NONE',  ( 0.6427876096865379196, 0.7660444431189792347, -0.000000000000000000 ) ) ;
#30098 = B_SPLINE_CURVE_WITH_KNOTS ( 'NONE', 3,
 ( #29991, #11033, #4874, #23611, #14331, #33303, #5083, #8354, #21345, #36576, #27518, #17615, #36177, #36981, #8763, #20505, #33089, #26902, #11235, #30194, #2014, #21557, #25255, #28123, #8972, #27713, #18861, #15571, #31229, #15156, #5905, #40678, #25052, #3458, #3051, #31636, #2636, #18444, #40266, #15359, #31031, #2838, #22175, #31434, #27915, #9381, #12482, #40461, #6312, #37584, #21967, #34539, #12051, #24630 ),
 .UNSPECIFIED., .F., .F.,
 ( 4, 1, 1, 1, 2, 2, 1, 1, 1, 1, 1, 1, 2, 2, 1, 1, 1, 1, 1, 1, 1, 1, 2, 2, 1, 1, 1, 1, 2, 2, 1, 1, 1, 1, 1, 2, 2, 1, 1, 1, 1, 4 ),
 ( 0.3081789993805284511, 0.4811342495358507110, 0.4919439526705583487, 0.4973488042379122787, 0.4987000171297506501, 0.5000512300215890216, 0.5027536558052657645, 0.5243730620746801518, 0.5676118746135082604, 0.6108506871523364801, 0.6216603902870434517, 0.6243628160707210828, 0.6247006192936801483, 0.6250384225166392138, 0.6257140289625566787, 0.6270652418543913864, 0.6324700934217306614, 0.6540894996910853187, 0.7405671247685048364, 0.7459719763358438893, 0.7486744021195133048, 0.7493500085654295484, 0.7496878117883878367, 0.7500256150113457920, 0.7513768279031767250, 0.7621865310378237446, 0.7838059373071175617, 0.8054253435764113789, 0.8108301951437346666, 0.8135326209273960885, 0.8162350467110577323, 0.8270447498457029756, 0.8702835623842855028, 0.8729859881679464806, 0.8743372010597769695, 0.8746750042827347027, 0.8750128075056922139, 0.8756884139516074583, 0.8810932655189296359, 0.8919029686535726587, 0.9135223749228589263, 1.000000000000000000 ),
 .UNSPECIFIED. ) ;
#30099 = CARTESIAN_POINT ( 'NONE',  ( -63.08379346057677139, 18.80112958435941906, -46.17089178453873188 ) ) ;
#30100 = LINE ( 'NONE', #33409, #12527 ) ;
#30101 = ORIENTED_EDGE ( 'NONE', *, *, #38120, .T. ) ;
#30102 = CARTESIAN_POINT ( 'NONE',  ( 35.56290024310237641, -1.640810893426935646, 5.744602770279306547 ) ) ;
#30103 = CARTESIAN_POINT ( 'NONE',  ( -69.92837670882107659, -0.6719362264620037939, 3.916079783099610800 ) ) ;
#30104 = CARTESIAN_POINT ( 'NONE',  ( 67.37599051809213790, 58.35250968650521486, -3.990882853436547251 ) ) ;
#30105 = CARTESIAN_POINT ( 'NONE',  ( 1.121324086407811338, -26.64985754041175525, 6.700000000000000178 ) ) ;
#30106 = VECTOR ( 'NONE', #15996, 1000.000000000000227 ) ;
#30107 = VERTEX_POINT ( 'NONE', #36376 ) ;
#30108 = CARTESIAN_POINT ( 'NONE',  ( -0.4936289198477532558, -32.16730372678311767, 7.775108481317158926 ) ) ;
#30109 = DIRECTION ( 'NONE',  ( -0.9396926207859058744, -0.3420201433256757628, -0.000000000000000000 ) ) ;
#30110 = CARTESIAN_POINT ( 'NONE',  ( 77.23471303065964833, 65.03087687845577136, 2.276447073266238963 ) ) ;
#30111 = CARTESIAN_POINT ( 'NONE',  ( 1.046581363270776555, -32.90648473631282656, 6.880147297696980857 ) ) ;
#30112 = FACE_OUTER_BOUND ( 'NONE', #9476, .T. ) ;
#30113 = CARTESIAN_POINT ( 'NONE',  ( 1.253554297217517766, -26.09856357079008760, 6.887547729233691740 ) ) ;
#30114 = ORIENTED_EDGE ( 'NONE', *, *, #16102, .T. ) ;
#30115 = CARTESIAN_POINT ( 'NONE',  ( 21.83113904852917031, 5.958251073797080188, 3.138007096634494619 ) ) ;
#30116 = CARTESIAN_POINT ( 'NONE',  ( 82.18073233876086192, 62.22941084722766902, -1.168532795814369418 ) ) ;
#30117 = CARTESIAN_POINT ( 'NONE',  ( 79.39927235112092774, 65.46614203786569419, 2.932725070486263519 ) ) ;
#30118 = CARTESIAN_POINT ( 'NONE',  ( 24.20404138067665656, -8.556376197523151816, -2.500000000000003997 ) ) ;
#30119 = ORIENTED_EDGE ( 'NONE', *, *, #33012, .F. ) ;
#30120 = CARTESIAN_POINT ( 'NONE',  ( 79.57681890279654624, 60.99726435378322975, -2.643019404356985014 ) ) ;
#30122 = CARTESIAN_POINT ( 'NONE',  ( 2.258100775518462111, -26.21598130464280629, 7.670860738520328681 ) ) ;
#30121 = CARTESIAN_POINT ( 'NONE',  ( 24.74193054586557139, 0.5345309101367632376, 4.782337473183671861 ) ) ;
#30123 = CARTESIAN_POINT ( 'NONE',  ( 80.84588251005583004, 64.54609234697846887, -3.375310687856057257 ) ) ;
#30124 = CARTESIAN_POINT ( 'NONE',  ( 77.65795924533195205, 64.82981391430571705, 2.842954625922254674 ) ) ;
#30125 = CARTESIAN_POINT ( 'NONE',  ( -9.078675913592196167, -24.55319635012989110, 6.800000000000000711 ) ) ;
#30126 = CARTESIAN_POINT ( 'NONE',  ( 82.41151909044434376, 62.85445852417080914, 1.451695327222104703 ) ) ;
#30128 = CARTESIAN_POINT ( 'NONE',  ( 66.41194937274630661, -13.65448019739280028, -6.000000000000000000 ) ) ;
#30127 = CARTESIAN_POINT ( 'NONE',  ( 1.700390093233090871, -29.56993018339339940, 7.800000000000000711 ) ) ;
#30129 = CARTESIAN_POINT ( 'NONE',  ( 24.23947115566313926, 0.8503125907183233245, 6.739520400040675874 ) ) ;
#30130 = CYLINDRICAL_SURFACE ( 'NONE', #28651, 1.000000000000000888 ) ;
#30131 = CARTESIAN_POINT ( 'NONE',  ( 4.180804271322692500, -31.89534315857266122, 7.013842709614101167 ) ) ;
#30132 = ORIENTED_EDGE ( 'NONE', *, *, #34324, .T. ) ;
#30133 = CARTESIAN_POINT ( 'NONE',  ( -80.93488167894386720, -6.594418668544227202, -0.1886647716054447033 ) ) ;
#30134 = CARTESIAN_POINT ( 'NONE',  ( 24.12180912460078730, 0.4861797095442714767, -5.096561526129780972 ) ) ;
#30135 = DIRECTION ( 'NONE',  ( 1.000000000000000000, 0.000000000000000000, 0.000000000000000000 ) ) ;
#30136 = CARTESIAN_POINT ( 'NONE',  ( 5.152478333118308385, -28.99279347164636889, 6.894806418505347700 ) ) ;
#30137 = ADVANCED_FACE ( 'NONE', ( #24844 ), #30624, .F. ) ;
#30138 = CARTESIAN_POINT ( 'NONE',  ( 5.152444924565728890, -30.14726668966421386, 7.665454363767880253 ) ) ;
#30139 = CARTESIAN_POINT ( 'NONE',  ( 34.63540570288399323, -0.7851885325132845761, -5.278762693032814646 ) ) ;
#30140 = DIRECTION ( 'NONE',  ( 0.000000000000000000, 0.000000000000000000, 1.000000000000000000 ) ) ;
#30141 = FACE_OUTER_BOUND ( 'NONE', #12144, .T. ) ;
#30142 = CARTESIAN_POINT ( 'NONE',  ( 1.078588498108656424, -33.79778590424514562, 7.754798119455333705 ) ) ;
#30143 = LINE ( 'NONE', #14477, #37669 ) ;
#30144 = CARTESIAN_POINT ( 'NONE',  ( 2.663273245751797802, -32.83073627245006065, 6.949473656533215582 ) ) ;
#30145 = CARTESIAN_POINT ( 'NONE',  ( -72.99783146927553901, 4.029110416273074868, 10.94627121662267122 ) ) ;
#30146 = VECTOR ( 'NONE', #34277, 1000.000000000000000 ) ;
#30147 = DIRECTION ( 'NONE',  ( -0.1736481776669268062, 0.9848077530122086864, 0.000000000000000000 ) ) ;
#30148 = ORIENTED_EDGE ( 'NONE', *, *, #15482, .F. ) ;
#30149 = CARTESIAN_POINT ( 'NONE',  ( 66.42495344877985985, 57.78257748056745413, 4.000000000000011546 ) ) ;
#30150 = CARTESIAN_POINT ( 'NONE',  ( 71.70339147920792300, 60.88422586754655441, -3.784404822148339953 ) ) ;
#30151 = ORIENTED_EDGE ( 'NONE', *, *, #2457, .F. ) ;
#30152 = CARTESIAN_POINT ( 'NONE',  ( 86.92455237868826146, -1.249784692553891574, -5.093375875629621241 ) ) ;
#30153 = CARTESIAN_POINT ( 'NONE',  ( 3.057746519440326605, -26.45262624289676978, 6.969307238440508812 ) ) ;
#30154 = DIRECTION ( 'NONE',  ( -0.000000000000000000, -1.000000000000000000, -0.000000000000000000 ) ) ;
#30155 = ADVANCED_FACE ( 'NONE', ( #8562 ), #33709, .F. ) ;
#30156 = CARTESIAN_POINT ( 'NONE',  ( 2.193021027211013330, -32.93406463935832562, 7.774064877406527962 ) ) ;
#30157 = ORIENTED_EDGE ( 'NONE', *, *, #30928, .F. ) ;
#30158 = LINE ( 'NONE', #4643, #21311 ) ;
#30159 = DIRECTION ( 'NONE',  ( -0.9848077530122067991, -0.1736481776669374644, -0.000000000000000000 ) ) ;
#30160 = EDGE_LOOP ( 'NONE', ( #32820, #29055, #20876, #19774 ) ) ;
#30161 = CARTESIAN_POINT ( 'NONE',  ( 79.22323586724851907, 64.66701280635210480, -3.467090974304450235 ) ) ;
#30162 = CARTESIAN_POINT ( 'NONE',  ( 16.61473287052537273, 9.888383995183708919, -2.499999999999976019 ) ) ;
#30163 = CARTESIAN_POINT ( 'NONE',  ( 78.83700374940842437, 65.31049604782704421, 2.918211652848220261 ) ) ;
#30164 = CARTESIAN_POINT ( 'NONE',  ( -0.1589752317941719728, -32.41646502212034875, 7.013842709614101167 ) ) ;
#30165 = EDGE_CURVE ( 'NONE', #21217, #22430, #15779, .T. ) ;
#30166 = CARTESIAN_POINT ( 'NONE',  ( 22.63566524836003069, 3.890655838760145979, 3.739241026276091340 ) ) ;
#30167 = CARTESIAN_POINT ( 'NONE',  ( -72.42837670882107659, -47.11702805680359063, 5.809475019311127753 ) ) ;
#30168 = CARTESIAN_POINT ( 'NONE',  ( 18.53067622772632461, 13.20527538885293062, 2.499999999999999556 ) ) ;
#30169 = CARTESIAN_POINT ( 'NONE',  ( 21.85643539959774984, 9.043776176932434296, -7.298091200098202336 ) ) ;
#30170 = ORIENTED_EDGE ( 'NONE', *, *, #12314, .F. ) ;
#30171 = CARTESIAN_POINT ( 'NONE',  ( -80.19809822935498289, 11.50978792661036998, 3.773274132804689263 ) ) ;
#30172 = CARTESIAN_POINT ( 'NONE',  ( 14.74178471286434622, -5.124043802339638631, 2.500000000000000444 ) ) ;
#30173 = CARTESIAN_POINT ( 'NONE',  ( -73.70430257933739426, 6.071219537989406057, -10.84014157372769382 ) ) ;
#30174 = EDGE_CURVE ( 'NONE', #15627, #8458, #12889, .T. ) ;
#30175 = CARTESIAN_POINT ( 'NONE',  ( 1.500917888593657379, -32.96407850412315810, 6.911401339314955372 ) ) ;
#30176 = CARTESIAN_POINT ( 'NONE',  ( 2.382407531972861037, -26.23902213697312291, 6.866852738645442322 ) ) ;
#30177 = CARTESIAN_POINT ( 'NONE',  ( 80.77164629763791481, 63.73694215246327133, 3.562450064734656419 ) ) ;
#30178 = CARTESIAN_POINT ( 'NONE',  ( 3.539909946428774656, -24.83646909262585112, 7.013842709614101167 ) ) ;
#30179 = DIRECTION ( 'NONE',  ( 0.000000000000000000, 0.000000000000000000, 1.000000000000000000 ) ) ;
#30180 = FACE_OUTER_BOUND ( 'NONE', #26964, .T. ) ;
#30181 = CARTESIAN_POINT ( 'NONE',  ( 0.6853293712966370688, -26.22035530670912351, 6.941203072598474577 ) ) ;
#30182 = CARTESIAN_POINT ( 'NONE',  ( 4.498621949403786680, -27.46757472365032982, 6.980586498568972509 ) ) ;
#30183 = CARTESIAN_POINT ( 'NONE',  ( -30.87867591359218977, -26.64985754041175525, 6.700000000000000178 ) ) ;
#30184 = CARTESIAN_POINT ( 'NONE',  ( 5.172564876073734830, -29.12947328719863194, 7.013842709614101167 ) ) ;
#30185 = ORIENTED_EDGE ( 'NONE', *, *, #25169, .T. ) ;
#30186 = CARTESIAN_POINT ( 'NONE',  ( 68.04343099365841852, 58.34291608657256489, 3.996230182412897403 ) ) ;
#30187 = CARTESIAN_POINT ( 'NONE',  ( 37.04435200418730290, -2.893112835670054395, 5.988065069928986794 ) ) ;
#30188 = VECTOR ( 'NONE', #28467, 1000.000000000000000 ) ;
#30189 = EDGE_CURVE ( 'NONE', #6925, #19965, #13453, .T. ) ;
#30190 = EDGE_LOOP ( 'NONE', ( #12521, #13972, #19729, #34678, #30739 ) ) ;
#30191 = CARTESIAN_POINT ( 'NONE',  ( 2.325325312725053717, -33.01368626817038887, 7.750000000000001776 ) ) ;
#30192 = CARTESIAN_POINT ( 'NONE',  ( 88.43294427370824451, -0.9743556922601576131, -2.623293804462837553 ) ) ;
#30194 = CARTESIAN_POINT ( 'NONE',  ( 33.64208751344185089, -1.232828649894890605, -5.457059412070498716 ) ) ;
#30193 = CARTESIAN_POINT ( 'NONE',  ( 33.80908501075300165, -4.930824710404003497, 3.361253013157701197 ) ) ;
#30195 = CARTESIAN_POINT ( 'NONE',  ( -1.617528036734913188, -28.82728981784584477, 6.871394612369936539 ) ) ;
#30196 = CARTESIAN_POINT ( 'NONE',  ( -58.20517375958247186, 28.49598760833110944, 5.016376253474285285 ) ) ;
#30197 = DIRECTION ( 'NONE',  ( 1.000000000000000000, 0.000000000000000000, 0.000000000000000000 ) ) ;
#30198 = ORIENTED_EDGE ( 'NONE', *, *, #9159, .T. ) ;
#30199 = CARTESIAN_POINT ( 'NONE',  ( -71.71319929822489314, -21.40271194095481633, 5.960493810635115963 ) ) ;
#30200 = VERTEX_POINT ( 'NONE', #3858 ) ;
#30201 = AXIS2_PLACEMENT_3D ( 'NONE', #6933, #22396, #10419 ) ;
#30202 = ORIENTED_EDGE ( 'NONE', *, *, #13623, .F. ) ;
#30203 = CARTESIAN_POINT ( 'NONE',  ( 80.83598165300548999, 61.89502789394175863, -2.843122152733553065 ) ) ;
#30204 = EDGE_CURVE ( 'NONE', #38080, #18928, #20212, .T. ) ;
#30205 = PLANE ( 'NONE',  #23375 ) ;
#30206 = ADVANCED_FACE ( 'NONE', ( #36681 ), #21047, .T. ) ;
#30207 = CARTESIAN_POINT ( 'NONE',  ( 78.83217078968489488, 65.79276158749709680, 2.259810845156947412 ) ) ;
#30208 = CARTESIAN_POINT ( 'NONE',  ( 23.17509331881612056, 0.5418487631251007741, 5.782618900065904732 ) ) ;
#30210 = ORIENTED_EDGE ( 'NONE', *, *, #18399, .F. ) ;
#30209 = CARTESIAN_POINT ( 'NONE',  ( -0.7646816970285992277, -27.22825800806822016, 6.939395833800444002 ) ) ;
#30211 = ADVANCED_FACE ( 'NONE', ( #27813 ), #34645, .F. ) ;
#30212 = CYLINDRICAL_SURFACE ( 'NONE', #1216, 0.1000000000000028644 ) ;
#30213 = CARTESIAN_POINT ( 'NONE',  ( 73.50720661118039345, 61.38260725348155944, -3.841642204035220942 ) ) ;
#30214 = CARTESIAN_POINT ( 'NONE',  ( -63.99293516169446150, 35.89893413629672381, -12.49999999999999645 ) ) ;
#30216 = DIRECTION ( 'NONE',  ( 0.000000000000000000, 0.000000000000000000, -1.000000000000000000 ) ) ;
#30215 = CARTESIAN_POINT ( 'NONE',  ( 14.69558838330753758, 3.996311804371543985, -6.000000000000000000 ) ) ;
#30217 = CARTESIAN_POINT ( 'NONE',  ( -1.233777691191984216, -27.85215430352675980, 7.779495906702012853 ) ) ;
#30218 = DIRECTION ( 'NONE',  ( -0.000000000000000000, -0.000000000000000000, 1.000000000000000000 ) ) ;
#30219 = PLANE ( 'NONE',  #25198 ) ;
#30220 = CARTESIAN_POINT ( 'NONE',  ( 22.92659693992655079, 4.107476889741620951, -3.299805457877865056 ) ) ;
#30221 = ORIENTED_EDGE ( 'NONE', *, *, #38521, .F. ) ;
#30222 = CYLINDRICAL_SURFACE ( 'NONE', #40619, 2.000000000000000000 ) ;
#30223 = ORIENTED_EDGE ( 'NONE', *, *, #17431, .T. ) ;
#30224 = AXIS2_PLACEMENT_3D ( 'NONE', #39081, #13974, #33548 ) ;
#30225 = CARTESIAN_POINT ( 'NONE',  ( 22.32844273176644379, 5.552903595841022444, -4.279453667248723114 ) ) ;
#30226 = CARTESIAN_POINT ( 'NONE',  ( -0.9579939928752762013, -31.84654925493761368, 7.710604733652627552 ) ) ;
#30227 = EDGE_CURVE ( 'NONE', #18554, #10884, #28624, .T. ) ;
#30228 = VERTEX_POINT ( 'NONE', #22481 ) ;
#30229 = CARTESIAN_POINT ( 'NONE',  ( 1.109803157764845061, -33.01974279738480789, 7.750000000000000888 ) ) ;
#30230 = CARTESIAN_POINT ( 'NONE',  ( 80.71310200136858271, 64.86488640220490254, 3.283621700565936052 ) ) ;
#30231 = CARTESIAN_POINT ( 'NONE',  ( 86.57035376367728929, -0.007661497531101129840, -5.962853773335548446 ) ) ;
#30232 = FACE_OUTER_BOUND ( 'NONE', #40190, .T. ) ;
#30233 = VERTEX_POINT ( 'NONE', #19584 ) ;
#30234 = DIRECTION ( 'NONE',  ( -0.4999999999999918954, -0.8660254037844432595, -0.000000000000000000 ) ) ;
#30235 = CARTESIAN_POINT ( 'NONE',  ( 5.066705152069533646, -29.09251744304078002, 6.864276522220859711 ) ) ;
#30236 = AXIS2_PLACEMENT_3D ( 'NONE', #11833, #24204, #12255 ) ;
#30237 = CARTESIAN_POINT ( 'NONE',  ( 16.05059429624258271, -3.466255778341811755, -2.706403111257027039 ) ) ;
#30238 = CARTESIAN_POINT ( 'NONE',  ( 33.68724495179844070, -3.100361039176545486, -5.464107322465908467 ) ) ;
#30239 = DIRECTION ( 'NONE',  ( 0.7394003126383927871, -0.1303762246624153853, -0.6605219282605403475 ) ) ;
#30240 = CARTESIAN_POINT ( 'NONE',  ( 24.69561352525090214, 0.6721404258068209847, -4.790969045266487036 ) ) ;
#30241 = CARTESIAN_POINT ( 'NONE',  ( 29.95669672263519701, -3.739584766489346013, -4.529080000040674570 ) ) ;
#30242 = ORIENTED_EDGE ( 'NONE', *, *, #38245, .F. ) ;
#30243 = CARTESIAN_POINT ( 'NONE',  ( 22.91740499742190096, 2.643278788709220617, 3.783213328018341759 ) ) ;
#30244 = ADVANCED_FACE ( 'NONE', ( #19782 ), #13390, .F. ) ;
#30245 = CARTESIAN_POINT ( 'NONE',  ( 32.03825560683729634, -2.979144026594910066, -5.206742654223620370 ) ) ;
#30246 = VERTEX_POINT ( 'NONE', #10498 ) ;
#30247 = EDGE_LOOP ( 'NONE', ( #8663, #15430 ) ) ;
#30248 = CARTESIAN_POINT ( 'NONE',  ( 34.63832540556266792, -0.7796590688174727113, 5.272668787675296009 ) ) ;
#30249 = CARTESIAN_POINT ( 'NONE',  ( -1.078675913592196167, -26.64985754041175525, 6.800000000000000711 ) ) ;
#30250 = CARTESIAN_POINT ( 'NONE',  ( 14.61802081865033642, 12.33286846116284252, -2.500000000000000000 ) ) ;
#30251 = CARTESIAN_POINT ( 'NONE',  ( 0.000000000000000000, -30.38627270959228710, 0.000000000000000000 ) ) ;
#30252 = EDGE_LOOP ( 'NONE', ( #3935, #31074, #980, #17439, #31782 ) ) ;
#30253 = DIRECTION ( 'NONE',  ( -0.000000000000000000, 0.000000000000000000, -1.000000000000000000 ) ) ;
#30254 = EDGE_LOOP ( 'NONE', ( #5423, #27788, #26321, #796 ) ) ;
#30255 = ADVANCED_FACE ( 'NONE', ( #26371 ), #13731, .F. ) ;
#30256 = EDGE_LOOP ( 'NONE', ( #36586, #25475 ) ) ;
#30257 = LINE ( 'NONE', #12893, #12802 ) ;
#30258 = CARTESIAN_POINT ( 'NONE',  ( 79.34351131543186852, 65.42632830064326299, -2.956864960647760832 ) ) ;
#30259 = CARTESIAN_POINT ( 'NONE',  ( -57.86591918990971806, 28.88504657882484494, -4.653542815086523454 ) ) ;
#30260 = ORIENTED_EDGE ( 'NONE', *, *, #15774, .T. ) ;
#30261 = CARTESIAN_POINT ( 'NONE',  ( 4.750267137322237154, -27.85286966892973126, 6.887161170156907097 ) ) ;
#30262 = ORIENTED_EDGE ( 'NONE', *, *, #14631, .T. ) ;
#30263 = CARTESIAN_POINT ( 'NONE',  ( 22.71203523026179028, 4.249011684457585147, 3.358792741310332008 ) ) ;
#30264 = EDGE_CURVE ( 'NONE', #21904, #34419, #39385, .T. ) ;
#30265 = CARTESIAN_POINT ( 'NONE',  ( 81.85640814870936310, 64.68575429476366878, -2.512558077908312537 ) ) ;
#30266 = DIRECTION ( 'NONE',  ( 0.1736481776669404897, -0.9848077530122062440, -0.000000000000000000 ) ) ;
#30267 = AXIS2_PLACEMENT_3D ( 'NONE', #19620, #29088, #35878 ) ;
#30268 = DIRECTION ( 'NONE',  ( 0.6427876096865481337, -0.7660444431189707970, -0.000000000000000000 ) ) ;
#30269 = EDGE_LOOP ( 'NONE', ( #3303, #13722, #10070, #18453 ) ) ;
#30271 = LINE ( 'NONE', #11511, #25575 ) ;
#30270 = CARTESIAN_POINT ( 'NONE',  ( -0.03065438358791858567, -26.64358689880297248, 7.703977250142846955 ) ) ;
#30272 = FACE_OUTER_BOUND ( 'NONE', #18290, .T. ) ;
#30273 = CARTESIAN_POINT ( 'NONE',  ( 76.19819836466999163, 59.97076997751576499, 3.322260703561256800 ) ) ;
#30274 = CARTESIAN_POINT ( 'NONE',  ( 22.49685282670636255, 2.447218780948473782, -4.963950670329193571 ) ) ;
#30275 = DIRECTION ( 'NONE',  ( -0.000000000000000000, -1.000000000000000000, -0.000000000000000000 ) ) ;
#30276 = CARTESIAN_POINT ( 'NONE',  ( -12.99139449055068241, 13.37661300689600097, 2.500000000000000000 ) ) ;
#30277 = CARTESIAN_POINT ( 'NONE',  ( -1.254132200242210837, -27.88741944239102466, 7.643333865083953071 ) ) ;
#30278 = CARTESIAN_POINT ( 'NONE',  ( 3.549114750742319746, -32.43177086262681996, 7.139196562012271485 ) ) ;
#30279 = CARTESIAN_POINT ( 'NONE',  ( 80.45692750329155274, 65.79057296784172593, 2.573500632437474511 ) ) ;
#30280 = CARTESIAN_POINT ( 'NONE',  ( 88.23268491810016201, -0.7494148791586221492, 1.919551801057179263 ) ) ;
#30281 = CARTESIAN_POINT ( 'NONE',  ( 33.90241230359465874, -5.503808810968542353, 0.4955917775451662566 ) ) ;
#30282 = CIRCLE ( 'NONE', #38184, 0.1000000000000028644 ) ;
#30283 = CARTESIAN_POINT ( 'NONE',  ( 2.827544659576278985, -32.88348186366498282, 6.867280401193707640 ) ) ;
#30284 = CARTESIAN_POINT ( 'NONE',  ( 18.28173501743642859, -3.120125090614966012, 3.013464740560008348 ) ) ;
#30285 = FACE_OUTER_BOUND ( 'NONE', #8827, .T. ) ;
#30286 = CARTESIAN_POINT ( 'NONE',  ( 34.12754808946520058, -3.289252972442476164, -5.532827275885577656 ) ) ;
#30287 = DIRECTION ( 'NONE',  ( 0.000000000000000000, 1.000000000000000000, 0.000000000000000000 ) ) ;
#30288 = DIRECTION ( 'NONE',  ( -0.000000000000000000, -1.000000000000000000, -0.000000000000000000 ) ) ;
#30289 =( BOUNDED_CURVE ( )  B_SPLINE_CURVE ( 3, ( #19625, #3798, #19822, #500 ),
 .UNSPECIFIED., .F., .T. ) 
 B_SPLINE_CURVE_WITH_KNOTS ( ( 4, 4 ),
 ( 4.748221474220558846, 4.941946782021393147 ),
 .UNSPECIFIED. ) 
 CURVE ( )  GEOMETRIC_REPRESENTATION_ITEM ( )  RATIONAL_B_SPLINE_CURVE ( ( 1.000000000000000000, 0.9968749865767494445, 0.9968749865767494445, 1.000000000000000000 ) ) 
 REPRESENTATION_ITEM ( '' )  );
#30290 = PRODUCT ( 'MAS-318', 'MAS-318', '', ( #22980 ) ) ;
#30291 = DIRECTION ( 'NONE',  ( 1.000000000000000000, 0.000000000000000000, 0.000000000000000000 ) ) ;
#30292 = CARTESIAN_POINT ( 'NONE',  ( 0.06066625181903905623, -26.47779407321028700, 7.750000000000000888 ) ) ;
#30293 = EDGE_CURVE ( 'NONE', #14785, #7585, #30068, .T. ) ;
#30294 = CARTESIAN_POINT ( 'NONE',  ( -69.62739392171840791, -46.36406956038555194, 5.857517722768268875 ) ) ;
#30295 = AXIS2_PLACEMENT_3D ( 'NONE', #39088, #10885, #3946 ) ;
#30296 = ORIENTED_EDGE ( 'NONE', *, *, #4514, .T. ) ;
#30297 = CARTESIAN_POINT ( 'NONE',  ( 37.15955769875629500, -2.950428308811992029, 5.999626784867526652 ) ) ;
#30298 = CARTESIAN_POINT ( 'NONE',  ( -70.14355411941724583, -0.1632709328201389365, 3.948449672239096486 ) ) ;
#30299 = CARTESIAN_POINT ( 'NONE',  ( 66.72638704319571445, 57.85960203741856134, -3.999543855871245945 ) ) ;
#30300 = ADVANCED_FACE ( 'NONE', ( #1194 ), #3681, .F. ) ;
#30301 = CARTESIAN_POINT ( 'NONE',  ( -71.19065411851930492, 0.1907566484747143243, 9.997285688091771760 ) ) ;
#30302 = DIRECTION ( 'NONE',  ( 0.000000000000000000, -0.000000000000000000, -1.000000000000000000 ) ) ;
#30303 = EDGE_LOOP ( 'NONE', ( #3257, #34199, #37266, #35094 ) ) ;
#30304 = DIRECTION ( 'NONE',  ( 1.000000000000000000, 0.000000000000000000, 0.000000000000000000 ) ) ;
#30305 = EDGE_CURVE ( 'NONE', #16957, #12163, #10620, .T. ) ;
#30306 = CARTESIAN_POINT ( 'NONE',  ( 3.809088224730495131, -32.23704061701660351, 7.774064877406527074 ) ) ;
#30307 = CARTESIAN_POINT ( 'NONE',  ( 14.77222812468937363, 12.33286846116137347, 2.511961485181785747 ) ) ;
#30308 = CARTESIAN_POINT ( 'NONE',  ( -80.31292318400757324, 11.50538633170450176, 3.479145684545672523 ) ) ;
#30309 = DIRECTION ( 'NONE',  ( -0.000000000000000000, -0.000000000000000000, -1.000000000000000000 ) ) ;
#30310 = PLANE ( 'NONE',  #33721 ) ;
#30311 = ORIENTED_EDGE ( 'NONE', *, *, #15484, .T. ) ;
#30312 = CARTESIAN_POINT ( 'NONE',  ( 22.18671130633063271, 5.268486589209644855, 3.076124624071696623 ) ) ;
#30313 = CIRCLE ( 'NONE', #28348, 5.329987104167474676 ) ;
#30314 = ADVANCED_FACE ( 'NONE', ( #16205 ), #3887, .T. ) ;
#30315 = CARTESIAN_POINT ( 'NONE',  ( 81.47320529907102582, 61.46857867680781595, -1.048259027381222008 ) ) ;
#30316 = CARTESIAN_POINT ( 'NONE',  ( -71.92837670882107659, -0.7829914368874776320, 3.916079783099624567 ) ) ;
#30317 = CARTESIAN_POINT ( 'NONE',  ( 81.21586879471321652, 61.61940358760092806, 2.137206601789639393 ) ) ;
#30318 = EDGE_CURVE ( 'NONE', #2808, #4035, #29404, .T. ) ;
#30319 = CARTESIAN_POINT ( 'NONE',  ( 7.121324086407810228, -26.64985754041175525, 6.700000000000000178 ) ) ;
#30320 = ORIENTED_EDGE ( 'NONE', *, *, #24370, .T. ) ;
#30321 = CARTESIAN_POINT ( 'NONE',  ( 77.32551012344487162, 64.79183443757983696, -2.725046208697011529 ) ) ;
#30322 = CIRCLE ( 'NONE', #37538, 3.499999999999999556 ) ;
#30324 = CARTESIAN_POINT ( 'NONE',  ( 14.66195011488853517, -4.891470949017669767, -2.500000000000007550 ) ) ;
#30323 = CARTESIAN_POINT ( 'NONE',  ( 24.74514331060581185, 0.5825920455569916223, 4.777508842034277059 ) ) ;
#30325 = CARTESIAN_POINT ( 'NONE',  ( 81.01997673013535461, 63.86331202395377460, -3.456914256419913567 ) ) ;
#30326 = CARTESIAN_POINT ( 'NONE',  ( 79.57145864546818359, 62.55878779196851269, 3.641957811749160001 ) ) ;
#30327 = VERTEX_POINT ( 'NONE', #22604 ) ;
#30328 = VERTEX_POINT ( 'NONE', #7340 ) ;
#30329 = B_SPLINE_CURVE_WITH_KNOTS ( 'NONE', 3,
 ( #28142, #3072, #40696, #18049, #12074, #21985, #34561, #30641, #6331, #25273, #2449, #24651, #8992, #18882, #31452, #19289, #38213, #32270, #7135, #28560, #19086, #10010, #31656 ),
 .UNSPECIFIED., .F., .F.,
 ( 4, 2, 2, 2, 1, 2, 2, 1, 2, 2, 1, 2, 4 ),
 ( 0.000000000000000000, 0.1556967518389709704, 0.2335451277584564278, 0.2530072217383279587, 0.2724693157181994896, 0.3113935036779426069, 0.4670902555169128001, 0.4865523494967844975, 0.4962833964867204295, 0.5011489199816884232, 0.5060144434766563615, 0.5449386314364057515, 0.6227870073559045316 ),
 .UNSPECIFIED. ) ;
#30330 = CARTESIAN_POINT ( 'NONE',  ( -0.9271279775035500270, -27.41211907304282036, 7.703977250142846067 ) ) ;
#30331 = AXIS2_PLACEMENT_3D ( 'NONE', #38477, #10676, #35429 ) ;
#30332 = CARTESIAN_POINT ( 'NONE',  ( 79.65107971589632996, 66.31509156740921185, 1.306649493516908400 ) ) ;
#30334 = CARTESIAN_POINT ( 'NONE',  ( 14.69558838330753758, 3.996311804371543985, -6.000000000000000000 ) ) ;
#30333 = CARTESIAN_POINT ( 'NONE',  ( 4.945445480008764605, -30.88065529806472043, 7.754798119455333705 ) ) ;
#30335 = CARTESIAN_POINT ( 'NONE',  ( 28.43092716748534343, -1.248584762127236569, 6.041969456467763955 ) ) ;
#30336 = CARTESIAN_POINT ( 'NONE',  ( -18.87867591359219333, -24.55319635012989110, 6.700000000000000178 ) ) ;
#30337 = CARTESIAN_POINT ( 'NONE',  ( -1.267760583032661037, -27.71561997405539302, 7.754798119455333705 ) ) ;
#30338 = EDGE_LOOP ( 'NONE', ( #19046, #16710, #30101, #8728 ) ) ;
#30339 = CARTESIAN_POINT ( 'NONE',  ( 1.645206451479275911, -33.06949512287985016, 6.875671892026061549 ) ) ;
#30340 = CARTESIAN_POINT ( 'NONE',  ( 22.61176954047653709, 0.2940635019282091256, -6.499681003685747527 ) ) ;
#30341 = DIRECTION ( 'NONE',  ( 0.9396926207859082059, 0.3420201433256695456, -0.000000000000000000 ) ) ;
#30342 = VERTEX_POINT ( 'NONE', #23395 ) ;
#30343 = LINE ( 'NONE', #2149, #38195 ) ;
#30344 = CARTESIAN_POINT ( 'NONE',  ( -0.7517451142625637406, -27.06299922110170542, 7.501983001166816933 ) ) ;
#30345 = CARTESIAN_POINT ( 'NONE',  ( 5.174173811910133480, -29.14233078835555091, 6.912143950357348743 ) ) ;
#30346 = CARTESIAN_POINT ( 'NONE',  ( -72.23853693793628850, -47.87307048379776120, 9.914091297619886944 ) ) ;
#30347 = CARTESIAN_POINT ( 'NONE',  ( 37.10367516289256429, -3.125626235160924526, -5.976315389033000081 ) ) ;
#30348 = CARTESIAN_POINT ( 'NONE',  ( 3.369184120440228636, -26.60764618298541251, 7.692469944509203295 ) ) ;
#30349 = CARTESIAN_POINT ( 'NONE',  ( 1.700390093233090871, -29.56993018339339940, 6.800000000000000711 ) ) ;
#30350 = CARTESIAN_POINT ( 'NONE',  ( 5.166866161692755810, -29.08666662507720702, 7.750000000000000888 ) ) ;
#30351 = CARTESIAN_POINT ( 'NONE',  ( 4.999353408448902414, -30.73905325571789149, 7.660770905198780234 ) ) ;
#30352 = CARTESIAN_POINT ( 'NONE',  ( -18.87867591359219333, -24.55319635012989110, 6.800000000000000711 ) ) ;
#30353 = CARTESIAN_POINT ( 'NONE',  ( -18.24874870218063450, -26.64985754041175525, 6.700000000000000178 ) ) ;
#30354 = CARTESIAN_POINT ( 'NONE',  ( 4.921995751488993598, -28.48303424522928040, 7.782034975670475418 ) ) ;
#30355 = CARTESIAN_POINT ( 'NONE',  ( 2.835597840154314042, -26.36504276394633806, 7.661510568013100375 ) ) ;
#30356 = CARTESIAN_POINT ( 'NONE',  ( 24.14678853894412214, 1.668812993869833283, -4.589722933970846519 ) ) ;
#30357 = ORIENTED_EDGE ( 'NONE', *, *, #16861, .T. ) ;
#30358 = CARTESIAN_POINT ( 'NONE',  ( -70.00483706461088218, -48.31492315352122802, 5.930144077445180351 ) ) ;
#30359 = CARTESIAN_POINT ( 'NONE',  ( 66.27376694608996388, 57.73522568913447373, 4.000000000000000000 ) ) ;
#30360 = CARTESIAN_POINT ( 'NONE',  ( 69.15563817390996348, 58.92225492517195562, -3.988427515945576207 ) ) ;
#30361 = ORIENTED_EDGE ( 'NONE', *, *, #1296, .F. ) ;
#30362 = DIRECTION ( 'NONE',  ( -1.000000000000000000, 0.000000000000000000, 0.000000000000000000 ) ) ;
#30363 = VECTOR ( 'NONE', #19340, 1000.000000000000000 ) ;
#30364 = DIRECTION ( 'NONE',  ( 0.3420201433256578882, 0.9396926207859123137, 0.000000000000000000 ) ) ;
#30365 = DIRECTION ( 'NONE',  ( 0.000000000000000000, 1.000000000000000000, 0.000000000000000000 ) ) ;
#30366 = CARTESIAN_POINT ( 'NONE',  ( -1.416913847263542081, -28.21257375718617055, 6.969307238440506147 ) ) ;
#30367 = CARTESIAN_POINT ( 'NONE',  ( -0.9119913687292857674, -27.24064530155898112, 6.863784140767622333 ) ) ;
#30368 = CARTESIAN_POINT ( 'NONE',  ( -1.798306572096198153, -29.57636892467929712, 7.762460296495606649 ) ) ;
#30369 = EDGE_LOOP ( 'NONE', ( #14357, #1658, #22677, #30481 ) ) ;
#30370 = CARTESIAN_POINT ( 'NONE',  ( 1.700390093233090871, -29.56993018339339940, 7.750000000000000888 ) ) ;
#30371 = EDGE_CURVE ( 'NONE', #16587, #17641, #17280, .T. ) ;
#30372 = DIRECTION ( 'NONE',  ( 0.000000000000000000, 0.000000000000000000, -1.000000000000000000 ) ) ;
#30373 = CARTESIAN_POINT ( 'NONE',  ( 22.38977015051906250, -3.087247959475952541, 3.600891321702764269 ) ) ;
#30374 = ADVANCED_FACE ( 'NONE', ( #32472 ), #32082, .F. ) ;
#30375 = VERTEX_POINT ( 'NONE', #10223 ) ;
#30376 = CARTESIAN_POINT ( 'NONE',  ( 78.50817655541952433, 65.71198414996337078, -2.174061886842029168 ) ) ;
#30377 = CARTESIAN_POINT ( 'NONE',  ( -30.87867591359218977, -26.64985754041175525, 6.700000000000000178 ) ) ;
#30378 = CARTESIAN_POINT ( 'NONE',  ( 79.89307030929698783, 66.05340108613441430, -2.264354540981541764 ) ) ;
#30379 = CARTESIAN_POINT ( 'NONE',  ( 78.44852601586514140, 65.88695166727248420, 1.521414672925275546 ) ) ;
#30380 = CARTESIAN_POINT ( 'NONE',  ( 0.3856705772283747780, -32.81361829944838604, 7.750000000000000888 ) ) ;
#30381 = B_SPLINE_CURVE_WITH_KNOTS ( 'NONE', 3,
 ( #2518, #15042, #21230, #24306, #5580, #30916, #40157, #39542, #15245, #11731, #39959, #33186, #33405, #33800, #2104, #5178, #27603, #40352, #24516 ),
 .UNSPECIFIED., .F., .F.,
 ( 4, 3, 3, 3, 3, 3, 4 ),
 ( 2.475319317933456060E-05, 2.546128104244956540E-05, 5.711050680483690107E-05, 8.113074941674912051E-05, 0.0001053129305726947589, 0.0001360598016346936364, 0.0001612931755702001855 ),
 .UNSPECIFIED. ) ;
#30382 = CARTESIAN_POINT ( 'NONE',  ( 4.030693118979438161, -27.09410047637255303, 7.006423389747789443 ) ) ;
#30383 = CARTESIAN_POINT ( 'NONE',  ( 17.44014759849567398, 14.20845974933103051, 2.500000000000000444 ) ) ;
#30384 = CARTESIAN_POINT ( 'NONE',  ( 21.85643539959773207, -2.491245572580281564, -14.29094192267194607 ) ) ;
#30385 = ORIENTED_EDGE ( 'NONE', *, *, #29961, .F. ) ;
#30386 = CARTESIAN_POINT ( 'NONE',  ( -80.70858810156305196, 11.48226577419836225, 2.235992612072733365 ) ) ;
#30387 = CARTESIAN_POINT ( 'NONE',  ( 14.74659717070468723, -5.121692793854265346, 2.499999999975831333 ) ) ;
#30388 = CARTESIAN_POINT ( 'NONE',  ( -74.02042637766889754, 8.682579473379398394, -9.514814749544530770 ) ) ;
#30389 = CARTESIAN_POINT ( 'NONE',  ( 1.506564090326510508, -32.96440090511088528, 6.903372536218457256 ) ) ;
#30390 = CARTESIAN_POINT ( 'NONE',  ( 35.36840502023477484, -3.795127586234050110, -5.508707976554834573 ) ) ;
#30391 = DIRECTION ( 'NONE',  ( -1.000000000000000000, 0.000000000000000000, 0.000000000000000000 ) ) ;
#30392 = CARTESIAN_POINT ( 'NONE',  ( 14.82426946740453921, 12.80491062889915099, 2.505159076423423503 ) ) ;
#30393 = CARTESIAN_POINT ( 'NONE',  ( -0.5769924795711234289, -32.09451502393404354, 7.754798119455333705 ) ) ;
#30394 = CARTESIAN_POINT ( 'NONE',  ( -69.95448302925287010, -0.5208875146770525211, 9.952591258774150518 ) ) ;
#30395 = LINE ( 'NONE', #2621, #36816 ) ;
#30396 = AXIS2_PLACEMENT_3D ( 'NONE', #31733, #36424, #17459 ) ;
#30397 = CARTESIAN_POINT ( 'NONE',  ( -64.71577923686258771, 34.74117003693350370, 6.230828392942166616 ) ) ;
#30398 = DIRECTION ( 'NONE',  ( 0.000000000000000000, 1.000000000000000000, 0.000000000000000000 ) ) ;
#30399 = CARTESIAN_POINT ( 'NONE',  ( -11.81496944966682960, -21.25669541281728669, -4.000000000000000000 ) ) ;
#30400 = VERTEX_POINT ( 'NONE', #22806 ) ;
#30401 = CARTESIAN_POINT ( 'NONE',  ( 68.80725167329416081, 58.08536582812667604, 3.941639393089866328 ) ) ;
#30402 = CARTESIAN_POINT ( 'NONE',  ( 25.29913702416237342, 1.743601996224051431, 4.154940213198440091 ) ) ;
#30403 = CARTESIAN_POINT ( 'NONE',  ( 84.57067941792149668, 3.126724152278200997, 0.3173792860121260051 ) ) ;
#30404 = CARTESIAN_POINT ( 'NONE',  ( 1.011962798722023882, -33.78603799583471101, 7.695279973900954751 ) ) ;
#30405 = CARTESIAN_POINT ( 'NONE',  ( -1.636164459686335615, -28.91612145343104245, 6.880147297696979969 ) ) ;
#30406 = LINE ( 'NONE', #11853, #31179 ) ;
#30407 = CARTESIAN_POINT ( 'NONE',  ( -69.92837670882106238, -20.91541721511087815, 5.916079783099611689 ) ) ;
#30408 = ORIENTED_EDGE ( 'NONE', *, *, #1279, .F. ) ;
#30409 = CARTESIAN_POINT ( 'NONE',  ( -71.04476776058896803, -21.78243674987466605, 6.011900603202944282 ) ) ;
#30410 = UNCERTAINTY_MEASURE_WITH_UNIT (LENGTH_MEASURE( 1.000000000000000082E-05 ), #21229, 'distance_accuracy_value', 'NONE');
#30411 = ORIENTED_EDGE ( 'NONE', *, *, #6055, .F. ) ;
#30412 = ADVANCED_FACE ( 'NONE', ( #32280 ), #16594, .T. ) ;
#30413 = VERTEX_POINT ( 'NONE', #33072 ) ;
#30414 = CARTESIAN_POINT ( 'NONE',  ( 79.28293246176357911, 65.06528690105534452, -3.252077313700849182 ) ) ;
#30415 = CARTESIAN_POINT ( 'NONE',  ( -1.526829923184012339, -28.21528965334980654, 7.013842709614101167 ) ) ;
#30416 = CARTESIAN_POINT ( 'NONE',  ( 80.10672643282893546, 63.77302114994544269, 3.692178340560209993 ) ) ;
#30417 = CARTESIAN_POINT ( 'NONE',  ( 23.10229947436055298, 0.3735801593563349843, 5.909219875391088728 ) ) ;
#30420 = ORIENTED_EDGE ( 'NONE', *, *, #30318, .F. ) ;
#30419 = CARTESIAN_POINT ( 'NONE',  ( 4.722721840544713778, -27.80484921947353527, 7.750000000000000888 ) ) ;
#30418 = VECTOR ( 'NONE', #20829, 1000.000000000000000 ) ;
#30421 = CARTESIAN_POINT ( 'NONE',  ( 74.33180802611956040, 62.54477577240981390, -3.494507759124076962 ) ) ;
#30422 = DIRECTION ( 'NONE',  ( -0.000000000000000000, -0.000000000000000000, 1.000000000000000000 ) ) ;
#30423 = B_SPLINE_CURVE_WITH_KNOTS ( 'NONE', 3,
 ( #10848, #11240, #39451, #23805 ),
 .UNSPECIFIED., .F., .F.,
 ( 4, 4 ),
 ( 0.000000000000000000, 6.391136169901225176E-06 ),
 .UNSPECIFIED. ) ;
#30425 = PLANE ( 'NONE',  #7174 ) ;
#30424 = CARTESIAN_POINT ( 'NONE',  ( 0.01871827436868165120, 0.5999999999999996447, -3.829290154341121966 ) ) ;
#30426 = LINE ( 'NONE', #14975, #21158 ) ;
#30427 = CARTESIAN_POINT ( 'NONE',  ( -1.597957901506573020, -30.69845554356182049, 7.784725160561909441 ) ) ;
#30428 = CARTESIAN_POINT ( 'NONE',  ( 22.89526542370903073, 4.247657506257562332, -3.165813468130866948 ) ) ;
#30429 = ORIENTED_EDGE ( 'NONE', *, *, #10415, .T. ) ;
#30430 = DIRECTION ( 'NONE',  ( 0.000000000000000000, 0.000000000000000000, -1.000000000000000000 ) ) ;
#30431 = CARTESIAN_POINT ( 'NONE',  ( 23.92067639343244778, 4.177307434159622801, 1.236145424036337426 ) ) ;
#30432 = DIRECTION ( 'NONE',  ( 0.000000000000000000, 0.000000000000000000, 1.000000000000000000 ) ) ;
#30433 = DIRECTION ( 'NONE',  ( 1.000000000000000000, 8.959828616340678715E-16, 0.000000000000000000 ) ) ;
#30434 = CARTESIAN_POINT ( 'NONE',  ( 81.53696963055323010, 62.69563756174483160, 2.920975158735852784 ) ) ;
#30435 = CARTESIAN_POINT ( 'NONE',  ( 85.74309555164268204, 1.026708856660649705, -5.825338620068188256 ) ) ;
#30436 = CARTESIAN_POINT ( 'NONE',  ( -40.87867591359218977, -26.64985754041175525, 6.700000000000000178 ) ) ;
#30437 = ORIENTED_EDGE ( 'NONE', *, *, #10963, .F. ) ;
#30438 = DIRECTION ( 'NONE',  ( -7.232507224765808510E-18, 1.000000000000000000, 0.000000000000000000 ) ) ;
#30439 = EDGE_CURVE ( 'NONE', #8770, #4319, #33691, .T. ) ;
#30440 = CARTESIAN_POINT ( 'NONE',  ( -70.92837670882107659, -60.53509472482660669, 5.950000000000010836 ) ) ;
#30441 = CARTESIAN_POINT ( 'NONE',  ( 19.68627602041497582, -2.909546155338069262, -3.262843111110074190 ) ) ;
#30442 = DIRECTION ( 'NONE',  ( -1.000000000000000000, 0.000000000000000000, 0.000000000000000000 ) ) ;
#30443 = FACE_OUTER_BOUND ( 'NONE', #35916, .T. ) ;
#30444 = B_SPLINE_CURVE_WITH_KNOTS ( 'NONE', 3,
 ( #38033, #32678, #35177, #13527, #19904, #6755, #29577, #32477, #28781, #26098 ),
 .UNSPECIFIED., .F., .F.,
 ( 4, 3, 3, 4 ),
 ( 9.697399036122160616E-19, 3.025570593003526365E-05, 6.051145698344814338E-05, 6.468151674593860048E-05 ),
 .UNSPECIFIED. ) ;
#30445 = ADVANCED_FACE ( 'NONE', ( #5470 ), #18880, .T. ) ;
#30446 = CARTESIAN_POINT ( 'NONE',  ( 1.906962465809825202, -26.17621130067962554, 6.929923840112063083 ) ) ;
#30447 = VERTEX_POINT ( 'NONE', #8127 ) ;
#30448 = CARTESIAN_POINT ( 'NONE',  ( 34.77322202883802760, -3.158692642683334384, 5.633600309789820848 ) ) ;
#30449 = VECTOR ( 'NONE', #24067, 1000.000000000000000 ) ;
#30450 = ADVANCED_FACE ( 'NONE', ( #27499 ), #33496, .F. ) ;
#30451 = CARTESIAN_POINT ( 'NONE',  ( 87.55151927672237377, 0.01570269930849589254, 4.249584817138070569 ) ) ;
#30452 = ORIENTED_EDGE ( 'NONE', *, *, #10120, .F. ) ;
#30453 = ORIENTED_EDGE ( 'NONE', *, *, #30439, .F. ) ;
#30455 = CARTESIAN_POINT ( 'NONE',  ( 20.92045951437903994, 4.581793376609706314, 2.649698315330352827 ) ) ;
#30454 = CARTESIAN_POINT ( 'NONE',  ( 80.91044703854151976, 63.42644682079063045, -3.500437194783537542 ) ) ;
#30456 = CARTESIAN_POINT ( 'NONE',  ( -69.46781065323600046, -47.51068050472974136, 9.893050960843961406 ) ) ;
#30457 = CARTESIAN_POINT ( 'NONE',  ( 3.478437006660350050, -32.58465225576620838, 7.670465701733749420 ) ) ;
#30458 = CARTESIAN_POINT ( 'NONE',  ( 14.77222812468926705, 12.33286846116276614, -2.511961485181769316 ) ) ;
#30459 = ORIENTED_EDGE ( 'NONE', *, *, #38760, .F. ) ;
#30460 = CARTESIAN_POINT ( 'NONE',  ( 0.3457495631895174948, -32.79715019981050972, 7.013842709614101167 ) ) ;
#30461 = ORIENTED_EDGE ( 'NONE', *, *, #27775, .F. ) ;
#30462 = CIRCLE ( 'NONE', #21921, 3.977260115179314770 ) ;
#30463 = VERTEX_POINT ( 'NONE', #1785 ) ;
#30464 = CARTESIAN_POINT ( 'NONE',  ( -22.44874870218064089, -25.49307895267003587, 6.800000000000000711 ) ) ;
#30465 = EDGE_CURVE ( 'NONE', #7270, #30107, #21644, .T. ) ;
#30466 = CARTESIAN_POINT ( 'NONE',  ( 81.13529310646418935, 61.59586411174932152, -2.189516896894245779 ) ) ;
#30467 = CARTESIAN_POINT ( 'NONE',  ( -59.35030935981331623, 27.06751177275600995, -5.142387704658982095 ) ) ;
#30468 = ORIENTED_EDGE ( 'NONE', *, *, #29843, .T. ) ;
#30470 = CARTESIAN_POINT ( 'NONE',  ( 4.292837626212670621, -27.37010842044347925, 7.748216051605120391 ) ) ;
#30469 = CARTESIAN_POINT ( 'NONE',  ( -62.92837670882109080, -52.49535338866469658, 6.000000000000000000 ) ) ;
#30471 = ORIENTED_EDGE ( 'NONE', *, *, #28086, .F. ) ;
#30472 = CARTESIAN_POINT ( 'NONE',  ( 22.76958335768329178, 3.831392003152646275, 3.677966780943355385 ) ) ;
#30473 = CARTESIAN_POINT ( 'NONE',  ( 82.09661666296807425, 62.69434707785882921, -2.190303691588676216 ) ) ;
#30474 = AXIS2_PLACEMENT_3D ( 'NONE', #12073, #8581, #21776 ) ;
#30475 = CARTESIAN_POINT ( 'NONE',  ( -26.44874870218064089, -25.49307895267003587, 6.800000000000000711 ) ) ;
#30476 = ORIENTED_EDGE ( 'NONE', *, *, #2249, .T. ) ;
#30478 = CARTESIAN_POINT ( 'NONE',  ( 20.90243674393227025, -2.659970222288498665, -3.468728799870355317 ) ) ;
#30477 = DIRECTION ( 'NONE',  ( 0.000000000000000000, 0.000000000000000000, -1.000000000000000000 ) ) ;
#30479 = DIRECTION ( 'NONE',  ( 1.000000000000000000, 0.000000000000000000, 0.000000000000000000 ) ) ;
#30480 = CARTESIAN_POINT ( 'NONE',  ( 74.33180802611956040, 62.54477577240979969, 3.494507759124076962 ) ) ;
#30481 = ORIENTED_EDGE ( 'NONE', *, *, #27961, .F. ) ;
#30482 = CARTESIAN_POINT ( 'NONE',  ( 22.43736279192665961, 3.331640513653970181, -4.315273480065289213 ) ) ;
#30483 = EDGE_CURVE ( 'NONE', #5741, #21149, #1783, .T. ) ;
#30484 = DIRECTION ( 'NONE',  ( -5.786005779812646808E-17, 1.000000000000000000, 0.000000000000000000 ) ) ;
#30485 = CARTESIAN_POINT ( 'NONE',  ( 1.512676170941966269, -26.06812520694141355, 7.139344958878410807 ) ) ;
#30486 = EDGE_LOOP ( 'NONE', ( #24941, #577, #3864, #3845 ) ) ;
#30487 = DIRECTION ( 'NONE',  ( -0.000000000000000000, 1.000000000000000000, -0.000000000000000000 ) ) ;
#30488 = CARTESIAN_POINT ( 'NONE',  ( 81.80968396272741927, 62.04343910699811460, 2.011780557866075014 ) ) ;
#30489 = CARTESIAN_POINT ( 'NONE',  ( 85.14289959633329374, 2.721178644307868044, -0.4516327360412458747 ) ) ;
#30490 = CARTESIAN_POINT ( 'NONE',  ( -62.86576508122315943, 38.67912974266877058, -4.000000000000000000 ) ) ;
#30491 = CARTESIAN_POINT ( 'NONE',  ( 2.743233935765024611, -32.91096671533840379, 6.887547729233689076 ) ) ;
#30492 = ORIENTED_EDGE ( 'NONE', *, *, #25488, .T. ) ;
#30493 = CARTESIAN_POINT ( 'NONE',  ( 26.28542322345758819, -3.293173076614191785, 4.155233155835949432 ) ) ;
#30494 = AXIS2_PLACEMENT_3D ( 'NONE', #32481, #29386, #7751 ) ;
#30495 = CIRCLE ( 'NONE', #29804, 0.1000000000000028644 ) ;
#30496 = PLANE ( 'NONE',  #28887 ) ;
#30497 = CARTESIAN_POINT ( 'NONE',  ( 21.25657147360305288, 3.328712036232781557, -3.524000089216284159 ) ) ;
#30498 = CARTESIAN_POINT ( 'NONE',  ( 4.661238701438277232, -31.43633321245790313, 6.870724624169667116 ) ) ;
#30499 = EDGE_CURVE ( 'NONE', #446, #36353, #39425, .T. ) ;
#30500 = ADVANCED_FACE ( 'NONE', ( #23985 ), #23781, .F. ) ;
#30501 = CARTESIAN_POINT ( 'NONE',  ( -14.34874870218063769, -25.49307895267003587, 6.700000000000000178 ) ) ;
#30502 = EDGE_CURVE ( 'NONE', #35504, #16824, #8990, .T. ) ;
#30503 = FACE_OUTER_BOUND ( 'NONE', #30905, .T. ) ;
#30504 = AXIS2_PLACEMENT_3D ( 'NONE', #32205, #16713, #6676 ) ;
#30505 = CARTESIAN_POINT ( 'NONE',  ( 3.679947863870264957, -32.46458404149915111, 7.501983001166817822 ) ) ;
#30506 = EDGE_LOOP ( 'NONE', ( #30802, #33987, #21109, #22635 ) ) ;
#30507 = CARTESIAN_POINT ( 'NONE',  ( 35.36787417293467684, -3.789710888759190155, 5.512881233678236015 ) ) ;
#30508 = CARTESIAN_POINT ( 'NONE',  ( -71.82557191872977853, -0.3413572496726843264, 5.944584973090449864 ) ) ;
#30509 = CARTESIAN_POINT ( 'NONE',  ( 66.87706763805377363, 57.90143666482605056, -3.999241724014405364 ) ) ;
#30510 = FACE_BOUND ( 'NONE', #12532, .T. ) ;
#30511 = ORIENTED_EDGE ( 'NONE', *, *, #12306, .T. ) ;
#30512 = CARTESIAN_POINT ( 'NONE',  ( -0.5769924795711234289, -32.09451502393404354, 7.754798119455333705 ) ) ;
#30513 = CARTESIAN_POINT ( 'NONE',  ( 3.870091955771714165, -32.18765598803872052, 7.779495906702013741 ) ) ;
#30514 = CARTESIAN_POINT ( 'NONE',  ( 66.55049206961604114, 57.90943322382748448, 3.999192535317435571 ) ) ;
#30515 = FACE_OUTER_BOUND ( 'NONE', #30303, .T. ) ;
#30516 = EDGE_LOOP ( 'NONE', ( #9833, #28753, #33665, #564 ) ) ;
#30517 = FACE_OUTER_BOUND ( 'NONE', #2255, .T. ) ;
#30518 = CARTESIAN_POINT ( 'NONE',  ( -1.713032059046489142, -28.79627056164295595, 7.013842709614101167 ) ) ;
#30519 = VERTEX_POINT ( 'NONE', #14111 ) ;
#30520 = CARTESIAN_POINT ( 'NONE',  ( 24.02218326506362089, 3.317473792240205999, 3.324804558572830526 ) ) ;
#30521 = CARTESIAN_POINT ( 'NONE',  ( 81.88789819931514558, 65.48572365615879676, -1.000000000000000000 ) ) ;
#30523 = AXIS2_PLACEMENT_3D ( 'NONE', #5189, #17720, #30304 ) ;
#30522 = CARTESIAN_POINT ( 'NONE',  ( 81.08836214216863425, 62.22329742272083308, 2.932725070486250196 ) ) ;
#30524 = AXIS2_PLACEMENT_3D ( 'NONE', #38865, #29416, #10656 ) ;
#30525 = FACE_OUTER_BOUND ( 'NONE', #26743, .T. ) ;
#30526 = ORIENTED_EDGE ( 'NONE', *, *, #9953, .F. ) ;
#30527 = CARTESIAN_POINT ( 'NONE',  ( 79.44050761702638397, 61.30339496468042171, -3.042889847487479038 ) ) ;
#30529 = CARTESIAN_POINT ( 'NONE',  ( 14.68777614925489772, -4.612119195195942822, -2.500000000000232259 ) ) ;
#30528 = CARTESIAN_POINT ( 'NONE',  ( 22.60590637795996116, 0.2865873366347984619, 6.509088009623860138 ) ) ;
#30530 = CARTESIAN_POINT ( 'NONE',  ( 81.43870310587888639, 62.97649354279380418, -3.113722587672206554 ) ) ;
#30531 = CARTESIAN_POINT ( 'NONE',  ( 78.68856915541800845, 64.27844437337117256, 3.554489553981586170 ) ) ;
#30532 = ORIENTED_EDGE ( 'NONE', *, *, #22528, .F. ) ;
#30533 = VECTOR ( 'NONE', #23945, 1000.000000000000000 ) ;
#30534 = CARTESIAN_POINT ( 'NONE',  ( 36.29481586213307764, -3.617251867669180498, -5.744675751259891605 ) ) ;
#30535 = AXIS2_PLACEMENT_3D ( 'NONE', #9660, #21417, #6175 ) ;
#30536 = CARTESIAN_POINT ( 'NONE',  ( 82.15576060805999248, 62.21674973124325447, 1.325417871280149429 ) ) ;
#30537 =( BOUNDED_CURVE ( )  B_SPLINE_CURVE ( 3, ( #18325, #25341, #12362, #28418 ),
 .UNSPECIFIED., .F., .T. ) 
 B_SPLINE_CURVE_WITH_KNOTS ( ( 4, 4 ),
 ( 4.708531083176466403, 4.895802057644187855 ),
 .UNSPECIFIED. ) 
 CURVE ( )  GEOMETRIC_REPRESENTATION_ITEM ( )  RATIONAL_B_SPLINE_CURVE ( ( 1.000000000000000000, 0.9970795998553221295, 0.9970795998553221295, 1.000000000000000000 ) ) 
 REPRESENTATION_ITEM ( '' )  );
#30539 = CARTESIAN_POINT ( 'NONE',  ( 37.83867290611771494, -6.084034091406928191, 6.000000000000000000 ) ) ;
#30538 = DIRECTION ( 'NONE',  ( -1.000000000000000000, -0.000000000000000000, -0.000000000000000000 ) ) ;
#30540 = CARTESIAN_POINT ( 'NONE',  ( 29.93139500891458127, 0.4880113553092989553, -5.118255730029571460 ) ) ;
#30541 = DIRECTION ( 'NONE',  ( -1.000000000000000000, 4.455221922683638036E-15, 0.000000000000000000 ) ) ;
#30542 = CARTESIAN_POINT ( 'NONE',  ( -2.448748702180640446, -26.64985754041175525, 6.700000000000000178 ) ) ;
#30543 = CARTESIAN_POINT ( 'NONE',  ( 1.585021184048799547, -33.06802824016562425, 6.865482280155369210 ) ) ;
#30544 = EDGE_CURVE ( 'NONE', #14576, #36371, #24407, .T. ) ;
#30545 = CYLINDRICAL_SURFACE ( 'NONE', #18885, 2.500000000000000444 ) ;
#30546 = ORIENTED_EDGE ( 'NONE', *, *, #15616, .F. ) ;
#30547 = DIRECTION ( 'NONE',  ( 0.7660444431189857850, -0.6427876096865300370, -0.000000000000000000 ) ) ;
#30548 = CARTESIAN_POINT ( 'NONE',  ( 0.5371711504799124848, -32.87097875789517332, 7.686927408461904143 ) ) ;
#30549 = EDGE_CURVE ( 'NONE', #17688, #39584, #31537, .T. ) ;
#30550 = CARTESIAN_POINT ( 'NONE',  ( -71.02745642956452343, -48.61702805680358352, 10.00000000000001066 ) ) ;
#30551 = CARTESIAN_POINT ( 'NONE',  ( 2.129437147705529387, -33.04353820846659318, 6.998987538705434552 ) ) ;
#30552 = CARTESIAN_POINT ( 'NONE',  ( 30.88168762873399587, 0.6966114428816204684, -4.496783944086453211 ) ) ;
#30553 = CARTESIAN_POINT ( 'NONE',  ( 30.88127119532873976, -3.422338893432233853, -4.937978149253780202 ) ) ;
#30554 = CARTESIAN_POINT ( 'NONE',  ( 53.63097637064826273, -5.819101496702492327, -6.000000000000000888 ) ) ;
#30555 = CARTESIAN_POINT ( 'NONE',  ( -12.34874870218063947, -26.64985754041175525, 6.700000000000000178 ) ) ;
#30556 = CARTESIAN_POINT ( 'NONE',  ( 1.578585683582352850, -25.86893018339335981, 7.754798119455333705 ) ) ;
#30557 = CARTESIAN_POINT ( 'NONE',  ( 2.664368798089519874, -32.83041366969101205, 6.939395833800439561 ) ) ;
#30558 = CARTESIAN_POINT ( 'NONE',  ( 5.099964974645724070, -29.62376613088546762, 6.889465824494256374 ) ) ;
#30559 = EDGE_CURVE ( 'NONE', #35445, #15320, #25440, .T. ) ;
#30560 = DIRECTION ( 'NONE',  ( 1.000000000000000000, 0.000000000000000000, -0.000000000000000000 ) ) ;
#30561=STYLED_ITEM('',(#40766),#12876);
#30562 = CARTESIAN_POINT ( 'NONE',  ( 14.77500326541903952, -5.175625724643098557, -2.499997102511863911 ) ) ;
#30563 = CARTESIAN_POINT ( 'NONE',  ( 24.36356524659568024, 2.395873619741290206, -4.116030573549343430 ) ) ;
#30564 = EDGE_LOOP ( 'NONE', ( #29458, #10190, #21339, #26163 ) ) ;
#30565 = ORIENTED_EDGE ( 'NONE', *, *, #20110, .T. ) ;
#30566 = CARTESIAN_POINT ( 'NONE',  ( -1.078675913592196167, -24.55319635012989110, 6.700000000000000178 ) ) ;
#30567 = CARTESIAN_POINT ( 'NONE',  ( 70.70040249450607917, 60.07892802134021792, -3.908768822720051883 ) ) ;
#30568 = AXIS2_PLACEMENT_3D ( 'NONE', #11700, #36433, #6527 ) ;
#30569 = CARTESIAN_POINT ( 'NONE',  ( 2.277526804980155362, -33.02201842327861669, 6.894806418505347700 ) ) ;
#30570 = ORIENTED_EDGE ( 'NONE', *, *, #35999, .F. ) ;
#30571 = CARTESIAN_POINT ( 'NONE',  ( 85.92174427069515730, 0.4035765525155806666, 6.008818417626160979 ) ) ;
#30572 = CARTESIAN_POINT ( 'NONE',  ( -61.00670947824507806, 24.84364830758654108, 8.800414904976364028 ) ) ;
#30573 = CARTESIAN_POINT ( 'NONE',  ( -2.253834945959114489, -26.23431501015891243, 7.635761828346577573 ) ) ;
#30574 = DIRECTION ( 'NONE',  ( -0.000000000000000000, -1.000000000000000000, -0.000000000000000000 ) ) ;
#30576 = CARTESIAN_POINT ( 'NONE',  ( 1.222977352880459723, -26.20361512455695774, 6.864276522220859711 ) ) ;
#30575 = CARTESIAN_POINT ( 'NONE',  ( -0.9390753546024662723, -27.27138652691368037, 6.870737987065013819 ) ) ;
#30577 = ITEM_DEFINED_TRANSFORMATION ( 'NONE', 'NONE', #1818,  #30744 ) ;
#30578 = CARTESIAN_POINT ( 'NONE',  ( -16.44874870218064089, -25.49307895267003587, 6.800000000000000711 ) ) ;
#30579 = ORIENTED_EDGE ( 'NONE', *, *, #9020, .F. ) ;
#30580 = FACE_OUTER_BOUND ( 'NONE', #18449, .T. ) ;
#30581 = SURFACE_SIDE_STYLE ('',( #37347 ) ) ;
#30582 = EDGE_LOOP ( 'NONE', ( #14583, #12548, #32528, #3819 ) ) ;
#30583 = VERTEX_POINT ( 'NONE', #12460 ) ;
#30584 = CARTESIAN_POINT ( 'NONE',  ( 80.20116317610164458, 62.79640268260013158, -3.571698303486882331 ) ) ;
#30585 = CARTESIAN_POINT ( 'NONE',  ( 15.99304537737771703, 7.920163261466188764, -3.484773916741529476 ) ) ;
#30586 = B_SPLINE_CURVE_WITH_KNOTS ( 'NONE', 3,
 ( #17646, #11875, #40094, #39681, #37006, #30226, #8788, #2042, #30024, #2662 ),
 .UNSPECIFIED., .F., .F.,
 ( 4, 3, 3, 4 ),
 ( 0.0001585009270395752084, 0.0001815657551981840858, 0.0002118214035944140504, 0.0002170292169044743470 ),
 .UNSPECIFIED. ) ;
#30587 = CARTESIAN_POINT ( 'NONE',  ( 81.36533387373951598, 61.41589781867487829, -1.313329331391850374 ) ) ;
#30588 = CARTESIAN_POINT ( 'NONE',  ( 78.66571724150243483, 65.64011997358944939, 2.392122129321807567 ) ) ;
#30589 = VECTOR ( 'NONE', #12516, 1000.000000000000000 ) ;
#30590 = CARTESIAN_POINT ( 'NONE',  ( 23.53282518156592573, 3.062426620546339073, 3.879264531747849354 ) ) ;
#30591 = VECTOR ( 'NONE', #7104, 1000.000000000000000 ) ;
#30593 = ORIENTED_EDGE ( 'NONE', *, *, #34749, .F. ) ;
#30592 = LINE ( 'NONE', #26875, #25519 ) ;
#30594 = CARTESIAN_POINT ( 'NONE',  ( 21.85643539959774273, 9.172641120068929510, -1.679843024921975347 ) ) ;
#30595 = ORIENTED_EDGE ( 'NONE', *, *, #37601, .T. ) ;
#30596 = CARTESIAN_POINT ( 'NONE',  ( -80.58817961249317818, 10.50547908170135791, 5.356801284506212291 ) ) ;
#30597 = CARTESIAN_POINT ( 'NONE',  ( 2.778259044425222868, -32.89982485500929954, 7.750000000000000888 ) ) ;
#30598 = CIRCLE ( 'NONE', #3670, 0.9999999999999991118 ) ;
#30599 = CARTESIAN_POINT ( 'NONE',  ( 0.8386806441584250260, -25.38437669007690900, 7.754798119455333705 ) ) ;
#30600 = CARTESIAN_POINT ( 'NONE',  ( -76.08100811359271631, 8.922477016430406138, -8.599497118620481828 ) ) ;
#30601 = DIRECTION ( 'NONE',  ( 0.4690749385695657803, 0.8831583674551003460, -0.000000000000000000 ) ) ;
#30602 = CARTESIAN_POINT ( 'NONE',  ( 2.493534863053076922, -26.26373349863179740, 6.979335674598005745 ) ) ;
#30603 = CARTESIAN_POINT ( 'NONE',  ( -1.741606627443540223, -30.11652268061110860, 7.785593909369613819 ) ) ;
#30604 = CARTESIAN_POINT ( 'NONE',  ( 14.86299874107311325, 12.06992840946315937, 2.526128435164121111 ) ) ;
#30605 = DIRECTION ( 'NONE',  ( 1.000000000000000000, 0.000000000000000000, -0.000000000000000000 ) ) ;
#30606 = CARTESIAN_POINT ( 'NONE',  ( -75.45330471031414277, 33.71485196875532608, -8.800414904976364028 ) ) ;
#30607 = CARTESIAN_POINT ( 'NONE',  ( 4.668948836787977896, -27.91232378075620701, 6.894806418505348589 ) ) ;
#30608 = EDGE_CURVE ( 'NONE', #4541, #4809, #7678, .T. ) ;
#30609 = EDGE_CURVE ( 'NONE', #20740, #29030, #38879, .T. ) ;
#30610 = CARTESIAN_POINT ( 'NONE',  ( -70.92837670882107659, -23.80776546975053520, -10.00000000000000533 ) ) ;
#30611 = CARTESIAN_POINT ( 'NONE',  ( -0.4414210011093676611, -26.92935349710845827, 6.887041543973313473 ) ) ;
#30612 = EDGE_CURVE ( 'NONE', #4540, #3011, #4438, .T. ) ;
#30613 = CARTESIAN_POINT ( 'NONE',  ( 25.67085356133009810, 2.140750286663625879, -4.140177559339564439 ) ) ;
#30614 = EDGE_LOOP ( 'NONE', ( #31638, #33141, #9506, #37489 ) ) ;
#30615 = CARTESIAN_POINT ( 'NONE',  ( 67.62039053056824400, 58.58799842263783120, 3.976226663256290372 ) ) ;
#30616 = CARTESIAN_POINT ( 'NONE',  ( 35.45469368754801565, -1.911696930450387688, 5.739960443585752969 ) ) ;
#30617 = LINE ( 'NONE', #34130, #1410 ) ;
#30618 = AXIS2_PLACEMENT_3D ( 'NONE', #23605, #14525, #24208 ) ;
#30619 = CARTESIAN_POINT ( 'NONE',  ( -0.2487487021806331078, -26.64985754041175525, 6.700000000000000178 ) ) ;
#30620 = AXIS2_PLACEMENT_3D ( 'NONE', #11740, #14436, #24318 ) ;
#30621 = CARTESIAN_POINT ( 'NONE',  ( 88.31640312351544253, -1.506181138579067103, 3.771763452802144201 ) ) ;
#30623 = CARTESIAN_POINT ( 'NONE',  ( 4.872722190795648167, -30.79319270744810311, 6.880147297696983522 ) ) ;
#30622 = CARTESIAN_POINT ( 'NONE',  ( 33.69128717328723610, -4.440785898112559416, 4.348130384999381981 ) ) ;
#30624 = CYLINDRICAL_SURFACE ( 'NONE', #27422, 0.09010775117052947925 ) ;
#30625 = ORIENTED_EDGE ( 'NONE', *, *, #22203, .T. ) ;
#30626 = CARTESIAN_POINT ( 'NONE',  ( -1.605257465718879395, -28.77450919976473998, 6.969307238440508812 ) ) ;
#30627 = CARTESIAN_POINT ( 'NONE',  ( 86.05684172526336795, 1.348548140555935193, 5.632715373612032117 ) ) ;
#30628 = AXIS2_PLACEMENT_3D ( 'NONE', #9378, #34941, #6309 ) ;
#30629 = VERTEX_POINT ( 'NONE', #18841 ) ;
#30630 = FACE_OUTER_BOUND ( 'NONE', #15352, .T. ) ;
#30631 = ORIENTED_EDGE ( 'NONE', *, *, #7388, .T. ) ;
#30632 = CARTESIAN_POINT ( 'NONE',  ( 78.89219914629886432, 65.63660985470716014, -2.576318598473995358 ) ) ;
#30633 = CARTESIAN_POINT ( 'NONE',  ( 87.04213330793400871, 0.5878691963681514920, -4.891134986362597914 ) ) ;
#30634 = CARTESIAN_POINT ( 'NONE',  ( 80.76107640992965742, 62.37607017537889931, 3.233326467035614105 ) ) ;
#30635 = CARTESIAN_POINT ( 'NONE',  ( 21.81854301884185432, 0.2747606569782626851, 8.209505977014627476 ) ) ;
#30637 = VERTEX_POINT ( 'NONE', #21536 ) ;
#30636 = CARTESIAN_POINT ( 'NONE',  ( 3.021324086407803478, -26.64985754041175525, 6.700000000000000178 ) ) ;
#30638 = CARTESIAN_POINT ( 'NONE',  ( 74.39246203999459794, 62.41596060291494297, -3.584990529380562840 ) ) ;
#30639 = CARTESIAN_POINT ( 'NONE',  ( 3.353554235774506953, -32.54096636651022578, 6.889465824494256374 ) ) ;
#30641 = CARTESIAN_POINT ( 'NONE',  ( 24.97205702378243330, -5.748183807572947224, 2.896408662958795066 ) ) ;
#30640 = CARTESIAN_POINT ( 'NONE',  ( -23.07867591359219617, -26.64985754041175525, 6.800000000000000711 ) ) ;
#30642 = CYLINDRICAL_SURFACE ( 'NONE', #36670, 7.744449365083023729 ) ;
#30643 = CARTESIAN_POINT ( 'NONE',  ( 24.69630075600026231, 2.999063368822487252, -3.452992298664733006 ) ) ;
#30644 = EDGE_LOOP ( 'NONE', ( #13202, #10571, #24248, #1343 ) ) ;
#30645 = CARTESIAN_POINT ( 'NONE',  ( -1.797340250851707344, -29.44390463015740522, 7.750000000000000888 ) ) ;
#30646 = AXIS2_PLACEMENT_3D ( 'NONE', #40662, #34520, #6297 ) ;
#30647 = AXIS2_PLACEMENT_3D ( 'NONE', #26318, #29597, #19923 ) ;
#30648 = CARTESIAN_POINT ( 'NONE',  ( 21.82633783062472688, 5.573671403123425350, 3.484773800359227014 ) ) ;
#30649 = CARTESIAN_POINT ( 'NONE',  ( 1.001059401594865061, -32.99204059322197935, 7.776484688137380807 ) ) ;
#30650 = CARTESIAN_POINT ( 'NONE',  ( 81.25398435008600018, 63.24110186484338669, 3.279590910093575840 ) ) ;
#30651 = CARTESIAN_POINT ( 'NONE',  ( 84.34456690318765482, 2.887654542466673746, -2.101772343363317752 ) ) ;
#30652 = CARTESIAN_POINT ( 'NONE',  ( 17.34292908646689568, 9.186004740436843008, 2.849848300167282744 ) ) ;
#30653 = ORIENTED_EDGE ( 'NONE', *, *, #507, .F. ) ;
#30654 = CYLINDRICAL_SURFACE ( 'NONE', #387, 2.499999999999996891 ) ;
#30655 = VECTOR ( 'NONE', #40386, 1000.000000000000000 ) ;
#30656 = ORIENTED_EDGE ( 'NONE', *, *, #3110, .F. ) ;
#30657 = FACE_OUTER_BOUND ( 'NONE', #24690, .T. ) ;
#30658 = CARTESIAN_POINT ( 'NONE',  ( 14.73050576274141932, -5.057416755502635475, -2.496373688475125974 ) ) ;
#30659 = ADVANCED_FACE ( 'NONE', ( #327 ), #31198, .T. ) ;
#30660 = CARTESIAN_POINT ( 'NONE',  ( 31.71708122509442873, -0.5641260517970680954, -5.156615624320846969 ) ) ;
#30661 = CARTESIAN_POINT ( 'NONE',  ( 1.700390093233090871, -29.56993018339339940, -6.000000000000001776 ) ) ;
#30662 = CARTESIAN_POINT ( 'NONE',  ( -63.03213158086253287, 38.26878225442504800, 4.032857076801014351 ) ) ;
#30663 = ORIENTED_EDGE ( 'NONE', *, *, #37780, .F. ) ;
#30664 = CARTESIAN_POINT ( 'NONE',  ( 34.77318038334062322, -3.160091470131585645, 5.633593810002675006 ) ) ;
#30665 = CARTESIAN_POINT ( 'NONE',  ( -17.69482985384421880, -42.37473357531882101, 6.000000000000000000 ) ) ;
#30666 = ORIENTED_EDGE ( 'NONE', *, *, #22009, .F. ) ;
#30667 = ORIENTED_EDGE ( 'NONE', *, *, #6059, .T. ) ;
#30669 = CARTESIAN_POINT ( 'NONE',  ( 37.18695530022691287, -2.963565836837915413, 6.000026294647724079 ) ) ;
#30668 = CARTESIAN_POINT ( 'NONE',  ( 79.92139222979439239, 65.15389119341904234, -3.261148789966887840 ) ) ;
#30670 = CARTESIAN_POINT ( 'NONE',  ( -70.92837670882107659, 13.87661300689593880, 0.000000000000000000 ) ) ;
#30671 = B_SPLINE_CURVE_WITH_KNOTS ( 'NONE', 3,
 ( #19816, #35483, #495, #22521, #25594, #13232, #891, #29289, #35089, #20011, #19622, #31780, #22720, #22913, #13637, #10535, #13030, #13427, #9938, #6863, #6664, #26002, #31990, #1105 ),
 .UNSPECIFIED., .F., .F.,
 ( 4, 1, 1, 1, 1, 1, 1, 2, 2, 1, 1, 1, 1, 1, 1, 2, 2, 4 ),
 ( 0.000000000000000000, 0.2500000000000391354, 0.3750000000000583422, 0.4375000000000676681, 0.4687500000000721645, 0.4843750000000747735, 0.4921875000000763833, 0.4960937500000768829, 0.5000000000000773825, 0.6250000000000768274, 0.6875000000000761613, 0.7187500000000758282, 0.7343750000000756062, 0.7421875000000754952, 0.7460937500000754952, 0.7480468750000754952, 0.7500000000000753841, 1.000000000000000000 ),
 .UNSPECIFIED. ) ;
#30672 = CARTESIAN_POINT ( 'NONE',  ( 15.01265474174107162, -4.182841212154375654, -2.538985411732104236 ) ) ;
#30673 = CARTESIAN_POINT ( 'NONE',  ( 14.72830186849878942, 12.61371249419844176, -2.505105730542713349 ) ) ;
#30674 = ORIENTED_EDGE ( 'NONE', *, *, #33012, .T. ) ;
#30675 = CARTESIAN_POINT ( 'NONE',  ( -2.954197855305039422, -12.43481156997016157, 1.000000000000000000 ) ) ;
#30676 = VERTEX_POINT ( 'NONE', #22453 ) ;
#30677 = ORIENTED_EDGE ( 'NONE', *, *, #24881, .T. ) ;
#30678 = CARTESIAN_POINT ( 'NONE',  ( 5.654615132425274027, -32.90554535662791835, 7.635761828346577573 ) ) ;
#30679 = CARTESIAN_POINT ( 'NONE',  ( 80.65823571794965119, 63.30623879605501259, -3.578839808218915230 ) ) ;
#30680 = AXIS2_PLACEMENT_3D ( 'NONE', #20935, #5291, #18450 ) ;
#30681 = CARTESIAN_POINT ( 'NONE',  ( -58.83253814471410692, 27.61819298006735224, -3.984408728655165710 ) ) ;
#30682 = VERTEX_POINT ( 'NONE', #34825 ) ;
#30683 = EDGE_CURVE ( 'NONE', #16841, #6774, #28073, .T. ) ;
#30685 = CARTESIAN_POINT ( 'NONE',  ( 14.73750015949773484, 12.90700633731061409, 2.501527175807433334 ) ) ;
#30684 = CARTESIAN_POINT ( 'NONE',  ( 23.87849444185487258, 2.668685871580891877, 4.066325986815254367 ) ) ;
#30686 = VERTEX_POINT ( 'NONE', #28196 ) ;
#30687 = CARTESIAN_POINT ( 'NONE',  ( 82.15165036511221786, 63.00212529317509080, -2.340562087103692956 ) ) ;
#30688 = CARTESIAN_POINT ( 'NONE',  ( -13.07867591359219617, -26.64985754041175525, 6.800000000000000711 ) ) ;
#30689 = EDGE_LOOP ( 'NONE', ( #15008, #29611, #31542, #6100 ) ) ;
#30691 = CARTESIAN_POINT ( 'NONE',  ( 26.95243645308021385, -2.795055227801056308, -4.412977574278784232 ) ) ;
#30690 = DIRECTION ( 'NONE',  ( 0.9267318687906785923, -0.3757233601570932335, 2.607104533349591435E-15 ) ) ;
#30692 = CARTESIAN_POINT ( 'NONE',  ( -1.794949259926919227, -29.38927334556171544, 6.998987538705436329 ) ) ;
#30693 = CARTESIAN_POINT ( 'NONE',  ( 75.02040913282911561, 59.50525224047964201, 3.395557233589185042 ) ) ;
#30694 = CARTESIAN_POINT ( 'NONE',  ( 23.69828321319373288, 3.038820287558408051, -3.842211770153025174 ) ) ;
#30695 = ORIENTED_EDGE ( 'NONE', *, *, #11932, .T. ) ;
#30696 = CARTESIAN_POINT ( 'NONE',  ( 0.5043319404286802365, -26.38725126186910686, 7.680992449362120666 ) ) ;
#30697 = EDGE_CURVE ( 'NONE', #1634, #7170, #25533, .T. ) ;
#30698 = CARTESIAN_POINT ( 'NONE',  ( 21.85643539959777826, -13.51165962708896728, -8.254727072381385256 ) ) ;
#30699 = DIRECTION ( 'NONE',  ( 0.000000000000000000, -1.000000000000000000, -0.000000000000000000 ) ) ;
#30700 = EDGE_LOOP ( 'NONE', ( #21024, #4441, #27340, #9140 ) ) ;
#30701 = CARTESIAN_POINT ( 'NONE',  ( 0.1384972100046504007, -34.01952225562621379, 7.695279973900954751 ) ) ;
#30702 = ORIENTED_EDGE ( 'NONE', *, *, #36035, .F. ) ;
#30703 = CARTESIAN_POINT ( 'NONE',  ( 81.83960663661416390, 62.56551448482344568, 2.484976468875359057 ) ) ;
#30704 = CARTESIAN_POINT ( 'NONE',  ( 88.52897200822518187, -1.082218601420786186, 0.1993289098281435523 ) ) ;
#30705 = CARTESIAN_POINT ( 'NONE',  ( 5.141684319425215755, -30.20828278875847062, 6.894806418505347700 ) ) ;
#30706 = CARTESIAN_POINT ( 'NONE',  ( 2.845456134469579457, -32.87731945005177181, 6.875671892026061549 ) ) ;
#30707 = CARTESIAN_POINT ( 'NONE',  ( 18.27718096362622546, -3.093593596032681248, 3.021173953333614826 ) ) ;
#30708 = VECTOR ( 'NONE', #2410, 1000.000000000000000 ) ;
#30709 = CARTESIAN_POINT ( 'NONE',  ( -16.27783086239806210, 25.90100547710869705, 2.500000000000000000 ) ) ;
#30710 = EDGE_CURVE ( 'NONE', #28641, #29003, #37382, .T. ) ;
#30711 = CARTESIAN_POINT ( 'NONE',  ( 37.04663327496000846, -2.800723657629412777, -5.988421117405737348 ) ) ;
#30712 =( NAMED_UNIT ( * ) SI_UNIT ( $, .STERADIAN. ) SOLID_ANGLE_UNIT ( ) );
#30713 = CARTESIAN_POINT ( 'NONE',  ( 4.646831710089861289, -31.45898555212992775, 6.887547729233681970 ) ) ;
#30714 = CARTESIAN_POINT ( 'NONE',  ( -8.448748702180639114, -25.49307895267003587, 6.700000000000000178 ) ) ;
#30715 = AXIS2_PLACEMENT_3D ( 'NONE', #27890, #12246, #8948 ) ;
#30716 = VECTOR ( 'NONE', #26210, 1000.000000000000000 ) ;
#30717 = CARTESIAN_POINT ( 'NONE',  ( 1.575771303524207134, -33.06771121410476155, 7.751599049952198506 ) ) ;
#30718 = CARTESIAN_POINT ( 'NONE',  ( -69.73579169773952913, -46.20201783773000415, 5.880545134273299723 ) ) ;
#30719 = ORIENTED_EDGE ( 'NONE', *, *, #2526, .T. ) ;
#30720 = CARTESIAN_POINT ( 'NONE',  ( 36.10471242579632190, -1.581987752735663166, 5.680909380111648588 ) ) ;
#30721 = DIRECTION ( 'NONE',  ( -1.000000000000000000, -5.331188706255073750E-15, 0.000000000000000000 ) ) ;
#30722 = CARTESIAN_POINT ( 'NONE',  ( 66.94886299149460740, 58.16124406473343811, -3.993952884371009926 ) ) ;
#30723 = DIRECTION ( 'NONE',  ( 0.000000000000000000, -0.6605219282605377940, -0.7508067542896645907 ) ) ;
#30724 = EDGE_CURVE ( 'NONE', #19287, #16154, #27583, .T. ) ;
#30725 = DIRECTION ( 'NONE',  ( 0.000000000000000000, 1.000000000000000000, 0.000000000000000000 ) ) ;
#30726 = ORIENTED_EDGE ( 'NONE', *, *, #26958, .T. ) ;
#30727 = CARTESIAN_POINT ( 'NONE',  ( -0.5665229445002866182, -32.10393105754645404, 7.768425012602599544 ) ) ;
#30728 = CARTESIAN_POINT ( 'NONE',  ( -80.88560043480099182, -6.600306782100017422, -1.015383303423792460 ) ) ;
#30729 = CARTESIAN_POINT ( 'NONE',  ( 76.21257126924976433, 64.31732071985945254, 2.649600530246794872 ) ) ;
#30730 = ORIENTED_EDGE ( 'NONE', *, *, #15054, .T. ) ;
#30731 = CARTESIAN_POINT ( 'NONE',  ( -22.24874870218063450, -26.64985754041175525, 6.700000000000000178 ) ) ;
#30732 = CARTESIAN_POINT ( 'NONE',  ( -13.07867591359219617, -26.64985754041175525, 6.700000000000000178 ) ) ;
#30733 = ORIENTED_EDGE ( 'NONE', *, *, #6102, .T. ) ;
#30734 = CARTESIAN_POINT ( 'NONE',  ( 23.42568583973897844, 3.752714481185509765, 3.194445122559177452 ) ) ;
#30735 = CARTESIAN_POINT ( 'NONE',  ( 81.88789819931514558, 65.48572365615879676, -1.161365684106807850 ) ) ;
#30736 = CARTESIAN_POINT ( 'NONE',  ( 80.42360172120015704, 63.56407742133696104, 3.661914029440276330 ) ) ;
#30737 = VECTOR ( 'NONE', #40704, 1000.000000000000000 ) ;
#30738 = CARTESIAN_POINT ( 'NONE',  ( 1.700390093233090871, -29.56993018339339940, 7.750000000000000888 ) ) ;
#30739 = ORIENTED_EDGE ( 'NONE', *, *, #6443, .T. ) ;
#30740 = CARTESIAN_POINT ( 'NONE',  ( 78.71019189666368732, 60.57837954350633680, -2.701592190110933878 ) ) ;
#30742 = CARTESIAN_POINT ( 'NONE',  ( 14.76691882379872034, -5.164572653182437634, -2.499999999999999556 ) ) ;
#30741 = CARTESIAN_POINT ( 'NONE',  ( 22.28825410457798384, 0.2534056759817530091, 7.122325049175724843 ) ) ;
#30743 = EDGE_CURVE ( 'NONE', #8555, #5492, #26649, .T. ) ;
#30744 = AXIS2_PLACEMENT_3D ( 'NONE', #35448, #9485, #3553 ) ;
#30745 = EDGE_CURVE ( 'NONE', #6204, #18417, #13217, .T. ) ;
#30746 = CARTESIAN_POINT ( 'NONE',  ( 80.79838846786208251, 64.52093256242186214, -3.402511877377343286 ) ) ;
#30747 = CARTESIAN_POINT ( 'NONE',  ( 79.50866325991141537, 61.15032965923190034, 2.842954625922348821 ) ) ;
#30748 = VECTOR ( 'NONE', #8901, 1000.000000000000000 ) ;
#30749 = VERTEX_POINT ( 'NONE', #18730 ) ;
#30750 = AXIS2_PLACEMENT_3D ( 'NONE', #32497, #20317, #29999 ) ;
#30751 = EDGE_CURVE ( 'NONE', #7709, #32308, #32039, .T. ) ;
#30752 = DIRECTION ( 'NONE',  ( -0.000000000000000000, -0.000000000000000000, -1.000000000000000000 ) ) ;
#30753 = CARTESIAN_POINT ( 'NONE',  ( 81.94344439483592168, 61.95170768642839221, 1.250177805244208740 ) ) ;
#30755 = CARTESIAN_POINT ( 'NONE',  ( -1.697684928147993766, -29.45553547605979006, 6.864276522220859711 ) ) ;
#30754 = DIRECTION ( 'NONE',  ( 0.000000000000000000, 0.000000000000000000, 1.000000000000000000 ) ) ;
#30756 = CARTESIAN_POINT ( 'NONE',  ( 29.97449823033972649, -1.245471885678776980, 6.039028575696650414 ) ) ;
#30757 = CARTESIAN_POINT ( 'NONE',  ( -1.764597594712412176, -30.06375234003086305, 6.865482280155368322 ) ) ;
#30758 = CARTESIAN_POINT ( 'NONE',  ( -62.92837670882106238, 3.729367930467588632, -6.000000000000000000 ) ) ;
#30759 = CARTESIAN_POINT ( 'NONE',  ( 1.669309969508061764, -33.06979218437418666, 6.894806418505347700 ) ) ;
#30760 = DIRECTION ( 'NONE',  ( -0.9396926207859104263, 0.3420201433256631063, -0.000000000000000000 ) ) ;
#30761 = VERTEX_POINT ( 'NONE', #25333 ) ;
#30762 = CARTESIAN_POINT ( 'NONE',  ( -18.27651686900387418, -64.04014080848075707, 2.500000000000000000 ) ) ;
#30763 = CARTESIAN_POINT ( 'NONE',  ( 80.30486976649511632, 60.99341039245124563, 1.909076843291450443 ) ) ;
#30764 = DIRECTION ( 'NONE',  ( 1.000000000000000000, 0.000000000000000000, 0.000000000000000000 ) ) ;
#30765 = EDGE_CURVE ( 'NONE', #26557, #29356, #28621, .T. ) ;
#30766 = CARTESIAN_POINT ( 'NONE',  ( 36.65987745959532162, -1.958086723934334694, -5.826241878318064060 ) ) ;
#30767 = DIRECTION ( 'NONE',  ( 1.000000000000000000, 0.000000000000000000, 0.000000000000000000 ) ) ;
#30768 = CARTESIAN_POINT ( 'NONE',  ( 5.200252094213874798, -29.60101030711846448, 6.894806418505347700 ) ) ;
#30769 = CARTESIAN_POINT ( 'NONE',  ( -0.06872588940044967176, -26.54995493937659390, 7.743886751744251562 ) ) ;
#30770 = CYLINDRICAL_SURFACE ( 'NONE', #31148, 3.399999999999999911 ) ;
#30771 = LINE ( 'NONE', #6461, #37155 ) ;
#30772 = CARTESIAN_POINT ( 'NONE',  ( 4.634748283818988845, -27.85249419169753438, 7.643333865083956624 ) ) ;
#30773 = DIRECTION ( 'NONE',  ( 0.3420201433256662704, 0.9396926207859093161, -0.000000000000000000 ) ) ;
#30774 = CARTESIAN_POINT ( 'NONE',  ( -0.9786759135921931918, -26.64985754041175525, 6.700000000000000178 ) ) ;
#30775 = CARTESIAN_POINT ( 'NONE',  ( 23.40345427751441321, 1.751723352111926424, -4.892213115278092772 ) ) ;
#30776 = ORIENTED_EDGE ( 'NONE', *, *, #19392, .F. ) ;
#30777 = CARTESIAN_POINT ( 'NONE',  ( 14.61802081865033820, -4.461849342347350422, 2.500000000000000000 ) ) ;
#30778 = CIRCLE ( 'NONE', #5129, 0.1000000000000028644 ) ;
#30779 = CARTESIAN_POINT ( 'NONE',  ( 69.23715119732055712, 58.71109548446294468, -3.988427515945585089 ) ) ;
#30780 = B_SPLINE_CURVE_WITH_KNOTS ( 'NONE', 3,
 ( #12592, #2751, #34863, #24753 ),
 .UNSPECIFIED., .F., .F.,
 ( 4, 4 ),
 ( 0.000000000000000000, 6.391136169993470452E-06 ),
 .UNSPECIFIED. ) ;
#30781 = ORIENTED_EDGE ( 'NONE', *, *, #19818, .F. ) ;
#30782 = CARTESIAN_POINT ( 'NONE',  ( -12.97867591359219297, -24.55319635012989110, 6.700000000000000178 ) ) ;
#30783 = LINE ( 'NONE', #21912, #33119 ) ;
#30784 = CARTESIAN_POINT ( 'NONE',  ( 70.02038816076994010, 58.42250406220534131, 3.901551322707178304 ) ) ;
#30785 = CARTESIAN_POINT ( 'NONE',  ( 3.048460970688392280, -26.44859712950919928, 6.997764925645182821 ) ) ;
#30786 = CARTESIAN_POINT ( 'NONE',  ( 1.307187192269261722, -26.19274102632997270, 6.997764925645181044 ) ) ;
#30787 = EDGE_CURVE ( 'NONE', #22121, #29149, #40547, .T. ) ;
#30788 = LINE ( 'NONE', #8520, #1509 ) ;
#30789 = ORIENTED_EDGE ( 'NONE', *, *, #16135, .F. ) ;
#30790 = CARTESIAN_POINT ( 'NONE',  ( 24.07321278147298926, 3.353042105641798720, 3.188969774653739986 ) ) ;
#30791 = EDGE_CURVE ( 'NONE', #2537, #30233, #851, .T. ) ;
#30792 = EDGE_LOOP ( 'NONE', ( #15594, #33466, #39504, #30461 ) ) ;
#30793 = CARTESIAN_POINT ( 'NONE',  ( 79.79522905248630593, 63.61080392591205168, -3.730195463674648604 ) ) ;
#30794 =( BOUNDED_CURVE ( )  B_SPLINE_CURVE ( 3, ( #15658, #24721, #12563, #12764 ),
 .UNSPECIFIED., .F., .T. ) 
 B_SPLINE_CURVE_WITH_KNOTS ( ( 4, 4 ),
 ( 1.381924640371166912, 1.574767692156075372 ),
 .UNSPECIFIED. ) 
 CURVE ( )  GEOMETRIC_REPRESENTATION_ITEM ( )  RATIONAL_B_SPLINE_CURVE ( ( 1.000000000000000000, 0.9969033633783032089, 0.9969033633783032089, 1.000000000000000000 ) ) 
 REPRESENTATION_ITEM ( '' )  );
#30795 = LINE ( 'NONE', #21314, #23022 ) ;
#30796 = CARTESIAN_POINT ( 'NONE',  ( 81.53193199008818226, 61.58838919619021368, -1.571309534768102090 ) ) ;
#30797 = CARTESIAN_POINT ( 'NONE',  ( 78.41749725426429052, 65.86496093260605278, 1.552792442904350034 ) ) ;
#30798 = EDGE_CURVE ( 'NONE', #31282, #19582, #33354, .T. ) ;
#30799 = AXIS2_PLACEMENT_3D ( 'NONE', #3291, #9626, #35178 ) ;
#30800 = CARTESIAN_POINT ( 'NONE',  ( -64.97837670882105954, -56.35932253828836025, 0.000000000000000000 ) ) ;
#30802 = ORIENTED_EDGE ( 'NONE', *, *, #2836, .F. ) ;
#30801 = CARTESIAN_POINT ( 'NONE',  ( 2.843927967873976392, -32.77186954725888768, 7.779495906702012853 ) ) ;
#30803 = CARTESIAN_POINT ( 'NONE',  ( 21.85643539959778181, 8.766930670454163632, 4.215001190429523703 ) ) ;
#30804 = ORIENTED_EDGE ( 'NONE', *, *, #16875, .F. ) ;
#30805 = B_SPLINE_CURVE_WITH_KNOTS ( 'NONE', 3,
 ( #27010, #24528, #14635, #33815, #23712, #34029, #5597, #5803, #20822, #15056, #30108, #39350, #8054, #21042, #2532, #14239, #33419, #33615, #33199, #11142, #30727, #11742, #1917, #36676, #30512 ),
 .UNSPECIFIED., .F., .F.,
 ( 4, 3, 3, 3, 3, 3, 3, 3, 4 ),
 ( 6.468151674594082310E-05, 9.076621574721611767E-05, 0.0001210204262067929927, 0.0001512763324577386321, 0.0001815301820994170122, 0.0002117781465860660436, 0.0002420274594459704371, 0.0002722905548971097170, 0.0002816827545175626369 ),
 .UNSPECIFIED. ) ;
#30806 = CARTESIAN_POINT ( 'NONE',  ( -1.799497888696266479, -29.59793221807746022, 7.658262384781102661 ) ) ;
#30807 = CIRCLE ( 'NONE', #37362, 2.500000000000000000 ) ;
#30808 = FACE_BOUND ( 'NONE', #27155, .T. ) ;
#30809 = CARTESIAN_POINT ( 'NONE',  ( -74.79361657344986725, 7.703038357672896019, -10.55606559225674879 ) ) ;
#30810 = DIRECTION ( 'NONE',  ( 0.000000000000000000, -0.000000000000000000, -1.000000000000000000 ) ) ;
#30811 = CARTESIAN_POINT ( 'NONE',  ( 35.73144206629780228, -1.302429614601412711, -5.536403668628991248 ) ) ;
#30812 = CARTESIAN_POINT ( 'NONE',  ( -1.763898702996634871, -30.06273584198100579, 7.761113333116788304 ) ) ;
#30813 = CARTESIAN_POINT ( 'NONE',  ( 14.83438443416239316, 12.32204325522479138, 2.521662480531097206 ) ) ;
#30814 = FACE_OUTER_BOUND ( 'NONE', #35931, .T. ) ;
#30815 = CARTESIAN_POINT ( 'NONE',  ( -2.448748702180640446, -26.64985754041175525, 6.800000000000000711 ) ) ;
#30816 = CARTESIAN_POINT ( 'NONE',  ( 5.042305363714541855, -28.94414881188822619, 7.703977250142848732 ) ) ;
#30817 = CARTESIAN_POINT ( 'NONE',  ( 18.48160911996360056, 13.25447782660471852, -2.499999999999999556 ) ) ;
#30818 = DIRECTION ( 'NONE',  ( -0.000000000000000000, -0.000000000000000000, -1.000000000000000000 ) ) ;
#30819 = CARTESIAN_POINT ( 'NONE',  ( 24.71965336222647736, 2.638756212794581835, -3.924200964849605011 ) ) ;
#30820 = ORIENTED_EDGE ( 'NONE', *, *, #29942, .T. ) ;
#30821 = CARTESIAN_POINT ( 'NONE',  ( 67.53434038244741089, 57.92037869207645429, 3.987264345885670913 ) ) ;
#30822 = CARTESIAN_POINT ( 'NONE',  ( 33.65798956961368305, -1.144971352236924922, 5.459541312528853219 ) ) ;
#30823 = DIRECTION ( 'NONE',  ( -0.000000000000000000, -0.000000000000000000, -1.000000000000000000 ) ) ;
#30824 = EDGE_CURVE ( 'NONE', #10798, #7879, #6186, .T. ) ;
#30825 = CARTESIAN_POINT ( 'NONE',  ( 2.313921169258307931, -33.01434178613541093, 7.762796336881262249 ) ) ;
#30826 = CARTESIAN_POINT ( 'NONE',  ( 86.19964454037233281, 1.163379821962233107, 5.771090254565081068 ) ) ;
#30828 = CARTESIAN_POINT ( 'NONE',  ( 4.876532544628377153, -30.78324251417176072, 6.889465824494259039 ) ) ;
#30827 = CARTESIAN_POINT ( 'NONE',  ( -71.54227241695252815, -21.58327309683471995, 5.969247584478902802 ) ) ;
#30829 = VERTEX_POINT ( 'NONE', #15650 ) ;
#30830 = CARTESIAN_POINT ( 'NONE',  ( -20.34874870218063947, -25.49307895267003587, 6.700000000000000178 ) ) ;
#30831 = CARTESIAN_POINT ( 'NONE',  ( -68.71186372058383540, 37.81212149306784909, 9.800414904976364028 ) ) ;
#30832 = VECTOR ( 'NONE', #13693, 1000.000000000000000 ) ;
#30833 = ORIENTED_EDGE ( 'NONE', *, *, #30089, .T. ) ;
#30834 = LINE ( 'NONE', #34346, #12922 ) ;
#30835 = ORIENTED_EDGE ( 'NONE', *, *, #40287, .T. ) ;
#30836 = CARTESIAN_POINT ( 'NONE',  ( 81.02662073326128223, 61.25180701697230035, -1.364493914842159539 ) ) ;
#30837 = CARTESIAN_POINT ( 'NONE',  ( -1.517625692061476794, -28.19356706969799831, 6.955226052476383813 ) ) ;
#30838 = CARTESIAN_POINT ( 'NONE',  ( 79.84444348018428173, 64.37461814510217550, 3.624000857162003264 ) ) ;
#30840 = VERTEX_POINT ( 'NONE', #26142 ) ;
#30839 = CARTESIAN_POINT ( 'NONE',  ( -0.8432521732669862047, -27.31383173241063389, 6.866852738645442322 ) ) ;
#30841 = EDGE_CURVE ( 'NONE', #34839, #16031, #9942, .T. ) ;
#30842 = CARTESIAN_POINT ( 'NONE',  ( 74.45643886899652841, 62.27924959144220196, -3.661998389317300706 ) ) ;
#30844 = ADVANCED_FACE ( 'NONE', ( #7193 ), #1435, .F. ) ;
#30843 = CARTESIAN_POINT ( 'NONE',  ( -26.34874870218063947, -25.49307895267003587, 6.800000000000000711 ) ) ;
#30845 = AXIS2_PLACEMENT_3D ( 'NONE', #3766, #14206, #4748 ) ;
#30847 = DIRECTION ( 'NONE',  ( -1.000000000000000000, 0.000000000000000000, 0.000000000000000000 ) ) ;
#30846 = CARTESIAN_POINT ( 'NONE',  ( 4.925414808968284319, -30.92978884623197899, 7.006908160621406978 ) ) ;
#30848 = CARTESIAN_POINT ( 'NONE',  ( -10.87867591359219155, -26.64985754041175525, 6.700000000000000178 ) ) ;
#30849 = B_SPLINE_CURVE_WITH_KNOTS ( 'NONE', 3,
 ( #10356, #28282, #31590, #22932, #12634, #22126, #25206, #509, #299, #37736, #25606, #34699, #12838, #25408, #34901, #6678, #19226, #31792, #16136, #10550, #33001, #32405, #26421, #29898, #32606, #35695, #23716, #17319, #38950, #26617, #16927 ),
 .UNSPECIFIED., .F., .F.,
 ( 4, 3, 3, 3, 3, 3, 3, 3, 3, 3, 4 ),
 ( 3.679904200040097469E-18, 3.077658087705444919E-05, 6.152638666998797327E-05, 9.267501192706533602E-05, 0.0001241882240135170300, 0.0001556618703051661765, 0.0001866161554452200268, 0.0002167966385860962497, 0.0002463805737537759716, 0.0002758761370306515685, 0.0002847094172290023386 ),
 .UNSPECIFIED. ) ;
#30850 = CARTESIAN_POINT ( 'NONE',  ( 0.3767051360551654238, -26.43053962681419122, 7.139196562012272373 ) ) ;
#30851 = CARTESIAN_POINT ( 'NONE',  ( 22.20701262861088310, 5.183280470103047932, -3.129361004166391069 ) ) ;
#30852 = ORIENTED_EDGE ( 'NONE', *, *, #27281, .F. ) ;
#30853 = CARTESIAN_POINT ( 'NONE',  ( 0.1825688514504736626, 0.5999999999999995337, -3.931742364880508767 ) ) ;
#30854 = CARTESIAN_POINT ( 'NONE',  ( 26.59415400691353071, 2.826550869980146707, -2.084159418869949043 ) ) ;
#30855 = CARTESIAN_POINT ( 'NONE',  ( 0.1463256921878338668, -32.60189304101577790, 7.139196562012272373 ) ) ;
#30856 = CARTESIAN_POINT ( 'NONE',  ( 0.9923868681965268834, -32.99281228919391395, 7.771081512783695189 ) ) ;
#30857 = CARTESIAN_POINT ( 'NONE',  ( 79.12689763788453945, 66.01933680498311219, 2.028924249969734195 ) ) ;
#30858 = CARTESIAN_POINT ( 'NONE',  ( 86.28404140065768502, 0.1054103399587360407, 6.008803426180587159 ) ) ;
#30859 = CARTESIAN_POINT ( 'NONE',  ( 21.78047190118184773, 5.616103730238553027, 3.473245441588607374 ) ) ;
#30860 = ORIENTED_EDGE ( 'NONE', *, *, #116, .T. ) ;
#30861 = CARTESIAN_POINT ( 'NONE',  ( 2.864725917214215212, -26.26927458485223355, 7.678495282201403427 ) ) ;
#30862 = CARTESIAN_POINT ( 'NONE',  ( 4.634557877658172842, -31.28770606326002124, 7.779495906702013741 ) ) ;
#30863 = AXIS2_PLACEMENT_3D ( 'NONE', #26201, #28879, #32385 ) ;
#30864 = VERTEX_POINT ( 'NONE', #16845 ) ;
#30865 = DIRECTION ( 'NONE',  ( 1.000000000000000000, 0.000000000000000000, 0.000000000000000000 ) ) ;
#30866 = CARTESIAN_POINT ( 'NONE',  ( 33.96709741332558252, -3.701672533693765921, -5.338239117359374397 ) ) ;
#30867 = CARTESIAN_POINT ( 'NONE',  ( -1.432293644835494373, -27.47664038617742577, 4.000000000000000000 ) ) ;
#30868 = DIRECTION ( 'NONE',  ( 0.000000000000000000, 0.000000000000000000, 1.000000000000000000 ) ) ;
#30869 = CARTESIAN_POINT ( 'NONE',  ( 1.909707170198035708, -26.17637943432646708, 6.969307238440505259 ) ) ;
#30870 = CARTESIAN_POINT ( 'NONE',  ( 36.14147691053851474, -3.141484228563025116, 5.847149575448376879 ) ) ;
#30871 = CARTESIAN_POINT ( 'NONE',  ( 4.327908163969746980, -31.72774129374395713, 7.695279973900954751 ) ) ;
#30872 = DIRECTION ( 'NONE',  ( -0.000000000000000000, -0.000000000000000000, -1.000000000000000000 ) ) ;
#30873 = AXIS2_PLACEMENT_3D ( 'NONE', #11661, #11456, #20949 ) ;
#30874 = VERTEX_POINT ( 'NONE', #22852 ) ;
#30875 = ORIENTED_EDGE ( 'NONE', *, *, #29784, .F. ) ;
#30877 = CARTESIAN_POINT ( 'NONE',  ( 35.36839093531861522, -3.794034914966402106, 5.509564447435172596 ) ) ;
#30876 = CARTESIAN_POINT ( 'NONE',  ( 79.06971639787833794, 65.98240043192647875, -2.069468987430130635 ) ) ;
#30878 = CARTESIAN_POINT ( 'NONE',  ( 19.07693085987039439, -3.073520552340138767, -3.127448232901508085 ) ) ;
#30879 = CARTESIAN_POINT ( 'NONE',  ( 14.61802081865033465, 12.33286846116284252, -2.500000000000000000 ) ) ;
#30880 = ORIENTED_EDGE ( 'NONE', *, *, #23369, .F. ) ;
#30881 = CARTESIAN_POINT ( 'NONE',  ( -1.765272865745179498, -30.05733663009887024, 7.754798119455333705 ) ) ;
#30882 = ORIENTED_EDGE ( 'NONE', *, *, #38947, .F. ) ;
#30883 = ORIENTED_EDGE ( 'NONE', *, *, #452, .T. ) ;
#30884 = CARTESIAN_POINT ( 'NONE',  ( 80.20683918224331421, 64.20264744734686246, -3.640670270625566918 ) ) ;
#30885 = CARTESIAN_POINT ( 'NONE',  ( -58.75407610588014506, 29.59432899155028807, -5.651746018159727214 ) ) ;
#30886 = ORIENTED_EDGE ( 'NONE', *, *, #591, .T. ) ;
#30888 = CARTESIAN_POINT ( 'NONE',  ( 20.70168030145549309, 10.21427254645072402, -2.500000000000002220 ) ) ;
#30887 = CARTESIAN_POINT ( 'NONE',  ( 23.18504663067065863, 2.575852116297360883, 4.415027062329348162 ) ) ;
#30889 = EDGE_LOOP ( 'NONE', ( #8096, #34309, #15177, #13607, #40003 ) ) ;
#30890 = CARTESIAN_POINT ( 'NONE',  ( 81.98790212893277385, 62.35967063417181322, -2.110636331688536593 ) ) ;
#30891 = EDGE_CURVE ( 'NONE', #19982, #19304, #16279, .T. ) ;
#30893 = EDGE_CURVE ( 'NONE', #39054, #14484, #19532, .T. ) ;
#30892 = FACE_OUTER_BOUND ( 'NONE', #25611, .T. ) ;
#30894 = ORIENTED_EDGE ( 'NONE', *, *, #24074, .T. ) ;
#30896 = DIRECTION ( 'NONE',  ( -1.000000000000000000, 0.000000000000000000, 0.000000000000000000 ) ) ;
#30895 = DIRECTION ( 'NONE',  ( -0.5000000000000039968, 0.8660254037844363761, -0.000000000000000000 ) ) ;
#30897 = CARTESIAN_POINT ( 'NONE',  ( -1.794313667778303589, -29.37745747938051366, 6.961115707816239784 ) ) ;
#30898 = CARTESIAN_POINT ( 'NONE',  ( 73.54169881536046205, 59.75047131450637750, 3.824679913398719044 ) ) ;
#30899 = ORIENTED_EDGE ( 'NONE', *, *, #20769, .T. ) ;
#30900 = CARTESIAN_POINT ( 'NONE',  ( 22.82378969653115419, 3.379723621962007929, -4.000272552100319956 ) ) ;
#30901 = EDGE_LOOP ( 'NONE', ( #39192, #24240, #13380, #40375 ) ) ;
#30902 = CARTESIAN_POINT ( 'NONE',  ( 21.85643539959780313, 0.4758835581198413989, -14.20546615820951963 ) ) ;
#30903 = TOROIDAL_SURFACE ( 'NONE', #7200, 3.449999999999999289, 0.05000000000000000278 ) ;
#30904 = CARTESIAN_POINT ( 'NONE',  ( 16.12938719714403746, 15.26369590458471315, -1.887449634882855110 ) ) ;
#30905 = EDGE_LOOP ( 'NONE', ( #9275, #1651, #16036, #11735 ) ) ;
#30906 = VERTEX_POINT ( 'NONE', #38877 ) ;
#30907 = CARTESIAN_POINT ( 'NONE',  ( 81.16644189562721579, 61.30283181452514185, 1.054034669007994252 ) ) ;
#30908 = CARTESIAN_POINT ( 'NONE',  ( 85.56873805237422914, 2.242856678970356565, 3.827793690346343869 ) ) ;
#30909 = CARTESIAN_POINT ( 'NONE',  ( 11.29080664838499182, -35.94265729135299381, 6.000000000000000000 ) ) ;
#30910 = CARTESIAN_POINT ( 'NONE',  ( -0.9271279775035500270, -27.41211907304282036, 7.693875151218750652 ) ) ;
#30911 = EDGE_LOOP ( 'NONE', ( #30039, #38090, #30719, #19395 ) ) ;
#30912 = CARTESIAN_POINT ( 'NONE',  ( 26.28072973217529906, -3.205359020229657574, 4.210232032756980658 ) ) ;
#30913 = CARTESIAN_POINT ( 'NONE',  ( -70.92837670882107659, 28.72470171467712063, 0.000000000000000000 ) ) ;
#30914 = CARTESIAN_POINT ( 'NONE',  ( 34.93036046862505373, -1.707846917307844770, -5.658125563726033924 ) ) ;
#30915 = FACE_OUTER_BOUND ( 'NONE', #3613, .T. ) ;
#30916 = CARTESIAN_POINT ( 'NONE',  ( 5.191621582129971380, -29.58803114832194936, 7.778495531946296282 ) ) ;
#30917 = FACE_OUTER_BOUND ( 'NONE', #17061, .T. ) ;
#30918 = EDGE_CURVE ( 'NONE', #8794, #6524, #20834, .T. ) ;
#30920 = AXIS2_PLACEMENT_3D ( 'NONE', #9394, #21979, #15166 ) ;
#30919 = CARTESIAN_POINT ( 'NONE',  ( -28.34874870218063947, -26.64985754041175525, 6.700000000000000178 ) ) ;
#30921 = CARTESIAN_POINT ( 'NONE',  ( -69.93716145283299568, -45.98695738452880732, 5.917975389153444787 ) ) ;
#30922 = EDGE_LOOP ( 'NONE', ( #815, #6502, #31176, #7816, #6545 ) ) ;
#30923 = CARTESIAN_POINT ( 'NONE',  ( 33.04854646635354243, -0.2660208435476467681, 5.100183431173213044 ) ) ;
#30924 = CARTESIAN_POINT ( 'NONE',  ( -71.92602134074772380, -0.7038144147489171498, 5.928523475362950990 ) ) ;
#30925 = CARTESIAN_POINT ( 'NONE',  ( 66.84561829912908593, 57.98873651192412382, -3.999241724016630251 ) ) ;
#30926 = B_SPLINE_CURVE_WITH_KNOTS ( 'NONE', 3,
 ( #34372, #15815, #6143, #18477, #34173, #24458, #37419, #12512, #27953, #21795, #11885, #12718, #28370, #18685, #5938, #34580, #18273, #25087, #15396, #31270, #3089, #15606, #28158, #18902, #181, #25292, #37016, #8599, #21177, #33745, #5524 ),
 .UNSPECIFIED., .F., .F.,
 ( 4, 3, 3, 3, 3, 3, 3, 3, 3, 3, 4 ),
 ( 5.057544569639794935E-18, 3.077658087705700384E-05, 6.152638666998954536E-05, 9.267501192706765350E-05, 0.0001241882240135207434, 0.0001556618703051702694, 0.0001866161554452256104, 0.0002167966385861005865, 0.0002463805737537815010, 0.0002758761370306578569, 0.0002847094172290074343 ),
 .UNSPECIFIED. ) ;
#30927 = DIRECTION ( 'NONE',  ( 1.000000000000000000, 0.000000000000000000, 0.000000000000000000 ) ) ;
#30928 = EDGE_CURVE ( 'NONE', #4780, #15847, #35424, .T. ) ;
#30929 = ORIENTED_EDGE ( 'NONE', *, *, #7037, .F. ) ;
#30930 = DIRECTION ( 'NONE',  ( -1.000000000000000000, 0.000000000000000000, 0.000000000000000000 ) ) ;
#30931 = CIRCLE ( 'NONE', #19077, 0.04999999999999969746 ) ;
#30932 = CYLINDRICAL_SURFACE ( 'NONE', #35142, 0.09010775117052974292 ) ;
#30933 = CARTESIAN_POINT ( 'NONE',  ( 66.96277167016233989, 58.17005278565000026, 3.993702900079018292 ) ) ;
#30934 = ORIENTED_EDGE ( 'NONE', *, *, #27200, .T. ) ;
#30935 = CARTESIAN_POINT ( 'NONE',  ( -7.890026461918812295, -8.913725925455491250, 6.000000000000000000 ) ) ;
#30936 = LINE ( 'NONE', #5605, #4825 ) ;
#30937 = ORIENTED_EDGE ( 'NONE', *, *, #18399, .T. ) ;
#30938 = CARTESIAN_POINT ( 'NONE',  ( 21.73371426548433050, 6.130834824796253635, 3.264951269434681613 ) ) ;
#30939 = CARTESIAN_POINT ( 'NONE',  ( 82.10909544300281482, 65.20937546977818045, -1.165579324820864571 ) ) ;
#30940 = CARTESIAN_POINT ( 'NONE',  ( 81.15397050155256409, 61.44050475792813870, 1.896863055073854332 ) ) ;
#30942 = EDGE_CURVE ( 'NONE', #25058, #18362, #13325, .T. ) ;
#30941 = LINE ( 'NONE', #40181, #12734 ) ;
#30943 = ORIENTED_EDGE ( 'NONE', *, *, #28738, .F. ) ;
#30944 = CARTESIAN_POINT ( 'NONE',  ( 76.31986902294666208, 64.06746608568099077, -3.012346708716354016 ) ) ;
#30946 = DIRECTION ( 'NONE',  ( -0.000000000000000000, -0.000000000000000000, 1.000000000000000000 ) ) ;
#30945 = LINE ( 'NONE', #27825, #14725 ) ;
#30947 = FACE_OUTER_BOUND ( 'NONE', #40506, .T. ) ;
#30948 = CARTESIAN_POINT ( 'NONE',  ( 78.68070521837707076, 66.05171761244720585, -1.104694797982641363 ) ) ;
#30949 = CARTESIAN_POINT ( 'NONE',  ( 77.76298154960849729, 62.57953843473563893, 3.839379600940513892 ) ) ;
#30950 = ORIENTED_EDGE ( 'NONE', *, *, #27000, .T. ) ;
#30951 = AXIS2_PLACEMENT_3D ( 'NONE', #22161, #12875, #31830 ) ;
#30952 = CARTESIAN_POINT ( 'NONE',  ( 4.749297472835599443, -31.28869828601962766, 7.686927408461905920 ) ) ;
#30953 = ORIENTED_EDGE ( 'NONE', *, *, #29201, .F. ) ;
#30954 = CARTESIAN_POINT ( 'NONE',  ( 79.92383974732996421, 66.30194418458920325, 1.599335268229121754 ) ) ;
#30956 = CARTESIAN_POINT ( 'NONE',  ( -1.696079551158403254, -29.41472263061939074, 6.871394612369935651 ) ) ;
#30955 = CARTESIAN_POINT ( 'NONE',  ( -64.08758708074097399, 41.34492105184755673, 2.999999999999999112 ) ) ;
#30957 = CARTESIAN_POINT ( 'NONE',  ( 33.73883514186113075, -4.630787605642836091, -3.992050560354765576 ) ) ;
#30958 = LINE ( 'NONE', #18371, #423 ) ;
#30959 = CARTESIAN_POINT ( 'NONE',  ( -12.97867591359219297, -26.64985754041175525, 6.700000000000000178 ) ) ;
#30960 = CARTESIAN_POINT ( 'NONE',  ( -64.62035675219918573, 36.25855371424984952, 6.071883532254790161 ) ) ;
#30961 = CARTESIAN_POINT ( 'NONE',  ( 21.80351395196640141, 0.2459331218041709566, -8.291272508738018132 ) ) ;
#30962 = DIRECTION ( 'NONE',  ( -0.3757233601570971193, -0.9267318687906769270, 0.000000000000000000 ) ) ;
#30963 = CARTESIAN_POINT ( 'NONE',  ( 5.000416883752518693, -30.73605123097268788, 7.720710062488893577 ) ) ;
#30964 = DIRECTION ( 'NONE',  ( -0.8660254037844344888, -0.5000000000000069944, -0.000000000000000000 ) ) ;
#30965 = DIRECTION ( 'NONE',  ( 0.000000000000000000, 0.000000000000000000, 1.000000000000000000 ) ) ;
#30966 = CARTESIAN_POINT ( 'NONE',  ( 27.78116730204126839, 1.798541041528136653, -4.024397514413323051 ) ) ;
#30967 = CARTESIAN_POINT ( 'NONE',  ( 30.88935601760522687, -3.446417099803610551, -4.925634463943371344 ) ) ;
#30968 = CARTESIAN_POINT ( 'NONE',  ( -2.248748702180634940, -26.64985754041175525, 6.700000000000000178 ) ) ;
#30969 = FACE_OUTER_BOUND ( 'NONE', #38707, .T. ) ;
#30970 = CARTESIAN_POINT ( 'NONE',  ( 0.3950279145847279683, -32.81649511626806515, 7.761113333117553026 ) ) ;
#30971 = PLANE ( 'NONE',  #23974 ) ;
#30972 = CARTESIAN_POINT ( 'NONE',  ( 2.123740571999295224, -26.18929573040587400, 7.139196562012271485 ) ) ;
#30973 = EDGE_CURVE ( 'NONE', #38905, #37912, #4127, .T. ) ;
#30974 = CARTESIAN_POINT ( 'NONE',  ( 8.290806648384990041, 0.000000000000000000, 6.000000000000000000 ) ) ;
#30975 = CARTESIAN_POINT ( 'NONE',  ( 21.49308418680749710, 7.713898994826276834, 2.801309206857172995 ) ) ;
#30976 = CARTESIAN_POINT ( 'NONE',  ( 23.46066938646308841, 1.523794879705043792, -5.010722692604085537 ) ) ;
#30977 = ORIENTED_EDGE ( 'NONE', *, *, #39984, .F. ) ;
#30978 = EDGE_CURVE ( 'NONE', #26946, #11923, #33542, .T. ) ;
#30979 = EDGE_LOOP ( 'NONE', ( #7506, #25660, #17229, #10937 ) ) ;
#30980 = CARTESIAN_POINT ( 'NONE',  ( 69.72614016916874391, 59.17085620800508394, -3.982895692900132456 ) ) ;
#30981 = EDGE_CURVE ( 'NONE', #20273, #8305, #37941, .T. ) ;
#30982 = EDGE_CURVE ( 'NONE', #35369, #24328, #14558, .T. ) ;
#30983 = VERTEX_POINT ( 'NONE', #30025 ) ;
#30984 = CARTESIAN_POINT ( 'NONE',  ( 87.47409246771869107, -1.962666243356603557, 3.672687813029068771 ) ) ;
#30985 = CARTESIAN_POINT ( 'NONE',  ( 3.121324086407806231, -24.55319635012989110, 6.700000000000000178 ) ) ;
#30986 = CARTESIAN_POINT ( 'NONE',  ( 3.037211893591657219, -26.44376520468768632, 7.013842709614101167 ) ) ;
#30987 = PRODUCT_DEFINITION_SHAPE ( 'NONE', 'NONE',  #11447 ) ;
#30988 = CARTESIAN_POINT ( 'NONE',  ( 4.897206782758049215, -30.72770037511210717, 7.763628509615289275 ) ) ;
#30989 = CONTEXT_DEPENDENT_SHAPE_REPRESENTATION ( #27111, #37447 ) ;
#30990 = CARTESIAN_POINT ( 'NONE',  ( 4.104433119696450305, -25.16239669867571749, 7.754798119455333705 ) ) ;
#30991 = ORIENTED_EDGE ( 'NONE', *, *, #5528, .F. ) ;
#30992 = CARTESIAN_POINT ( 'NONE',  ( 24.07681195139318930, 3.355352448838379242, 3.179409747024673827 ) ) ;
#30993 = CARTESIAN_POINT ( 'NONE',  ( -75.45330471031414277, 33.71485196875532608, -12.49999999999999645 ) ) ;
#30994 = CIRCLE ( 'NONE', #32949, 6.000000000000002665 ) ;
#30995 = EDGE_CURVE ( 'NONE', #10306, #22791, #14929, .T. ) ;
#30996 = EDGE_LOOP ( 'NONE', ( #6579, #17263, #40110, #28657 ) ) ;
#30997 = CARTESIAN_POINT ( 'NONE',  ( 80.23310653198076636, 61.53645999506316855, -2.845586111146968911 ) ) ;
#30998 = CARTESIAN_POINT ( 'NONE',  ( 16.81957533019866702, 9.797912850251352168, -2.500000000000367706 ) ) ;
#30999 = CARTESIAN_POINT ( 'NONE',  ( 80.71114116412915962, 65.59088185864118259, -2.713791510777194382 ) ) ;
#31000 = CARTESIAN_POINT ( 'NONE',  ( 78.59965762292412705, 65.58148208812491475, 2.436540443961506597 ) ) ;
#31001 = ORIENTED_EDGE ( 'NONE', *, *, #21253, .T. ) ;
#31002 = CARTESIAN_POINT ( 'NONE',  ( 4.396048886544873469, -27.49787234876598063, 6.868387053540518927 ) ) ;
#31003 = CARTESIAN_POINT ( 'NONE',  ( 2.834760927471382530, -32.77511392390336908, 7.782167645815904145 ) ) ;
#31004 = CARTESIAN_POINT ( 'NONE',  ( 22.39040353993711108, 2.683735211801196563, -8.168217153243197970 ) ) ;
#31005 = ORIENTED_EDGE ( 'NONE', *, *, #6257, .T. ) ;
#31006 = CARTESIAN_POINT ( 'NONE',  ( -76.09017072707489149, 8.929435588302428783, 8.593849483394778943 ) ) ;
#31007 = CARTESIAN_POINT ( 'NONE',  ( 36.96316948681300119, -3.289061831793972157, 5.933911304578510126 ) ) ;
#31008 = CARTESIAN_POINT ( 'NONE',  ( 1.700390093233090871, -29.56993018339339940, 6.000000000000000000 ) ) ;
#31009 = CARTESIAN_POINT ( 'NONE',  ( -80.96054980827190661, 10.55948373611085778, -0.1886338521618539932 ) ) ;
#31010 = CARTESIAN_POINT ( 'NONE',  ( 30.68921806961705556, -2.925807085693435727, -4.996192719944245297 ) ) ;
#31011 = CARTESIAN_POINT ( 'NONE',  ( 37.18663386580139729, -2.963620350049941177, -6.000007560707241616 ) ) ;
#31012 = CYLINDRICAL_SURFACE ( 'NONE', #26216, 3.399999999999999911 ) ;
#31013 = CARTESIAN_POINT ( 'NONE',  ( 14.79496864341336604, 12.68087409683664823, 2.510197516273051654 ) ) ;
#31014 = CARTESIAN_POINT ( 'NONE',  ( -0.06309262675075595628, -26.54666488804996405, 7.638132480492513920 ) ) ;
#31015 = CARTESIAN_POINT ( 'NONE',  ( 4.313599969017027469, -31.74504722509605159, 7.635761828346577573 ) ) ;
#31016 = B_SPLINE_CURVE_WITH_KNOTS ( 'NONE', 3,
 ( #22151, #18619, #27497, #2407 ),
 .UNSPECIFIED., .F., .F.,
 ( 4, 4 ),
 ( 1.134857258918348999E-18, 6.391136169993800794E-06 ),
 .UNSPECIFIED. ) ;
#31017 = CARTESIAN_POINT ( 'NONE',  ( -28.87867591359218977, -24.55319635012989110, 6.700000000000000178 ) ) ;
#31018 = CARTESIAN_POINT ( 'NONE',  ( 22.01630332033667514, 0.2560055906900143841, -7.605423277453922104 ) ) ;
#31019 = AXIS2_PLACEMENT_3D ( 'NONE', #14224, #39955, #11526 ) ;
#31020 = CARTESIAN_POINT ( 'NONE',  ( 36.85527851974480029, -2.080028804847991353, -5.860598804419308472 ) ) ;
#31021 = CARTESIAN_POINT ( 'NONE',  ( 24.66063408182436945, 2.989447463104236036, -3.506463971955919412 ) ) ;
#31022 = ORIENTED_EDGE ( 'NONE', *, *, #10605, .T. ) ;
#31024 = EDGE_CURVE ( 'NONE', #31748, #11338, #24451, .T. ) ;
#31023 = CARTESIAN_POINT ( 'NONE',  ( 67.01778322055632486, 57.97087264248310134, 3.999241514195644775 ) ) ;
#31025 = CARTESIAN_POINT ( 'NONE',  ( 29.17643449372946307, 0.5759355299653177163, 4.760086256117967984 ) ) ;
#31026 = CARTESIAN_POINT ( 'NONE',  ( 4.974883666185707654, -30.78101102078142048, 7.778495531946297170 ) ) ;
#31027 = EDGE_CURVE ( 'NONE', #17900, #38669, #20638, .T. ) ;
#31028 = FACE_OUTER_BOUND ( 'NONE', #25501, .T. ) ;
#31029 = CARTESIAN_POINT ( 'NONE',  ( 88.66616934308579800, -1.912773240965560673, 2.173515562489431563 ) ) ;
#31031 = CARTESIAN_POINT ( 'NONE',  ( 37.03859629130157316, -3.000568126192123319, -5.987166751730718772 ) ) ;
#31030 = CARTESIAN_POINT ( 'NONE',  ( -71.92837670882107659, -20.78299143688747819, 5.916079783099617906 ) ) ;
#31032 =( BOUNDED_CURVE ( )  B_SPLINE_CURVE ( 3, ( #4170, #26191, #29273, #1085 ),
 .UNSPECIFIED., .F., .T. ) 
 B_SPLINE_CURVE_WITH_KNOTS ( ( 4, 4 ),
 ( 1.347909859412853351, 1.534781240595298302 ),
 .UNSPECIFIED. ) 
 CURVE ( )  GEOMETRIC_REPRESENTATION_ITEM ( )  RATIONAL_B_SPLINE_CURVE ( ( 1.000000000000000000, 0.9970920404276226723, 0.9970920404276226723, 1.000000000000000000 ) ) 
 REPRESENTATION_ITEM ( '' )  );
#31033 = ORIENTED_EDGE ( 'NONE', *, *, #21440, .F. ) ;
#31034 = CARTESIAN_POINT ( 'NONE',  ( 24.73897951283172247, 3.010565050160694422, 3.390208192849414548 ) ) ;
#31035 = EDGE_CURVE ( 'NONE', #22478, #3797, #5726, .T. ) ;
#31036 = CARTESIAN_POINT ( 'NONE',  ( 7.121324086407810228, -26.64985754041175525, 6.800000000000000711 ) ) ;
#31037 = VERTEX_POINT ( 'NONE', #2461 ) ;
#31038 = CARTESIAN_POINT ( 'NONE',  ( -70.50053432363721129, -21.68684479525939324, 5.996770606117007851 ) ) ;
#31039 = ORIENTED_EDGE ( 'NONE', *, *, #25812, .T. ) ;
#31040 = CARTESIAN_POINT ( 'NONE',  ( 79.03702048636715460, 65.49184929578454728, -2.818206040476802343 ) ) ;
#31041 = CARTESIAN_POINT ( 'NONE',  ( 4.894814254439905810, -28.12309771077098830, 7.501983001166816933 ) ) ;
#31042 = CARTESIAN_POINT ( 'NONE',  ( 80.48752863069321961, 62.90068369996134834, 3.525318766974259166 ) ) ;
#31044 = ORIENTED_EDGE ( 'NONE', *, *, #40046, .T. ) ;
#31043 = CARTESIAN_POINT ( 'NONE',  ( -1.340724465380329633, -31.09033463251039464, 6.920489980334475710 ) ) ;
#31045 = CIRCLE ( 'NONE', #18528, 3.499999999999999556 ) ;
#31046 = CARTESIAN_POINT ( 'NONE',  ( 0.02220050038877733126, -26.51254151590686092, 7.782861076432731728 ) ) ;
#31048 = DIRECTION ( 'NONE',  ( 1.000000000000000000, 0.000000000000000000, 0.000000000000000000 ) ) ;
#31047 = CARTESIAN_POINT ( 'NONE',  ( 4.926102704777563623, -30.92815744066947303, 7.009310105710482297 ) ) ;
#31049 = DIRECTION ( 'NONE',  ( -0.000000000000000000, -0.000000000000000000, -1.000000000000000000 ) ) ;
#31050 = CARTESIAN_POINT ( 'NONE',  ( 33.89871771371753084, -5.477042562592300712, 0.06951882857151732431 ) ) ;
#31051 = EDGE_LOOP ( 'NONE', ( #31953, #22281, #19141, #22452 ) ) ;
#31052 = CARTESIAN_POINT ( 'NONE',  ( 5.196299276553091318, -29.73910164073445017, 7.013842709614101167 ) ) ;
#31053 = VECTOR ( 'NONE', #25141, 1000.000000000000000 ) ;
#31054 = CARTESIAN_POINT ( 'NONE',  ( -78.00837106247750796, -5.149560780178712882, -7.068249347921222281 ) ) ;
#31055 = CARTESIAN_POINT ( 'NONE',  ( 5.006679844419255510, -30.36267735696220171, 6.929923840112066635 ) ) ;
#31056 = CARTESIAN_POINT ( 'NONE',  ( 81.34501369141621296, 61.50378551383993653, 1.741375869723579273 ) ) ;
#31057 = CARTESIAN_POINT ( 'NONE',  ( 86.17157777234386629, 0.6269314577163517255, 5.990399513018050293 ) ) ;
#31058 = FACE_OUTER_BOUND ( 'NONE', #2920, .T. ) ;
#31059 = ORIENTED_EDGE ( 'NONE', *, *, #6666, .T. ) ;
#31060 = CARTESIAN_POINT ( 'NONE',  ( -64.08758708074093136, 35.89366350591650701, -3.939604612811969719 ) ) ;
#31061 = CARTESIAN_POINT ( 'NONE',  ( 3.455938198587527044, -26.65821024669467931, 6.880147297696981745 ) ) ;
#31062 = EDGE_CURVE ( 'NONE', #21833, #15683, #33336, .T. ) ;
#31063 = FACE_OUTER_BOUND ( 'NONE', #4393, .T. ) ;
#31064 = EDGE_CURVE ( 'NONE', #36848, #28284, #26738, .T. ) ;
#31065 = CARTESIAN_POINT ( 'NONE',  ( 19.70092807311216987, -3.044756132290810768, -3.216959551844232656 ) ) ;
#31066 = CARTESIAN_POINT ( 'NONE',  ( -64.95171866297674512, 36.28765213650432742, -6.629387290673639299 ) ) ;
#31067 = DIRECTION ( 'NONE',  ( -0.8660254037844399289, 0.000000000000000000, -0.4999999999999977240 ) ) ;
#31068 = CARTESIAN_POINT ( 'NONE',  ( 1.814784800566712653, -26.17185516201231366, 6.864276522220859711 ) ) ;
#31069 = CARTESIAN_POINT ( 'NONE',  ( 33.68728320403869247, -3.101957757517421754, 5.464113292652290177 ) ) ;
#31070 = EDGE_CURVE ( 'NONE', #34839, #39722, #15780, .T. ) ;
#31071 = CARTESIAN_POINT ( 'NONE',  ( 4.265723375214720114, -31.80131207638199697, 7.785172627573962778 ) ) ;
#31072 = EDGE_CURVE ( 'NONE', #21009, #10798, #36203, .T. ) ;
#31073 = CARTESIAN_POINT ( 'NONE',  ( 4.934953675687837382, -28.52226686387824373, 7.754798119455333705 ) ) ;
#31074 = ORIENTED_EDGE ( 'NONE', *, *, #386, .T. ) ;
#31076 = CARTESIAN_POINT ( 'NONE',  ( 14.74006167184663241, -5.120305118510855458, 2.499999999999999556 ) ) ;
#31075 = CARTESIAN_POINT ( 'NONE',  ( 81.23980251882781545, 61.36242252098747940, -1.459100623883069048 ) ) ;
#31077 = CARTESIAN_POINT ( 'NONE',  ( 16.62281228516970799, -3.166379901436700006, 2.800789899971793062 ) ) ;
#31078 = CARTESIAN_POINT ( 'NONE',  ( -69.42837670882107659, -47.11702805680359063, 9.886859966642603581 ) ) ;
#31079 = AXIS2_PLACEMENT_3D ( 'NONE', #25055, #18865, #28336 ) ;
#31080 = ORIENTED_EDGE ( 'NONE', *, *, #22623, .F. ) ;
#31081 = CARTESIAN_POINT ( 'NONE',  ( -2.348748702180637693, -26.64985754041175525, 6.700000000000000178 ) ) ;
#31082 = ORIENTED_EDGE ( 'NONE', *, *, #4793, .F. ) ;
#31083 = VERTEX_POINT ( 'NONE', #33123 ) ;
#31084 = CARTESIAN_POINT ( 'NONE',  ( 81.17684021745370160, 61.76890268566524611, -2.450942308261408353 ) ) ;
#31085 = EDGE_CURVE ( 'NONE', #21319, #28100, #4903, .T. ) ;
#31086 = CARTESIAN_POINT ( 'NONE',  ( -58.93521193748836140, 27.64319143539497148, -6.467610917686843486 ) ) ;
#31087 = ORIENTED_EDGE ( 'NONE', *, *, #37145, .F. ) ;
#31089 = CARTESIAN_POINT ( 'NONE',  ( 4.361733393105681422, -27.45397842585655113, 7.778050822775631978 ) ) ;
#31088 = CARTESIAN_POINT ( 'NONE',  ( 22.24090466686359946, 3.269623998474210591, 4.510814169736189427 ) ) ;
#31090 = EDGE_LOOP ( 'NONE', ( #33771, #3042, #38563, #37649 ) ) ;
#31091 = CARTESIAN_POINT ( 'NONE',  ( 80.77640933968160653, 65.62578451531314272, -2.636331425444868870 ) ) ;
#31092 = LINE ( 'NONE', #18714, #23529 ) ;
#31093 = CARTESIAN_POINT ( 'NONE',  ( 4.727494763369829656, -28.02182252691845576, 6.882085323592684212 ) ) ;
#31095 = PLANE ( 'NONE',  #18353 ) ;
#31094 = CARTESIAN_POINT ( 'NONE',  ( -70.79776717266595654, 0.2170085631123328807, 5.999999999999970690 ) ) ;
#31096 = CARTESIAN_POINT ( 'NONE',  ( -80.92837670882107659, 2.429809908903242555, 12.50000000000000000 ) ) ;
#31097 = CARTESIAN_POINT ( 'NONE',  ( 0.1825688514500733994, -0.6000000000000004219, 3.931742364882332197 ) ) ;
#31098 = CARTESIAN_POINT ( 'NONE',  ( 74.40173173411091057, 59.34324565254589601, 3.478821770173325501 ) ) ;
#31099 = ORIENTED_EDGE ( 'NONE', *, *, #36136, .T. ) ;
#31100 = CARTESIAN_POINT ( 'NONE',  ( 23.27552172775332551, 3.086263684135279295, -3.977210565842318246 ) ) ;
#31101 = ORIENTED_EDGE ( 'NONE', *, *, #13147, .F. ) ;
#31102 = DIRECTION ( 'NONE',  ( -0.000000000000000000, -0.000000000000000000, 1.000000000000000000 ) ) ;
#31103 = CARTESIAN_POINT ( 'NONE',  ( 21.85643539959774273, -7.673977846683588844, 14.52234238348545681 ) ) ;
#31104 = DIRECTION ( 'NONE',  ( -0.000000000000000000, -1.000000000000000000, -0.000000000000000000 ) ) ;
#31105 = ORIENTED_EDGE ( 'NONE', *, *, #25251, .F. ) ;
#31106 = CARTESIAN_POINT ( 'NONE',  ( 81.81758241818920396, 62.27516227682820471, 2.299173245602474935 ) ) ;
#31107 = CARTESIAN_POINT ( 'NONE',  ( 87.92727933775610438, -0.4063688358931643041, -3.816426586085390760 ) ) ;
#31108 = ORIENTED_EDGE ( 'NONE', *, *, #35976, .T. ) ;
#31109 = AXIS2_PLACEMENT_3D ( 'NONE', #40633, #25003, #23326 ) ;
#31110 = CARTESIAN_POINT ( 'NONE',  ( 2.778550765842568104, -32.89974653295162454, 6.867199677474202346 ) ) ;
#31111 = CARTESIAN_POINT ( 'NONE',  ( 23.83988866691774078, -2.865115883751661929, 3.921967457249267319 ) ) ;
#31112 = DIRECTION ( 'NONE',  ( 0.000000000000000000, 1.000000000000000000, 0.000000000000000000 ) ) ;
#31113 = CARTESIAN_POINT ( 'NONE',  ( 36.89759893298676019, -3.003103866610235873, -5.965160703931689845 ) ) ;
#31114 = CARTESIAN_POINT ( 'NONE',  ( 5.141351571375373020, -29.01534782536966617, 7.785344483711592822 ) ) ;
#31115 = CARTESIAN_POINT ( 'NONE',  ( 4.926808446430161581, -28.19584895585300544, 7.139344958878410807 ) ) ;
#31116 = EDGE_CURVE ( 'NONE', #10579, #39042, #18909, .T. ) ;
#31117 = CARTESIAN_POINT ( 'NONE',  ( 21.89888535303197870, 5.088844031853470895, -3.617585142307979673 ) ) ;
#31118 = EDGE_CURVE ( 'NONE', #2581, #31697, #7706, .T. ) ;
#31119 = CARTESIAN_POINT ( 'NONE',  ( -69.58118028693378676, -46.45007417365150815, 5.846929218950453588 ) ) ;
#31120 = ADVANCED_FACE ( 'NONE', ( #18676 ), #19299, .T. ) ;
#31121 = ORIENTED_EDGE ( 'NONE', *, *, #23984, .T. ) ;
#31122 = ORIENTED_EDGE ( 'NONE', *, *, #19112, .F. ) ;
#31123 = CARTESIAN_POINT ( 'NONE',  ( 35.83223476015841413, -3.727955879379408533, 5.624514018808150162 ) ) ;
#31124 = CARTESIAN_POINT ( 'NONE',  ( -71.54962422038506986, 0.008394241410477492477, 5.980324962551074819 ) ) ;
#31125 = CARTESIAN_POINT ( 'NONE',  ( 66.95869957004099149, 58.13407781516350070, -3.995640437668403155 ) ) ;
#31126 = ORIENTED_EDGE ( 'NONE', *, *, #15565, .T. ) ;
#31127 = CARTESIAN_POINT ( 'NONE',  ( 87.98680850476117143, -0.4732348216977415589, -3.104595713354958875 ) ) ;
#31128 = CARTESIAN_POINT ( 'NONE',  ( -74.35246078617609555, 9.035812363374233769, -9.396779859613371144 ) ) ;
#31129 = FACE_OUTER_BOUND ( 'NONE', #5216, .T. ) ;
#31130 = DIRECTION ( 'NONE',  ( 0.000000000000000000, -1.000000000000000000, 0.000000000000000000 ) ) ;
#31131 = VECTOR ( 'NONE', #3758, 1000.000000000000000 ) ;
#31132 = CARTESIAN_POINT ( 'NONE',  ( 3.914573333748507356, -32.28055252020246968, 6.880608371227946662 ) ) ;
#31133 = ORIENTED_EDGE ( 'NONE', *, *, #38854, .F. ) ;
#31134 = CARTESIAN_POINT ( 'NONE',  ( 23.73628397669238055, 3.550931190053107311, 3.214768951104281847 ) ) ;
#31135 = CARTESIAN_POINT ( 'NONE',  ( 78.99916064199128130, 66.21331998952629760, -1.048259027381222008 ) ) ;
#31136 = CARTESIAN_POINT ( 'NONE',  ( 79.01164091803718748, 65.74483092438761389, 2.494286432550486321 ) ) ;
#31137 = DIRECTION ( 'NONE',  ( 1.000000000000000000, 1.090397613471135978E-14, 0.000000000000000000 ) ) ;
#31138 = ORIENTED_EDGE ( 'NONE', *, *, #10830, .F. ) ;
#31139 = CARTESIAN_POINT ( 'NONE',  ( 76.36824339142350482, 62.58715529212016548, -3.801074476319113327 ) ) ;
#31140 =( BOUNDED_CURVE ( )  B_SPLINE_CURVE ( 3, ( #39408, #20272, #38997, #26668 ),
 .UNSPECIFIED., .F., .F. ) 
 B_SPLINE_CURVE_WITH_KNOTS ( ( 4, 4 ),
 ( 1.347909859412855127, 1.534781240595300078 ),
 .UNSPECIFIED. ) 
 CURVE ( )  GEOMETRIC_REPRESENTATION_ITEM ( )  RATIONAL_B_SPLINE_CURVE ( ( 1.000000000000000000, 0.9970920404276226723, 0.9970920404276226723, 1.000000000000000000 ) ) 
 REPRESENTATION_ITEM ( '' )  );
#31142 = CARTESIAN_POINT ( 'NONE',  ( -0.03790328338398483987, -32.60774784362404688, 7.635761828346575797 ) ) ;
#31141 = CARTESIAN_POINT ( 'NONE',  ( 0.03672680498656953618, -25.15737950931636036, 7.695279973900954751 ) ) ;
#31143 = CARTESIAN_POINT ( 'NONE',  ( 14.96406161801628443, 11.85168694806318257, -2.541901741326018982 ) ) ;
#31144 = CARTESIAN_POINT ( 'NONE',  ( 79.20630559137384807, 66.06758606029085001, -1.969816429101940214 ) ) ;
#31145 = CARTESIAN_POINT ( 'NONE',  ( 78.34663729941155452, 61.36874863982431094, 3.480716904142319379 ) ) ;
#31146 = EDGE_LOOP ( 'NONE', ( #30663, #15977, #37589, #3111 ) ) ;
#31147 = ORIENTED_EDGE ( 'NONE', *, *, #4301, .F. ) ;
#31148 = AXIS2_PLACEMENT_3D ( 'NONE', #37525, #21495, #27854 ) ;
#31149 = CARTESIAN_POINT ( 'NONE',  ( 4.744007798040242641, -31.29805785553299557, 7.651421919295144036 ) ) ;
#31150 = CIRCLE ( 'NONE', #10751, 10.00000000000000888 ) ;
#31151 = CARTESIAN_POINT ( 'NONE',  ( -57.69469465617550696, 32.53235267577638723, 4.116732114020066113 ) ) ;
#31152 = CARTESIAN_POINT ( 'NONE',  ( 78.95874065903555561, 66.19121013986816138, 1.203271478923122251 ) ) ;
#31154 = CARTESIAN_POINT ( 'NONE',  ( -1.693770939237457585, -29.37071670600890272, 6.997764925645181933 ) ) ;
#31153 = CARTESIAN_POINT ( 'NONE',  ( -64.08758708074093136, 43.50655619156261622, 1.588711929256377831 ) ) ;
#31155 = CARTESIAN_POINT ( 'NONE',  ( 32.01248540970218670, -4.887874588265229470, -2.123135123820048875 ) ) ;
#31156 = DIRECTION ( 'NONE',  ( 0.000000000000000000, 1.000000000000000000, 0.000000000000000000 ) ) ;
#31157 = CARTESIAN_POINT ( 'NONE',  ( -1.796364496817714818, -29.56936870405388618, 7.767720160662275219 ) ) ;
#31158 = CARTESIAN_POINT ( 'NONE',  ( -64.53809346645429912, 34.68836506924190388, 5.879071147244312456 ) ) ;
#31159 = CARTESIAN_POINT ( 'NONE',  ( 21.79325021498261705, 0.2292132057495366859, -8.345714203105845996 ) ) ;
#31160 = CARTESIAN_POINT ( 'NONE',  ( 1.358827467012312384, -32.95986981511961034, 7.505001789837626447 ) ) ;
#31161 = EDGE_LOOP ( 'NONE', ( #30296, #2787, #6815, #6596 ) ) ;
#31162 = CARTESIAN_POINT ( 'NONE',  ( 1.682951012397970292, -26.06997362959739206, 7.750000000000000888 ) ) ;
#31163 = CARTESIAN_POINT ( 'NONE',  ( 80.84593566081812810, 61.18628925133899799, 1.559654057697081875 ) ) ;
#31164 = DIRECTION ( 'NONE',  ( -0.000000000000000000, -1.000000000000000000, -0.000000000000000000 ) ) ;
#31165 = CARTESIAN_POINT ( 'NONE',  ( 2.140846989427893643, -33.04210496623404225, 7.013842709614101167 ) ) ;
#31166 = CARTESIAN_POINT ( 'NONE',  ( 37.15677058856715576, -2.581106085008523898, -5.983794649111914943 ) ) ;
#31167 = DIRECTION ( 'NONE',  ( 0.000000000000000000, 0.000000000000000000, 1.000000000000000000 ) ) ;
#31168 = CARTESIAN_POINT ( 'NONE',  ( 28.67087680535204797, -4.024283280459782119, 4.110896467804376009 ) ) ;
#31169 = DIRECTION ( 'NONE',  ( -1.000000000000000000, 0.000000000000000000, 0.000000000000000000 ) ) ;
#31170 = FACE_OUTER_BOUND ( 'NONE', #12909, .T. ) ;
#31171 = PLANE ( 'NONE',  #2325 ) ;
#31172 = CARTESIAN_POINT ( 'NONE',  ( 1.674779974442441643, -26.17002453643706517, 7.652160403243383868 ) ) ;
#31173 = CARTESIAN_POINT ( 'NONE',  ( -30.24874870218063450, -25.49307895267003587, 6.700000000000000178 ) ) ;
#31174 = CARTESIAN_POINT ( 'NONE',  ( 2.832035007868547893, -26.36378076803745429, 7.670860738520332234 ) ) ;
#31175 = EDGE_CURVE ( 'NONE', #37024, #22121, #22207, .T. ) ;
#31176 = ORIENTED_EDGE ( 'NONE', *, *, #32503, .F. ) ;
#31177 = DIRECTION ( 'NONE',  ( -0.3420201433256578882, -0.9396926207859123137, 0.000000000000000000 ) ) ;
#31178 = CARTESIAN_POINT ( 'NONE',  ( 70.93434718597480071, 59.50194243796293136, -3.976054184260643609 ) ) ;
#31179 = VECTOR ( 'NONE', #33516, 1000.000000000000000 ) ;
#31180 = ORIENTED_EDGE ( 'NONE', *, *, #1367, .F. ) ;
#31181 = DIRECTION ( 'NONE',  ( 1.000000000000000000, 0.000000000000000000, 0.000000000000000000 ) ) ;
#31182 = DIRECTION ( 'NONE',  ( 0.000000000000000000, 1.000000000000000000, 0.000000000000000000 ) ) ;
#31183 = CARTESIAN_POINT ( 'NONE',  ( 5.033334561780324456, -28.50148930192538543, 6.870724624169668004 ) ) ;
#31184 = CARTESIAN_POINT ( 'NONE',  ( -15.07867591359219439, -26.64985754041175525, 6.800000000000000711 ) ) ;
#31185 = CARTESIAN_POINT ( 'NONE',  ( -29.07867591359219617, -26.64985754041175525, 6.800000000000000711 ) ) ;
#31186 = ORIENTED_EDGE ( 'NONE', *, *, #26330, .F. ) ;
#31187 = CARTESIAN_POINT ( 'NONE',  ( 21.82973510601959788, 5.967885360353585078, 3.133254696524513605 ) ) ;
#31188 = DIRECTION ( 'NONE',  ( 1.000000000000000000, 0.000000000000000000, 0.000000000000000000 ) ) ;
#31189 = VECTOR ( 'NONE', #15673, 1000.000000000000114 ) ;
#31190 = AXIS2_PLACEMENT_3D ( 'NONE', #34403, #12124, #5766 ) ;
#31191 = ORIENTED_EDGE ( 'NONE', *, *, #264, .F. ) ;
#31192 = CARTESIAN_POINT ( 'NONE',  ( 80.45616750117871163, 61.42990784962029949, -2.551437666014049643 ) ) ;
#31193 = CARTESIAN_POINT ( 'NONE',  ( -1.484393579397379259, -30.76037252073963657, 7.661510568013098599 ) ) ;
#31194 = CARTESIAN_POINT ( 'NONE',  ( 80.93893743487447523, 65.34845912995858441, -2.808566127056343564 ) ) ;
#31195 = ADVANCED_FACE ( 'NONE', ( #378 ), #3481, .F. ) ;
#31196 = CARTESIAN_POINT ( 'NONE',  ( 78.76746739705249922, 65.24896075961403596, 2.948506306558721590 ) ) ;
#31197 = CARTESIAN_POINT ( 'NONE',  ( 4.434547210566933018, -27.54894399270960292, 6.969307238440501706 ) ) ;
#31198 = B_SPLINE_SURFACE_WITH_KNOTS ( 'NONE', 5, 3, ( 
 ( #15756, #6087, #22153, #31010, #34725, #34317, #12867 ),
 ( #6504, #5886, #19053, #28310, #2815, #128, #31616 ),
 ( #27894, #18422, #31210, #8950, #2615, #25235, #15134 ),
 ( #3439, #15955, #27690, #12249, #37366, #40246, #12032 ),
 ( #24610, #9162, #3031, #19458, #3839, #28725, #16356 ),
 ( #9780, #34927, #6902, #22362, #25635, #28930, #6705 ),
 ( #32032, #19253, #731, #31822, #3636, #38177, #16161 ),
 ( #537, #13073, #9980, #22559, #35124, #37460, #27997 ) ),
 .UNSPECIFIED., .F., .F., .F.,
 ( 6, 2, 6 ),
 ( 4, 1, 1, 1, 4 ),
 ( 0.000000000000000000, 0.5000000000000000000, 1.000000000000000000 ),
 ( 0.000000000000000000, 0.001659480086290941693, 0.002765800143818236082, 0.004008671076256031980, 0.005388092883604330037 ),
 .UNSPECIFIED. ) ;
#31199 = CARTESIAN_POINT ( 'NONE',  ( 81.88789819931513136, 65.48572365615882518, 1.000000000000000000 ) ) ;
#31200 = CARTESIAN_POINT ( 'NONE',  ( -70.92837670882106238, -48.61702805680358352, 6.000000000000002665 ) ) ;
#31201 = CARTESIAN_POINT ( 'NONE',  ( 22.37440129197860728, 3.331413251109061058, -7.657642981191555620 ) ) ;
#31202 = DIRECTION ( 'NONE',  ( -0.6834397476448861308, 0.000000000000000000, 0.7300069255418706327 ) ) ;
#31203 = ORIENTED_EDGE ( 'NONE', *, *, #3448, .T. ) ;
#31204 = CARTESIAN_POINT ( 'NONE',  ( -75.82730537676935967, 10.26191331253318673, 8.725661018608912300 ) ) ;
#31205 = CARTESIAN_POINT ( 'NONE',  ( 14.61802081865033642, -4.660388157181345470, -2.500000000000000000 ) ) ;
#31206 = EDGE_CURVE ( 'NONE', #6285, #35485, #21787, .T. ) ;
#31207 = CARTESIAN_POINT ( 'NONE',  ( -69.42837670882107659, -47.11702805680359063, 5.809475019311128641 ) ) ;
#31208 = VECTOR ( 'NONE', #9353, 1000.000000000000000 ) ;
#31209 = CARTESIAN_POINT ( 'NONE',  ( 1.578585683582427235, -32.96774767198657941, 7.754798119455333705 ) ) ;
#31210 = CARTESIAN_POINT ( 'NONE',  ( 32.00046961360993691, -3.138592191753610372, -5.200845236069852717 ) ) ;
#31211 = CARTESIAN_POINT ( 'NONE',  ( 35.73199623123087321, -1.301391055416668552, -5.535525800874729008 ) ) ;
#31212 = CARTESIAN_POINT ( 'NONE',  ( 5.551251297819359110, -26.64985754041175525, 6.800000000000000711 ) ) ;
#31213 = CARTESIAN_POINT ( 'NONE',  ( 14.73041858808750426, 13.02581678099233287, 2.501001369465592372 ) ) ;
#31214 = DIRECTION ( 'NONE',  ( 0.3420201433256662704, 0.9396926207859093161, -0.000000000000000000 ) ) ;
#31215 = CARTESIAN_POINT ( 'NONE',  ( -0.02262473055865150268, -26.52342071894167574, 6.894806418505347700 ) ) ;
#31216 = CARTESIAN_POINT ( 'NONE',  ( 5.044365408655546723, -28.95522359424513326, 7.740055089680399902 ) ) ;
#31217 = VECTOR ( 'NONE', #14830, 1000.000000000000000 ) ;
#31218 = CARTESIAN_POINT ( 'NONE',  ( 18.48595909569426610, 13.25013647629958768, -2.499999999999999112 ) ) ;
#31219 = CARTESIAN_POINT ( 'NONE',  ( 21.73669896701832016, 0.3099803614507385396, -8.866688668638362358 ) ) ;
#31220 = FACE_OUTER_BOUND ( 'NONE', #32914, .T. ) ;
#31221 = CARTESIAN_POINT ( 'NONE',  ( 25.67289584648164080, 2.139690751649415024, -4.140607619995577693 ) ) ;
#31222 = EDGE_CURVE ( 'NONE', #31466, #5967, #34165, .T. ) ;
#31223 = ORIENTED_EDGE ( 'NONE', *, *, #22001, .F. ) ;
#31224 = CARTESIAN_POINT ( 'NONE',  ( 66.97346358352143625, 58.09330026553017490, 3.997553359131192696 ) ) ;
#31225 = CARTESIAN_POINT ( 'NONE',  ( 27.44841020286834166, 1.080609055311573252, 4.490386273103699644 ) ) ;
#31226 = FACE_OUTER_BOUND ( 'NONE', #29162, .T. ) ;
#31227 = FACE_OUTER_BOUND ( 'NONE', #40318, .T. ) ;
#31228 = CARTESIAN_POINT ( 'NONE',  ( 85.61248512101352048, 1.464218027013357570, -5.526712519226341769 ) ) ;
#31229 = CARTESIAN_POINT ( 'NONE',  ( 35.95133392841589171, -2.121479879121625167, -5.817473164462794166 ) ) ;
#31230 = ORIENTED_EDGE ( 'NONE', *, *, #8779, .F. ) ;
#31231 = CARTESIAN_POINT ( 'NONE',  ( 24.42333371043659440, 2.822406383138230002, 3.828119244412326427 ) ) ;
#31232 = DIRECTION ( 'NONE',  ( 0.000000000000000000, 0.000000000000000000, 1.000000000000000000 ) ) ;
#31233 = LINE ( 'NONE', #34139, #40357 ) ;
#31234 = EDGE_CURVE ( 'NONE', #1652, #20764, #15807, .T. ) ;
#31235 = ORIENTED_EDGE ( 'NONE', *, *, #6816, .T. ) ;
#31236 = LINE ( 'NONE', #12275, #24173 ) ;
#31237=STYLED_ITEM('',(#40773),#12327);
#31238 = PRODUCT_DEFINITION_CONTEXT ( 'detailed design', #18698, 'design' ) ;
#31239 = AXIS2_PLACEMENT_3D ( 'NONE', #35176, #16010, #28780 ) ;
#31240 = ORIENTED_EDGE ( 'NONE', *, *, #17927, .T. ) ;
#31241 = EDGE_LOOP ( 'NONE', ( #21225, #195, #23967, #11710 ) ) ;
#31242 = CARTESIAN_POINT ( 'NONE',  ( 79.37660656468217724, 64.78470313322911522, -3.432573985763849311 ) ) ;
#31243 = CIRCLE ( 'NONE', #13474, 0.1000000000000028644 ) ;
#31244 = DIRECTION ( 'NONE',  ( -0.000000000000000000, -1.000000000000000000, -0.000000000000000000 ) ) ;
#31245 = CARTESIAN_POINT ( 'NONE',  ( 78.61081429290072720, 65.94468767047428059, 1.703597047176659940 ) ) ;
#31247 = VERTEX_POINT ( 'NONE', #16006 ) ;
#31246 = PLANE ( 'NONE',  #19067 ) ;
#31248 = CIRCLE ( 'NONE', #36490, 2.500000000000002220 ) ;
#31249 = CARTESIAN_POINT ( 'NONE',  ( -58.90952946163269388, 28.52995886935198300, 6.184968675637443347 ) ) ;
#31251 = CARTESIAN_POINT ( 'NONE',  ( -0.7996099067669091287, -29.56993018339339940, -8.199999999999999289 ) ) ;
#31250 = CARTESIAN_POINT ( 'NONE',  ( 4.919044599153583164, -30.94480175767570884, 6.971170733404092879 ) ) ;
#31252 = FACE_OUTER_BOUND ( 'NONE', #34158, .T. ) ;
#31253 = ADVANCED_FACE ( 'NONE', ( #15389 ), #34365, .T. ) ;
#31254 = EDGE_CURVE ( 'NONE', #12078, #27566, #7061, .T. ) ;
#31255 = CARTESIAN_POINT ( 'NONE',  ( -1.748756095191392523, -28.97546355617463121, 7.635761828346576685 ) ) ;
#31256 = CARTESIAN_POINT ( 'NONE',  ( 22.01991341521145173, 5.470200110361999712, -3.165064741469916232 ) ) ;
#31257 = ORIENTED_EDGE ( 'NONE', *, *, #18684, .F. ) ;
#31258 = CARTESIAN_POINT ( 'NONE',  ( -54.01549048184568846, -30.38627270959228710, -4.152976064860135708 ) ) ;
#31259 = ADVANCED_FACE ( 'NONE', ( #12299 ), #38026, .T. ) ;
#31260 = CARTESIAN_POINT ( 'NONE',  ( 25.48218379196744721, -4.266488024150952185, 3.117641769822204090 ) ) ;
#31261 = CARTESIAN_POINT ( 'NONE',  ( -80.83477924395624825, -5.699948517445438512, -1.424373511022223537 ) ) ;
#31262 = CARTESIAN_POINT ( 'NONE',  ( 5.008393135667492224, -30.35550703842281806, 6.997764925645181933 ) ) ;
#31263 = CARTESIAN_POINT ( 'NONE',  ( 81.29658979812207065, 62.90761208998647902, 3.189931650267155749 ) ) ;
#31264 = CARTESIAN_POINT ( 'NONE',  ( 84.21289197705223728, 3.045783863710543660, -0.4930364517660317802 ) ) ;
#31265 = DIRECTION ( 'NONE',  ( -0.000000000000000000, -0.000000000000000000, 1.000000000000000000 ) ) ;
#31266 = EDGE_LOOP ( 'NONE', ( #6730, #9202, #4637, #29595 ) ) ;
#31267 = CARTESIAN_POINT ( 'NONE',  ( -69.08758708074093136, 36.88538962427716683, 8.800414904976364028 ) ) ;
#31268 = CARTESIAN_POINT ( 'NONE',  ( 17.49771952580762502, -6.259504178003650665, -2.500000000000000444 ) ) ;
#31269 = AXIS2_PLACEMENT_3D ( 'NONE', #12094, #24671, #37223 ) ;
#31270 = CARTESIAN_POINT ( 'NONE',  ( 4.092117021882133443, -27.01461099462299131, 6.931070083220558509 ) ) ;
#31271 = CARTESIAN_POINT ( 'NONE',  ( -68.71186372058383540, 37.81212149306784909, -9.800414904976365804 ) ) ;
#31272 = CARTESIAN_POINT ( 'NONE',  ( 85.64493543437410494, 0.8953488218558967038, 5.847730123973997607 ) ) ;
#31273 =( BOUNDED_CURVE ( )  B_SPLINE_CURVE ( 3, ( #24436, #2649, #36995, #24644 ),
 .UNSPECIFIED., .F., .T. ) 
 B_SPLINE_CURVE_WITH_KNOTS ( ( 4, 4 ),
 ( 4.712388980384689674, 4.895802057644187855 ),
 .UNSPECIFIED. ) 
 CURVE ( )  GEOMETRIC_REPRESENTATION_ITEM ( )  RATIONAL_B_SPLINE_CURVE ( ( 1.000000000000000000, 0.9971986010846199955, 0.9971986010846199955, 1.000000000000000000 ) ) 
 REPRESENTATION_ITEM ( '' )  );
#31274 = CARTESIAN_POINT ( 'NONE',  ( 34.92925997322895881, -1.710623459408137759, 5.657953804803885767 ) ) ;
#31275 = AXIS2_PLACEMENT_3D ( 'NONE', #34335, #6106, #18642 ) ;
#31276 = CARTESIAN_POINT ( 'NONE',  ( 1.128064129311358244, -33.02281926226938680, 7.695279973900954751 ) ) ;
#31277 = ORIENTED_EDGE ( 'NONE', *, *, #24649, .T. ) ;
#31279 = CARTESIAN_POINT ( 'NONE',  ( -71.92837670882107659, -0.7829914368874778541, 5.916079783099620570 ) ) ;
#31278 = CARTESIAN_POINT ( 'NONE',  ( 81.21493646480149664, 62.54560775605910550, -3.083955809406642601 ) ) ;
#31280 = CARTESIAN_POINT ( 'NONE',  ( 2.913938899263716742, -32.85281041678479141, 7.640616322432100205 ) ) ;
#31281 = CARTESIAN_POINT ( 'NONE',  ( -2.512351830342552717, -31.78256350185187884, 6.894806418505347700 ) ) ;
#31282 = VERTEX_POINT ( 'NONE', #6749 ) ;
#31283 = CARTESIAN_POINT ( 'NONE',  ( 1.651251297819358754, -26.64985754041175525, 6.700000000000000178 ) ) ;
#31284 = EDGE_CURVE ( 'NONE', #9806, #14269, #18744, .T. ) ;
#31285 = ORIENTED_EDGE ( 'NONE', *, *, #14775, .F. ) ;
#31286 = CARTESIAN_POINT ( 'NONE',  ( 6.921324086407803833, -26.64985754041175525, 6.800000000000000711 ) ) ;
#31287 = EDGE_LOOP ( 'NONE', ( #2701, #35421, #24948, #6776 ) ) ;
#31288 = CARTESIAN_POINT ( 'NONE',  ( 80.20530801487242911, 63.82446735998111365, -3.674973878998262666 ) ) ;
#31289 = CARTESIAN_POINT ( 'NONE',  ( -1.506673198718692985, -28.44088410562211067, 7.692469944509197077 ) ) ;
#31290 = ORIENTED_EDGE ( 'NONE', *, *, #34809, .T. ) ;
#31292 = DIRECTION ( 'NONE',  ( 0.000000000000000000, 0.000000000000000000, -1.000000000000000000 ) ) ;
#31291 = CARTESIAN_POINT ( 'NONE',  ( 24.63348758885817702, 2.687559539024136246, 3.900614856717827816 ) ) ;
#31293 = ORIENTED_EDGE ( 'NONE', *, *, #12675, .T. ) ;
#31294 = EDGE_CURVE ( 'NONE', #38704, #12271, #28536, .T. ) ;
#31295 = CARTESIAN_POINT ( 'NONE',  ( 81.07711124303935435, 65.42186869171261776, -2.645340681430279339 ) ) ;
#31296 = AXIS2_PLACEMENT_3D ( 'NONE', #12171, #5806, #14848 ) ;
#31297 = EDGE_CURVE ( 'NONE', #36016, #10099, #8380, .T. ) ;
#31298 = CARTESIAN_POINT ( 'NONE',  ( 4.719422864845836507, -28.00610904475917806, 6.871394612369934762 ) ) ;
#31300 = LINE ( 'NONE', #3122, #24263 ) ;
#31299 = DIRECTION ( 'NONE',  ( 1.000000000000000000, 0.000000000000000000, 0.000000000000000000 ) ) ;
#31301 = CARTESIAN_POINT ( 'NONE',  ( -18.87867591359219333, -26.64985754041175525, 6.700000000000000178 ) ) ;
#31302 = CARTESIAN_POINT ( 'NONE',  ( 0.5049572051612778445, -26.28386366117923245, 7.767720160662275219 ) ) ;
#31303 = CARTESIAN_POINT ( 'NONE',  ( 73.73614897715009420, 59.29615633563123822, 3.619654763491260585 ) ) ;
#31304 = CARTESIAN_POINT ( 'NONE',  ( 22.62432447131647706, 3.405416539215757599, -4.114152520097174914 ) ) ;
#31305 = VECTOR ( 'NONE', #25381, 1000.000000000000000 ) ;
#31306 = EDGE_CURVE ( 'NONE', #16841, #34783, #16954, .T. ) ;
#31307 = CARTESIAN_POINT ( 'NONE',  ( 21.85643539959776760, -14.20048109512665135, 6.697783101734796851 ) ) ;
#31308 = CARTESIAN_POINT ( 'NONE',  ( 17.09215160921039356, 14.51084972821218599, 1.912535534561743411 ) ) ;
#31309 = ORIENTED_EDGE ( 'NONE', *, *, #23744, .F. ) ;
#31310 = CARTESIAN_POINT ( 'NONE',  ( -38.87867591359218977, -26.64985754041175525, 6.800000000000000711 ) ) ;
#31311 = CARTESIAN_POINT ( 'NONE',  ( 78.68779346184201984, 66.05675297672225099, 1.054034669007998026 ) ) ;
#31312 = CARTESIAN_POINT ( 'NONE',  ( 86.21492201224262431, 1.517032185505227559, -5.007191195300914721 ) ) ;
#31313 = ORIENTED_EDGE ( 'NONE', *, *, #17606, .T. ) ;
#31314 = CARTESIAN_POINT ( 'NONE',  ( 14.61802081865033642, 12.33286846116140190, 2.500000000000000000 ) ) ;
#31315 = ORIENTED_EDGE ( 'NONE', *, *, #32486, .T. ) ;
#31316 = CARTESIAN_POINT ( 'NONE',  ( 33.94523891240480395, -3.271630530324667774, 5.504373519622959954 ) ) ;
#31317 = EDGE_CURVE ( 'NONE', #36530, #26219, #17634, .T. ) ;
#31318 = CARTESIAN_POINT ( 'NONE',  ( 33.62927951164961371, -1.227240062974174650, -5.455060413628188165 ) ) ;
#31319 = CARTESIAN_POINT ( 'NONE',  ( 5.143269691484856132, -28.97182734739054411, 7.773839561854633651 ) ) ;
#31320 = CARTESIAN_POINT ( 'NONE',  ( -20.44874870218064444, -25.49307895267003587, 6.700000000000000178 ) ) ;
#31321 = VERTEX_POINT ( 'NONE', #27736 ) ;
#31322 = DIRECTION ( 'NONE',  ( 1.000000000000000000, 0.000000000000000000, -0.000000000000000000 ) ) ;
#31323 = VERTEX_POINT ( 'NONE', #11870 ) ;
#31324 = ORIENTED_EDGE ( 'NONE', *, *, #30174, .T. ) ;
#31325 = CARTESIAN_POINT ( 'NONE',  ( 27.81551784075586298, 1.843619295897225285, 3.908845422569096950 ) ) ;
#31326 = CARTESIAN_POINT ( 'NONE',  ( 0.9943839796752991234, -25.86893018339336692, 6.954324564059724878 ) ) ;
#31327=STYLED_ITEM('',(#40766),#39462);
#31328 = ORIENTED_EDGE ( 'NONE', *, *, #4112, .T. ) ;
#31329 = CARTESIAN_POINT ( 'NONE',  ( 66.43187891275414358, 57.76301247919344206, -4.000000000000007994 ) ) ;
#31330 = VERTEX_POINT ( 'NONE', #26928 ) ;
#31331 = CARTESIAN_POINT ( 'NONE',  ( -57.97698207090199674, 31.94645990616745834, 4.307980060361010999 ) ) ;
#31332 = CARTESIAN_POINT ( 'NONE',  ( -74.64083662667529495, 9.321351725019315637, -9.286628282490790198 ) ) ;
#31333 = DIRECTION ( 'NONE',  ( -1.000000000000000000, -0.000000000000000000, -0.000000000000000000 ) ) ;
#31334 = VECTOR ( 'NONE', #30075, 1000.000000000000000 ) ;
#31335 = FACE_BOUND ( 'NONE', #19764, .T. ) ;
#31336 = DIRECTION ( 'NONE',  ( -1.000000000000000000, -1.165409145176969993E-16, 0.000000000000000000 ) ) ;
#31337 = ORIENTED_EDGE ( 'NONE', *, *, #37321, .F. ) ;
#31338 = CARTESIAN_POINT ( 'NONE',  ( 22.19901381586180023, 5.214777149643200715, 3.111044880889567210 ) ) ;
#31339 = CARTESIAN_POINT ( 'NONE',  ( 82.13789946638775064, 62.20769933019765574, -1.398807481800598662 ) ) ;
#31340 = CARTESIAN_POINT ( 'NONE',  ( 79.60112097352363492, 64.95058993122677293, 3.372125408468117591 ) ) ;
#31341 = CARTESIAN_POINT ( 'NONE',  ( 2.830618245060743554, -26.36328231767235764, 7.712764235869106422 ) ) ;
#31342 = ORIENTED_EDGE ( 'NONE', *, *, #13349, .F. ) ;
#31343 = CARTESIAN_POINT ( 'NONE',  ( 76.81167355577591138, 60.15069890908841899, -3.230144225296931904 ) ) ;
#31345 = DIRECTION ( 'NONE',  ( -0.000000000000000000, -0.000000000000000000, 1.000000000000000000 ) ) ;
#31344 = CARTESIAN_POINT ( 'NONE',  ( -71.68163889809667921, -45.81621559017686707, 5.953091488286674782 ) ) ;
#31346 = CARTESIAN_POINT ( 'NONE',  ( 14.92465469600171524, 12.09808818448366807, -2.535751338085821427 ) ) ;
#31347 = CARTESIAN_POINT ( 'NONE',  ( 81.15350626233055209, 61.29809656771022475, -1.122020883098639565 ) ) ;
#31348 = CARTESIAN_POINT ( 'NONE',  ( 76.75621762107158474, 64.55157797518404550, 2.701592190110927216 ) ) ;
#31349 = VERTEX_POINT ( 'NONE', #30853 ) ;
#31350 = EDGE_CURVE ( 'NONE', #30840, #6772, #20955, .T. ) ;
#31351 = EDGE_CURVE ( 'NONE', #24034, #33766, #18678, .T. ) ;
#31352 = LINE ( 'NONE', #31556, #27342 ) ;
#31353 = ADVANCED_FACE ( 'NONE', ( #27129 ), #5512, .T. ) ;
#31354 = CARTESIAN_POINT ( 'NONE',  ( 0.5370264050447969284, -32.87092774913090665, 7.700536657684211583 ) ) ;
#31355 = CARTESIAN_POINT ( 'NONE',  ( 81.41819469040454749, 65.60226997055954712, 2.078018481492983405 ) ) ;
#31357 = CARTESIAN_POINT ( 'NONE',  ( -1.699184788179541439, -29.51609423590135606, 6.889465824494257262 ) ) ;
#31356 = CARTESIAN_POINT ( 'NONE',  ( 4.268313344242012697, -31.94811734417107019, 7.011627023500183853 ) ) ;
#31358 = CARTESIAN_POINT ( 'NONE',  ( 29.60215801812428182, 1.109421360397880862, -4.380391640306282142 ) ) ;
#31359 = AXIS2_PLACEMENT_3D ( 'NONE', #3306, #18700, #3100 ) ;
#31360 = DIRECTION ( 'NONE',  ( 1.000000000000000000, 0.000000000000000000, 0.000000000000000000 ) ) ;
#31361 = AXIS2_PLACEMENT_3D ( 'NONE', #4674, #1208, #17209 ) ;
#31362 = CARTESIAN_POINT ( 'NONE',  ( -62.81463675898083210, 36.67811266762162603, -4.600311178732273021 ) ) ;
#31363 = CARTESIAN_POINT ( 'NONE',  ( 1.512219044453454675, -33.06486818805116457, 6.980586498568970732 ) ) ;
#31364 = AXIS2_PLACEMENT_3D ( 'NONE', #32281, #32083, #4081 ) ;
#31365 = CARTESIAN_POINT ( 'NONE',  ( -71.92837670882106238, -42.87473357531881391, -1.732050807568860318 ) ) ;
#31366 = CARTESIAN_POINT ( 'NONE',  ( -0.6392939734488634063, -32.03688751340837371, 6.929923840112063083 ) ) ;
#31367 = CARTESIAN_POINT ( 'NONE',  ( 5.189197560432777578, -29.24685097578066006, 7.566278858797852003 ) ) ;
#31368 = CARTESIAN_POINT ( 'NONE',  ( 32.00275383920578065, 0.1412686694384412134, -4.903342167364729498 ) ) ;
#31369 = LINE ( 'NONE', #12617, #20018 ) ;
#31370 = CARTESIAN_POINT ( 'NONE',  ( -0.9766862336921242616, -31.66594123770981284, 7.761597726988848756 ) ) ;
#31371 = CARTESIAN_POINT ( 'NONE',  ( -72.45330471031414277, 33.71485196875532608, 15.50000000000000000 ) ) ;
#31372 = LINE ( 'NONE', #5640, #27925 ) ;
#31373 = CARTESIAN_POINT ( 'NONE',  ( 87.20660408302002509, 0.2574974038930863407, -5.635807106906071340 ) ) ;
#31374 = CARTESIAN_POINT ( 'NONE',  ( 21.87459114891373702, -13.50524245770412257, 2.500000000000000444 ) ) ;
#31375 = CARTESIAN_POINT ( 'NONE',  ( -1.531881223433573025, -30.62464442689916666, 6.864276522220859711 ) ) ;
#31376 = ORIENTED_EDGE ( 'NONE', *, *, #4554, .F. ) ;
#31377 = VERTEX_POINT ( 'NONE', #24447 ) ;
#31378 = CARTESIAN_POINT ( 'NONE',  ( 68.71160781503239434, 58.33825098880495119, -3.980709302925372839 ) ) ;
#31379 = CARTESIAN_POINT ( 'NONE',  ( 2.940766276717598160, -26.29708008006877407, 6.880608371227951103 ) ) ;
#31380 = VECTOR ( 'NONE', #12352, 1000.000000000000000 ) ;
#31381 = ORIENTED_EDGE ( 'NONE', *, *, #30293, .F. ) ;
#31382 = CARTESIAN_POINT ( 'NONE',  ( -0.9416808278050282643, -27.29637960496864935, 7.785096263473211486 ) ) ;
#31383 = DIRECTION ( 'NONE',  ( -3.491481338843133750E-15, 1.000000000000000000, -0.000000000000000000 ) ) ;
#31384 =( BOUNDED_CURVE ( )  B_SPLINE_CURVE ( 3, ( #10661, #13961, #26528, #39062 ),
 .UNSPECIFIED., .F., .T. ) 
 B_SPLINE_CURVE_WITH_KNOTS ( ( 4, 4 ),
 ( 4.708531083176469068, 4.895802057644189631 ),
 .UNSPECIFIED. ) 
 CURVE ( )  GEOMETRIC_REPRESENTATION_ITEM ( )  RATIONAL_B_SPLINE_CURVE ( ( 1.000000000000000000, 0.9970795998553221295, 0.9970795998553221295, 1.000000000000000000 ) ) 
 REPRESENTATION_ITEM ( '' )  );
#31385 =( GEOMETRIC_REPRESENTATION_CONTEXT ( 3 ) GLOBAL_UNCERTAINTY_ASSIGNED_CONTEXT ( ( #34545 ) ) GLOBAL_UNIT_ASSIGNED_CONTEXT ( ( #32553, #23665, #26372 ) ) REPRESENTATION_CONTEXT ( 'NONE', 'WORKASPACE' ) );
#31386 = CARTESIAN_POINT ( 'NONE',  ( 4.891521542694104774, -30.74327958826899732, 7.775108481317163367 ) ) ;
#31387 = DIRECTION ( 'NONE',  ( 0.7126435865141239612, 0.000000000000000000, 0.7015262779114451730 ) ) ;
#31388 = ORIENTED_EDGE ( 'NONE', *, *, #31680, .T. ) ;
#31389 = CARTESIAN_POINT ( 'NONE',  ( 24.06887988145387069, 3.350337168359989626, 3.200280518033681521 ) ) ;
#31390 = FACE_OUTER_BOUND ( 'NONE', #6614, .T. ) ;
#31391 = DIRECTION ( 'NONE',  ( 1.000000000000000000, 0.000000000000000000, 0.000000000000000000 ) ) ;
#31392 = VERTEX_POINT ( 'NONE', #8172 ) ;
#31393 = CARTESIAN_POINT ( 'NONE',  ( 78.40460260197330911, 65.77602943765538157, -1.910479420724411570 ) ) ;
#31395 = CARTESIAN_POINT ( 'NONE',  ( -1.482122867364318530, -30.76642976786031980, 7.691066658568948000 ) ) ;
#31394 = CARTESIAN_POINT ( 'NONE',  ( 24.12588890033682887, 0.5212924738780745360, 5.092295861883279429 ) ) ;
#31396 = CARTESIAN_POINT ( 'NONE',  ( 81.12957769509920070, 64.69578868775869296, -3.179853676209053237 ) ) ;
#31397 = CARTESIAN_POINT ( 'NONE',  ( 79.70629046221083058, 63.56464109829104814, 3.738478073092014853 ) ) ;
#31398 = ORIENTED_EDGE ( 'NONE', *, *, #38798, .F. ) ;
#31399 = EDGE_CURVE ( 'NONE', #7610, #35491, #17393, .T. ) ;
#31400 = CARTESIAN_POINT ( 'NONE',  ( 4.428520246153464512, -27.54081190378528277, 6.997764925645178380 ) ) ;
#31401 = EDGE_CURVE ( 'NONE', #30749, #19738, #21881, .T. ) ;
#31402 = FACE_OUTER_BOUND ( 'NONE', #2796, .T. ) ;
#31403 = CARTESIAN_POINT ( 'NONE',  ( 2.796830827761068949, -32.78830227222591986, 7.784476445165072533 ) ) ;
#31404 = CARTESIAN_POINT ( 'NONE',  ( 21.85643539959776049, -11.26069278398387929, -1.499473835228683383 ) ) ;
#31405 = CARTESIAN_POINT ( 'NONE',  ( -18.87867591359219333, -26.64985754041175525, 6.700000000000000178 ) ) ;
#31406 = VERTEX_POINT ( 'NONE', #14760 ) ;
#31407 = CARTESIAN_POINT ( 'NONE',  ( -73.10008652833232645, 0.2745614453624863338, 10.93886590303131534 ) ) ;
#31408 = DIRECTION ( 'NONE',  ( -0.000000000000000000, -0.000000000000000000, 1.000000000000000000 ) ) ;
#31409 = DIRECTION ( 'NONE',  ( -0.3420201433256601087, -0.9396926207859114255, -0.000000000000000000 ) ) ;
#31410 = CARTESIAN_POINT ( 'NONE',  ( -11.81496944966682960, -21.25669541281728669, 1.000000000000000000 ) ) ;
#31411 = DIRECTION ( 'NONE',  ( 1.000000000000000000, -8.959828616340678715E-16, 0.000000000000000000 ) ) ;
#31412 = CARTESIAN_POINT ( 'NONE',  ( 33.68500911095676997, -3.840374874697897845, -5.137585959034770333 ) ) ;
#31413 = CARTESIAN_POINT ( 'NONE',  ( -1.560256750498681289, -30.53335229257609384, 6.959317978105168834 ) ) ;
#31414 = CARTESIAN_POINT ( 'NONE',  ( 3.750629725403504366, -32.28222025834440245, 6.882085323592688653 ) ) ;
#31415 = CARTESIAN_POINT ( 'NONE',  ( 20.61347566090116246, 6.036182562928900985, 3.423629434313151698 ) ) ;
#31416 = DIRECTION ( 'NONE',  ( 0.9267318687906785923, -0.3757233601570932335, 0.000000000000000000 ) ) ;
#31417 = DIRECTION ( 'NONE',  ( 0.7660444431189857850, -0.6427876096865299260, -0.000000000000000000 ) ) ;
#31418 = EDGE_CURVE ( 'NONE', #39042, #21520, #28850, .T. ) ;
#31419 = FACE_OUTER_BOUND ( 'NONE', #4736, .T. ) ;
#31420 = VECTOR ( 'NONE', #30266, 1000.000000000000000 ) ;
#31421 = AXIS2_PLACEMENT_3D ( 'NONE', #34092, #33675, #36947 ) ;
#31422 = CARTESIAN_POINT ( 'NONE',  ( 3.911174477942264804, -32.15303813520912257, 7.670860738520331346 ) ) ;
#31423 = CARTESIAN_POINT ( 'NONE',  ( 25.52861145932945064, 1.274360088752857889, -4.422354827559902724 ) ) ;
#31424 = CARTESIAN_POINT ( 'NONE',  ( 30.92600629254716793, -3.767230967968932198, -4.587853941829935778 ) ) ;
#31425 = CARTESIAN_POINT ( 'NONE',  ( 26.61111181199286335, 1.629400868845519490, -4.332867922176739661 ) ) ;
#31426 = ORIENTED_EDGE ( 'NONE', *, *, #29643, .F. ) ;
#31427 = ORIENTED_EDGE ( 'NONE', *, *, #10369, .T. ) ;
#31428 = CARTESIAN_POINT ( 'NONE',  ( 67.05223802139354916, 57.87567627276845883, 3.996315564296190725 ) ) ;
#31429 = CARTESIAN_POINT ( 'NONE',  ( 37.11163797912877271, -2.778243138683350821, 5.998008405196137538 ) ) ;
#31430 = EDGE_CURVE ( 'NONE', #25231, #2110, #598, .T. ) ;
#31431 = CARTESIAN_POINT ( 'NONE',  ( -51.01549048184568846, -30.38627270959228710, 6.000000000000000000 ) ) ;
#31432 = B_SPLINE_CURVE_WITH_KNOTS ( 'NONE', 3,
 ( #24861, #161, #3671, #15797, #12902, #25468, #15990, #37401, #28761, #9397, #34765, #5921, #6125, #572, #31249, #3273, #2854, #8989, #6539, #21574, #3070, #15375, #34560, #3468 ),
 .UNSPECIFIED., .F., .F.,
 ( 4, 2, 2, 2, 2, 2, 2, 2, 2, 2, 2, 4 ),
 ( 0.000000000000000000, 0.0006665208131132561780, 0.001333041626226512356, 0.001999562439339766691, 0.002666083252453021243, 0.003999124878679529912, 0.004332385285236159574, 0.004665645691792788367, 0.004832275895071106234, 0.004998906098349424100, 0.005165536301627741099, 0.005332166504906058965 ),
 .UNSPECIFIED. ) ;
#31433 = CARTESIAN_POINT ( 'NONE',  ( 84.36655727669636917, 3.025886916471207222, -1.294691096651311435 ) ) ;
#31434 = CARTESIAN_POINT ( 'NONE',  ( 36.00510628997864870, -3.152656186843009412, -5.825865641974139031 ) ) ;
#31435 = ORIENTED_EDGE ( 'NONE', *, *, #7592, .F. ) ;
#31436 = CARTESIAN_POINT ( 'NONE',  ( 24.71170268252853930, 2.643186313627579054, 3.922093749847886723 ) ) ;
#31437 = DIRECTION ( 'NONE',  ( -0.000000000000000000, -0.000000000000000000, -1.000000000000000000 ) ) ;
#31438 = CARTESIAN_POINT ( 'NONE',  ( 37.19747295490952155, -2.841588721108153415, -5.999818660317219887 ) ) ;
#31439 = ORIENTED_EDGE ( 'NONE', *, *, #28208, .F. ) ;
#31440 = CARTESIAN_POINT ( 'NONE',  ( -38.24874870218063450, -25.49307895267003587, 6.700000000000000178 ) ) ;
#31441 = EDGE_CURVE ( 'NONE', #5140, #6584, #8786, .T. ) ;
#31442 = VECTOR ( 'NONE', #11168, 1000.000000000000000 ) ;
#31443 = ORIENTED_EDGE ( 'NONE', *, *, #215, .F. ) ;
#31444 = CARTESIAN_POINT ( 'NONE',  ( 80.54480326438822146, 62.60292565479354465, -3.426353657592656976 ) ) ;
#31445 = CARTESIAN_POINT ( 'NONE',  ( -1.727331447465891401, -28.92962485930595662, 7.783750581861600182 ) ) ;
#31446 = CARTESIAN_POINT ( 'NONE',  ( 78.52594532581824183, 65.94185624388921951, 1.429680343938493081 ) ) ;
#31449 = ORIENTED_EDGE ( 'NONE', *, *, #31317, .T. ) ;
#31448 = EDGE_LOOP ( 'NONE', ( #5689, #1929, #35949, #38599 ) ) ;
#31447 = CARTESIAN_POINT ( 'NONE',  ( 14.62858089720432631, 12.62725169013283377, 2.500000000000000000 ) ) ;
#31450 = CARTESIAN_POINT ( 'NONE',  ( 0.05244770176878708196, -26.48311302728685490, 7.761113333116790081 ) ) ;
#31451 = EDGE_CURVE ( 'NONE', #38171, #2784, #24656, .T. ) ;
#31452 = CARTESIAN_POINT ( 'NONE',  ( 27.27118286198125574, -4.471745766876631833, 3.644977776233934819 ) ) ;
#31453 = CARTESIAN_POINT ( 'NONE',  ( 5.654615132425274027, -32.90554535662791835, 7.635761828346577573 ) ) ;
#31454 = CARTESIAN_POINT ( 'NONE',  ( -41.07867591359219972, -26.64985754041175525, 6.700000000000000178 ) ) ;
#31455 = CARTESIAN_POINT ( 'NONE',  ( 24.38063191036968647, 3.152000527247066142, -3.325049431601771133 ) ) ;
#31456 = ORIENTED_EDGE ( 'NONE', *, *, #30022, .F. ) ;
#31457 = CARTESIAN_POINT ( 'NONE',  ( -20.97867591359219475, -26.64985754041175525, 6.700000000000000178 ) ) ;
#31458 = ORIENTED_EDGE ( 'NONE', *, *, #7328, .T. ) ;
#31459 = CARTESIAN_POINT ( 'NONE',  ( 4.954463893073100422, -28.58453498085037836, 7.013842709614101167 ) ) ;
#31460 = CARTESIAN_POINT ( 'NONE',  ( -29.07867591359219617, -26.64985754041175525, 6.700000000000000178 ) ) ;
#31461 = CARTESIAN_POINT ( 'NONE',  ( -81.48936617853665609, -5.631775123504498382, -2.862016309434455952 ) ) ;
#31462 = CARTESIAN_POINT ( 'NONE',  ( 5.006040973414683570, -30.36534187942935148, 6.939395833800443114 ) ) ;
#31463 = CARTESIAN_POINT ( 'NONE',  ( 78.80232334588868071, 66.09893194982535647, 1.428845309148514486 ) ) ;
#31464 = CARTESIAN_POINT ( 'NONE',  ( 87.78960583812504126, -2.347739977990699778, 2.116702103816012759 ) ) ;
#31465 = CARTESIAN_POINT ( 'NONE',  ( 24.97740817842744221, 3.110183573126763079, -2.920139942405988620 ) ) ;
#31466 = VERTEX_POINT ( 'NONE', #17848 ) ;
#31467 = CARTESIAN_POINT ( 'NONE',  ( -42.83131703149249603, -27.06993018339339585, 6.800000000000000711 ) ) ;
#31468 = LINE ( 'NONE', #180, #5801 ) ;
#31470 = ADVANCED_FACE ( 'NONE', ( #17642 ), #30222, .T. ) ;
#31469 = ORIENTED_EDGE ( 'NONE', *, *, #6540, .F. ) ;
#31471 = CARTESIAN_POINT ( 'NONE',  ( -32.87867591359218977, -26.64985754041175525, 6.800000000000000711 ) ) ;
#31472 = CARTESIAN_POINT ( 'NONE',  ( -1.624655799086301533, -28.85995144147929992, 7.754798119455333705 ) ) ;
#31473 = CARTESIAN_POINT ( 'NONE',  ( 4.703888560603170177, -27.97650715214728123, 7.754798119455333705 ) ) ;
#31474 = FACE_OUTER_BOUND ( 'NONE', #38417, .T. ) ;
#31475 = ORIENTED_EDGE ( 'NONE', *, *, #1157, .T. ) ;
#31476 = CARTESIAN_POINT ( 'NONE',  ( 33.62750157612018143, -1.232156386184390495, 5.454782923789285753 ) ) ;
#31477 = AXIS2_PLACEMENT_3D ( 'NONE', #23748, #10583, #23356 ) ;
#31478 = CARTESIAN_POINT ( 'NONE',  ( 85.63852691662546590, 2.164466514264067332, 3.769402685279828358 ) ) ;
#31479 = EDGE_LOOP ( 'NONE', ( #33476, #5031, #5116 ) ) ;
#31481 = CARTESIAN_POINT ( 'NONE',  ( -22.44874870218064089, -26.64985754041175525, 6.800000000000000711 ) ) ;
#31480 = CARTESIAN_POINT ( 'NONE',  ( 81.23328907848382130, 61.46306935600725296, -1.830101370957703200 ) ) ;
#31482 = ADVANCED_FACE ( 'NONE', ( #36802 ), #14979, .F. ) ;
#31483 = DIRECTION ( 'NONE',  ( 0.000000000000000000, -0.000000000000000000, -1.000000000000000000 ) ) ;
#31484 = ORIENTED_EDGE ( 'NONE', *, *, #31399, .T. ) ;
#31485 = EDGE_CURVE ( 'NONE', #18407, #33448, #28769, .T. ) ;
#31486 = CARTESIAN_POINT ( 'NONE',  ( 24.89525126181291981, -5.810506762332490638, -2.873249729385407125 ) ) ;
#31487 = ORIENTED_EDGE ( 'NONE', *, *, #36633, .T. ) ;
#31488 = CARTESIAN_POINT ( 'NONE',  ( -79.12200251776535254, -6.600066278497241257, 5.748117179618010830 ) ) ;
#31489 = ORIENTED_EDGE ( 'NONE', *, *, #6829, .F. ) ;
#31490 = CARTESIAN_POINT ( 'NONE',  ( 80.85530923529172753, 62.40557805022640991, -3.206617288017365119 ) ) ;
#31491 = DIRECTION ( 'NONE',  ( -1.000000000000000000, -0.000000000000000000, -0.000000000000000000 ) ) ;
#31493 = CARTESIAN_POINT ( 'NONE',  ( 24.75830837035764276, 3.019210359990082804, 3.350572556515618583 ) ) ;
#31492 = CARTESIAN_POINT ( 'NONE',  ( 23.63060222782971920, 2.673617165426260822, 4.137625349533057495 ) ) ;
#31495 = ORIENTED_EDGE ( 'NONE', *, *, #7264, .F. ) ;
#31494 = EDGE_LOOP ( 'NONE', ( #25864, #12344, #6573, #20642 ) ) ;
#31496 = CARTESIAN_POINT ( 'NONE',  ( 82.00886418671275635, 63.26204695399086120, -2.636331425444868870 ) ) ;
#31497 = CARTESIAN_POINT ( 'NONE',  ( -7.890026461918812295, -6.626103207857777159E-16, -6.000000000000000000 ) ) ;
#31498 = EDGE_CURVE ( 'NONE', #1835, #33795, #28356, .T. ) ;
#31500 = CARTESIAN_POINT ( 'NONE',  ( 1.551251297819356001, -26.64985754041175525, 6.800000000000000711 ) ) ;
#31499 = DIRECTION ( 'NONE',  ( 1.000000000000000000, 0.000000000000000000, 0.000000000000000000 ) ) ;
#31501 = LINE ( 'NONE', #28816, #30363 ) ;
#31502 = CARTESIAN_POINT ( 'NONE',  ( 0.5410499997217619317, -26.28128359000521641, 7.783750581861600182 ) ) ;
#31503 = CARTESIAN_POINT ( 'NONE',  ( 73.12040677118544352, 60.72248633788713335, 3.934110468535477079 ) ) ;
#31504 = CARTESIAN_POINT ( 'NONE',  ( 22.02891390162299246, 3.924681071272548838, -4.221871318386710925 ) ) ;
#31505 = EDGE_LOOP ( 'NONE', ( #28810, #9775, #25600, #36892 ) ) ;
#31506 = DIRECTION ( 'NONE',  ( 0.000000000000000000, 0.000000000000000000, -1.000000000000000000 ) ) ;
#31507 = VECTOR ( 'NONE', #2520, 1000.000000000000000 ) ;
#31508 = CARTESIAN_POINT ( 'NONE',  ( 21.85643539959779602, 5.813509198596546135, -11.62788251339591206 ) ) ;
#31509 = CARTESIAN_POINT ( 'NONE',  ( -58.28276732369787538, 31.18492359376757150, -4.639233030986043893 ) ) ;
#31510 = CARTESIAN_POINT ( 'NONE',  ( 1.075454873741154005, -26.12617409861640638, 7.750000000000000888 ) ) ;
#31511 = CARTESIAN_POINT ( 'NONE',  ( 80.40506551886733178, 65.76252680069860901, 2.626729253126741881 ) ) ;
#31512 = CARTESIAN_POINT ( 'NONE',  ( 84.99141033049929206, 2.891338577806874088, -0.4625859348280507155 ) ) ;
#31513 = VERTEX_POINT ( 'NONE', #34968 ) ;
#31514 = DIRECTION ( 'NONE',  ( -0.000000000000000000, -0.000000000000000000, -1.000000000000000000 ) ) ;
#31515 = ADVANCED_FACE ( 'NONE', ( #28565 ), #26096, .T. ) ;
#31516 = CARTESIAN_POINT ( 'NONE',  ( 19.70069104262061543, -2.834677804756353225, 3.278428930171599198 ) ) ;
#31517 = CARTESIAN_POINT ( 'NONE',  ( 34.77301379943533988, -3.161486423658268929, -5.633567810555343058 ) ) ;
#31518 = CARTESIAN_POINT ( 'NONE',  ( -36.44874870218064444, -25.49307895267003587, 6.700000000000000178 ) ) ;
#31519 = LINE ( 'NONE', #31723, #13448 ) ;
#31520 = ORIENTED_EDGE ( 'NONE', *, *, #4070, .T. ) ;
#31521 = CYLINDRICAL_SURFACE ( 'NONE', #25690, 3.399999999999999911 ) ;
#31522 = CARTESIAN_POINT ( 'NONE',  ( -1.278692756456701662, -31.20857796775482029, 7.784476445165072533 ) ) ;
#31523 = EDGE_CURVE ( 'NONE', #32517, #13762, #22598, .T. ) ;
#31524 = CARTESIAN_POINT ( 'NONE',  ( 32.01160833602948941, -2.960095084777874863, 5.202583703147388050 ) ) ;
#31525 = ORIENTED_EDGE ( 'NONE', *, *, #25026, .F. ) ;
#31526 = ORIENTED_EDGE ( 'NONE', *, *, #31222, .T. ) ;
#31527 = CARTESIAN_POINT ( 'NONE',  ( 37.18616516907447078, -2.963186209105021618, 6.000013960849525319 ) ) ;
#31528 = CARTESIAN_POINT ( 'NONE',  ( -1.086373026989221113, -31.68746443619045650, 7.013842709614101167 ) ) ;
#31529 = CARTESIAN_POINT ( 'NONE',  ( 66.41407057682044979, 57.81332248272632057, -4.000000000000023981 ) ) ;
#31530 = CARTESIAN_POINT ( 'NONE',  ( 87.54002591101105679, -2.043453341785346655, -3.425432998280521613 ) ) ;
#31531 = EDGE_CURVE ( 'NONE', #35842, #5754, #20898, .T. ) ;
#31532 = AXIS2_PLACEMENT_3D ( 'NONE', #13470, #934, #19457 ) ;
#31533 = ORIENTED_EDGE ( 'NONE', *, *, #30544, .T. ) ;
#31534 = CARTESIAN_POINT ( 'NONE',  ( 88.13815211262131299, -0.6432311452471944913, -2.427475510744327547 ) ) ;
#31535 = DIRECTION ( 'NONE',  ( 0.000000000000000000, 0.000000000000000000, 1.000000000000000000 ) ) ;
#31536 = CARTESIAN_POINT ( 'NONE',  ( 4.959318750259752662, -28.60070809536833636, 6.920489980334478375 ) ) ;
#31537 = B_SPLINE_CURVE_WITH_KNOTS ( 'NONE', 3,
 ( #14931, #36964, #20490, #5264, #32872, #36555, #4662, #17198, #36360, #39225, #20698, #30175, #30389, #5062, #8334, #23595, #17595, #29765, #1996, #2194, #27286, #39851, #28517, #40658, #28103, #37565, #21943, #12659, #15549, #21736, #9360 ),
 .UNSPECIFIED., .F., .F.,
 ( 4, 3, 3, 3, 3, 3, 3, 3, 3, 3, 4 ),
 ( 9.697399036122160616E-19, 2.999644130997777025E-05, 6.002588995694800887E-05, 8.960886084588142201E-05, 0.0001190604700446492420, 0.0001489538463052727504, 0.0001796139255493989120, 0.0002109707048517087591, 0.0002426195318110369015, 0.0002740640997890066719, 0.0002849778069099832270 ),
 .UNSPECIFIED. ) ;
#31538 = DIRECTION ( 'NONE',  ( -0.000000000000000000, -0.000000000000000000, -1.000000000000000000 ) ) ;
#31539 = ORIENTED_EDGE ( 'NONE', *, *, #19410, .T. ) ;
#31540 = FACE_BOUND ( 'NONE', #3872, .T. ) ;
#31541 = CARTESIAN_POINT ( 'NONE',  ( -26.24874870218063450, -26.64985754041175525, 6.800000000000000711 ) ) ;
#31542 = ORIENTED_EDGE ( 'NONE', *, *, #35743, .F. ) ;
#31543 = CARTESIAN_POINT ( 'NONE',  ( 21.73868531115960678, 6.081862488199073269, 3.283576032310306481 ) ) ;
#31544 = CARTESIAN_POINT ( 'NONE',  ( 78.69027363540493525, 66.05851491966868139, -1.011532654301245060 ) ) ;
#31545 = CARTESIAN_POINT ( 'NONE',  ( 80.60461247708464327, 63.28149962716669563, 3.592474444481852824 ) ) ;
#31546 = CARTESIAN_POINT ( 'NONE',  ( -69.92844879064466568, -20.91563447912280438, 3.916091967151599462 ) ) ;
#31547 = VERTEX_POINT ( 'NONE', #9403 ) ;
#31548 = CARTESIAN_POINT ( 'NONE',  ( 77.06776432268853227, 63.96223838934590589, -3.363831406679916203 ) ) ;
#31550 = DIRECTION ( 'NONE',  ( -0.000000000000000000, -0.000000000000000000, -1.000000000000000000 ) ) ;
#31549 = CARTESIAN_POINT ( 'NONE',  ( 3.959546255067319276, -32.24317540230298107, 7.756742906098588186 ) ) ;
#31551 = CARTESIAN_POINT ( 'NONE',  ( 20.06531201372480311, 6.854292503151608429, -3.230284889801701365 ) ) ;
#31552 = CARTESIAN_POINT ( 'NONE',  ( 80.90189697519821266, 63.80306449575952144, -3.509897338575004966 ) ) ;
#31553 = CARTESIAN_POINT ( 'NONE',  ( 76.98094665547928628, 64.12925941789167439, 3.220231295875716437 ) ) ;
#31554 = ORIENTED_EDGE ( 'NONE', *, *, #32842, .F. ) ;
#31555 = ORIENTED_EDGE ( 'NONE', *, *, #30007, .T. ) ;
#31556 = CARTESIAN_POINT ( 'NONE',  ( -39.07867591359219261, -26.64985754041175525, 6.700000000000000178 ) ) ;
#31557 = CYLINDRICAL_SURFACE ( 'NONE', #16421, 3.000000000000002665 ) ;
#31558 = CARTESIAN_POINT ( 'NONE',  ( 81.88210331175126555, 61.92077230045141789, 1.461108304021874416 ) ) ;
#31560 = CARTESIAN_POINT ( 'NONE',  ( 15.21972599668117709, 10.50943688033427392, 2.499999999998679723 ) ) ;
#31559 = CARTESIAN_POINT ( 'NONE',  ( 0.000000000000000000, 0.000000000000000000, -2.500000000000000000 ) ) ;
#31561 = CARTESIAN_POINT ( 'NONE',  ( 29.58677136987063960, -0.8116067495284342570, -6.002319972564883699 ) ) ;
#31562 = CARTESIAN_POINT ( 'NONE',  ( -1.408800653676522074, -31.17709578999077280, 6.887547729233688187 ) ) ;
#31563 = CARTESIAN_POINT ( 'NONE',  ( 14.37591153880835293, -5.022958543253408514, 2.500000000000000444 ) ) ;
#31564 = CARTESIAN_POINT ( 'NONE',  ( 1.523859786807980177, -33.06548219330246496, 6.903112506833891437 ) ) ;
#31565 = CIRCLE ( 'NONE', #16412, 4.406751979251624540 ) ;
#31566 = CARTESIAN_POINT ( 'NONE',  ( 4.685027897762059190, -31.37120921750302571, 7.784725160561907664 ) ) ;
#31567 = DIRECTION ( 'NONE',  ( 0.4999999999999980016, 0.8660254037844398178, -0.000000000000000000 ) ) ;
#31568 = LINE ( 'NONE', #3391, #30188 ) ;
#31569 = CARTESIAN_POINT ( 'NONE',  ( 33.45255242130070172, -3.771379754131906736, -5.158309509446562302 ) ) ;
#31570 = CARTESIAN_POINT ( 'NONE',  ( 20.88448294811174932, 4.552397361489173733, -2.802001057294738917 ) ) ;
#31571 = CARTESIAN_POINT ( 'NONE',  ( 4.862064339916653211, -31.08699507435702358, 7.501983001166817822 ) ) ;
#31572 = CARTESIAN_POINT ( 'NONE',  ( -0.8833599345365857891, -31.77996090580433020, 7.721096864323906850 ) ) ;
#31573 = CARTESIAN_POINT ( 'NONE',  ( 19.67572283850595838, -2.760578293782835146, -3.277270426740663378 ) ) ;
#31574 = CARTESIAN_POINT ( 'NONE',  ( 3.430328219694326108, -32.49692869527085293, 7.712764235869103757 ) ) ;
#31575 = CARTESIAN_POINT ( 'NONE',  ( 2.167464131630131519, -32.93771148289538786, 6.863904403958576594 ) ) ;
#31576 = ADVANCED_FACE ( 'NONE', ( #22201 ), #18669, .F. ) ;
#31577 = DIRECTION ( 'NONE',  ( 1.000000000000000000, 0.000000000000000000, 0.000000000000000000 ) ) ;
#31578 = CARTESIAN_POINT ( 'NONE',  ( -1.462749531912453271, -28.32311515628067511, 7.778050822775632867 ) ) ;
#31579 = EDGE_CURVE ( 'NONE', #7170, #14656, #6546, .T. ) ;
#31580 = VERTEX_POINT ( 'NONE', #19502 ) ;
#31581 = VERTEX_POINT ( 'NONE', #21783 ) ;
#31582 = CARTESIAN_POINT ( 'NONE',  ( 6.107923577950775673, -31.97397320985677993, 7.754798119455333705 ) ) ;
#31583 = CARTESIAN_POINT ( 'NONE',  ( 68.58273017919226788, 58.67848115723035107, -3.992679187475148161 ) ) ;
#31584 = ADVANCED_FACE ( 'NONE', ( #2861 ), #25476, .T. ) ;
#31585 = EDGE_LOOP ( 'NONE', ( #3354, #3281, #5047, #16772, #702 ) ) ;
#31586 = CARTESIAN_POINT ( 'NONE',  ( 22.01541346579904967, 4.834729283906541220, -3.642368534677343117 ) ) ;
#31587 = EDGE_CURVE ( 'NONE', #34426, #32530, #34532, .T. ) ;
#31588 = CARTESIAN_POINT ( 'NONE',  ( 21.85643539959776760, -15.29860455024666877, -0.2154785770160333180 ) ) ;
#31589 = CARTESIAN_POINT ( 'NONE',  ( 22.38542502781336196, 4.029546766862340590, 3.839276850840922517 ) ) ;
#31590 = CARTESIAN_POINT ( 'NONE',  ( 3.490246631599678739, -26.56219109107605547, 6.880608371227948439 ) ) ;
#31591 = PLANE ( 'NONE',  #36994 ) ;
#31592 = ORIENTED_EDGE ( 'NONE', *, *, #33802, .T. ) ;
#31593 = CARTESIAN_POINT ( 'NONE',  ( 21.71224184863732631, 6.326580208086403978, 3.193838826403248454 ) ) ;
#31594 = AXIS2_PLACEMENT_3D ( 'NONE', #3692, #4278, #32480 ) ;
#31595 = CARTESIAN_POINT ( 'NONE',  ( -26.44874870218064089, -26.64985754041175525, 6.800000000000000711 ) ) ;
#31596 = ORIENTED_EDGE ( 'NONE', *, *, #12055, .F. ) ;
#31597 = DIRECTION ( 'NONE',  ( 0.000000000000000000, 0.000000000000000000, 1.000000000000000000 ) ) ;
#31598 = ORIENTED_EDGE ( 'NONE', *, *, #20853, .T. ) ;
#31599 = CARTESIAN_POINT ( 'NONE',  ( 78.31969284963511768, 65.55289002357415029, -2.305838555344981611 ) ) ;
#31601 = CARTESIAN_POINT ( 'NONE',  ( -1.676158249790094645, -29.96863586080081632, 7.006423389747792108 ) ) ;
#31600 = CARTESIAN_POINT ( 'NONE',  ( 27.16088236247300713, 1.273373388036902920, 4.440073707454521568 ) ) ;
#31602 = CARTESIAN_POINT ( 'NONE',  ( 81.16407079065466235, 61.30196360636987407, -1.071687152255755171 ) ) ;
#31603 = CARTESIAN_POINT ( 'NONE',  ( 80.61353453797053703, 61.63497835834533589, 2.716276829189518960 ) ) ;
#31604 = AXIS2_PLACEMENT_3D ( 'NONE', #33801, #5179, #17710 ) ;
#31605 = CARTESIAN_POINT ( 'NONE',  ( 82.35470118046110599, 62.54510421749742477, 1.000000000000000000 ) ) ;
#31607 = ORIENTED_EDGE ( 'NONE', *, *, #39255, .F. ) ;
#31606 = CARTESIAN_POINT ( 'NONE',  ( 2.825595610131681035, -32.77835769072562044, 7.784838882742139532 ) ) ;
#31608 = CARTESIAN_POINT ( 'NONE',  ( 21.85643539959774273, 9.212406492340052822, 1.715677401501900956 ) ) ;
#31609 = CARTESIAN_POINT ( 'NONE',  ( 21.85643539959776760, -15.22304117831051862, 1.450816989262757151 ) ) ;
#31610 = EDGE_LOOP ( 'NONE', ( #35889, #28126, #13289, #25560, #3270, #28295, #33519 ) ) ;
#31611 = CARTESIAN_POINT ( 'NONE',  ( -75.62813303713400614, 8.531731237985169969, 10.23129255942193261 ) ) ;
#31612 = DIRECTION ( 'NONE',  ( -1.000000000000000000, 0.000000000000000000, 0.000000000000000000 ) ) ;
#31613 = ORIENTED_EDGE ( 'NONE', *, *, #12414, .T. ) ;
#31614 = CARTESIAN_POINT ( 'NONE',  ( -34.34874870218063592, -25.49307895267003587, 6.700000000000000178 ) ) ;
#31615 = CARTESIAN_POINT ( 'NONE',  ( 1.640016842007158804, -32.96939412209556508, 7.785172627573962778 ) ) ;
#31616 = CARTESIAN_POINT ( 'NONE',  ( 28.20719035837850441, -3.294622348659617117, -4.608812267538287877 ) ) ;
#31617 = CARTESIAN_POINT ( 'NONE',  ( 34.63778478821021167, -0.7807839475658682193, -5.273897451186136287 ) ) ;
#31618 = DIRECTION ( 'NONE',  ( -1.000000000000000000, 0.000000000000000000, 0.000000000000000000 ) ) ;
#31619 = CARTESIAN_POINT ( 'NONE',  ( 21.58804800731853391, 5.739108358429902523, 3.444525775481035001 ) ) ;
#31620 = CARTESIAN_POINT ( 'NONE',  ( 4.327887301732942227, -31.72776669797016424, 7.692469944509193525 ) ) ;
#31621 = CARTESIAN_POINT ( 'NONE',  ( 30.67406393699503298, -3.593393542108534344, -4.777508688867102116 ) ) ;
#31622 = AXIS2_PLACEMENT_3D ( 'NONE', #35880, #39342, #20012 ) ;
#31623 = CYLINDRICAL_SURFACE ( 'NONE', #30951, 0.1000000000000028644 ) ;
#31624 = CARTESIAN_POINT ( 'NONE',  ( 26.56410588169512721, 1.659669406648513368, -4.323734781818131978 ) ) ;
#31625 = CARTESIAN_POINT ( 'NONE',  ( 37.19747295490952155, -2.841588721108153415, -5.999818660317219887 ) ) ;
#31626 = DIRECTION ( 'NONE',  ( 0.7660444431189840087, -0.6427876096865322575, 0.000000000000000000 ) ) ;
#31627 = ORIENTED_EDGE ( 'NONE', *, *, #7347, .F. ) ;
#31628 =( BOUNDED_SURFACE ( )  B_SPLINE_SURFACE ( 3, 2, ( 
 ( #16013, #18901, #16211 ),
 ( #38428, #38230, #31878 ),
 ( #3893, #37821, #22213 ),
 ( #16408, #34782, #25687 ),
 ( #21793, #6558, #28578 ),
 ( #13316, #12511, #25290 ),
 ( #3687, #19103, #385 ),
 ( #15813, #22610, #28367 ) ),
 .UNSPECIFIED., .F., .F., .F. ) 
 B_SPLINE_SURFACE_WITH_KNOTS ( ( 4, 2, 2, 4 ),
 ( 3, 3 ),
 ( 0.002497028706408050639, 0.005364503022961082321, 0.006798240181237598379, 0.008231977339514114436 ),
 ( 0.000000000000000000, 1.000000000000000000 ),
 .UNSPECIFIED. ) 
 GEOMETRIC_REPRESENTATION_ITEM ( )  RATIONAL_B_SPLINE_SURFACE ( (
 ( 1.000000000000000000, 0.8503863343361129923, 1.000000000000000000),
 ( 1.000000000000000000, 0.8564594667157611196, 1.000000000000000000),
 ( 1.000000000000000000, 0.8588771854361650915, 1.000000000000000000),
 ( 1.000000000000000000, 0.8588307351573004622, 1.000000000000000000),
 ( 1.000000000000000000, 0.8581754178396920896, 1.000000000000000000),
 ( 1.000000000000000000, 0.8554071838990657817, 1.000000000000000000),
 ( 1.000000000000000000, 0.8533070252407790601, 1.000000000000000000),
 ( 1.000000000000000000, 0.8501577991238667975, 1.000000000000000000) ) ) 
 REPRESENTATION_ITEM ( '' )  SURFACE ( )  );
#31629 = CARTESIAN_POINT ( 'NONE',  ( 67.16030903438456789, 58.03511467963866011, 3.999036733496184048 ) ) ;
#31630 = CARTESIAN_POINT ( 'NONE',  ( 35.91723242733118582, -1.971476223945344719, 5.812150800470588408 ) ) ;
#31631 = ADVANCED_FACE ( 'NONE', ( #12295 ), #18888, .T. ) ;
#31632 = CARTESIAN_POINT ( 'NONE',  ( 5.149536281657578485, -30.16439681061213918, 7.635761828346576685 ) ) ;
#31633 = CARTESIAN_POINT ( 'NONE',  ( 88.70663687723717317, -1.959581838532896025, -1.901098908833099621 ) ) ;
#31634 = AXIS2_PLACEMENT_3D ( 'NONE', #32894, #7560, #4681 ) ;
#31635 = ADVANCED_FACE ( 'NONE', ( #13915 ), #11010, .T. ) ;
#31636 = CARTESIAN_POINT ( 'NONE',  ( 37.00354821055626076, -2.736456545284593478, -5.981696651089377426 ) ) ;
#31637 = B_SPLINE_CURVE_WITH_KNOTS ( 'NONE', 3,
 ( #16689, #4374, #10522, #9925, #1289, #22901, #10324, #3577, #6843, #35469, #13218, #19401, #7241, #26395, #38519, #19804, #35071, #16497, #23296, #16896, #7039, #16105, #38925, #29276, #10717, #28870, #7437, #22507, #31761, #476, #880 ),
 .UNSPECIFIED., .F., .F.,
 ( 4, 3, 3, 3, 3, 3, 3, 3, 3, 3, 4 ),
 ( 2.032879073410320814E-19, 3.077658087706071046E-05, 6.152638666999271666E-05, 9.267501192707260018E-05, 0.0001241882240135244839, 0.0001556618703051763680, 0.0001866161554452290799, 0.0002167966385861025652, 0.0002463805737537836694, 0.0002758761370306578569, 0.0002847094172290117169 ),
 .UNSPECIFIED. ) ;
#31638 = ORIENTED_EDGE ( 'NONE', *, *, #38903, .F. ) ;
#31639 = CARTESIAN_POINT ( 'NONE',  ( 24.38334378067764163, 2.944219297565202176, 3.714561838593425147 ) ) ;
#31640 = LINE ( 'NONE', #21971, #14056 ) ;
#31641 = DIRECTION ( 'NONE',  ( 0.9848077530122080203, 0.1736481776669307198, -0.000000000000000000 ) ) ;
#31642 = ORIENTED_EDGE ( 'NONE', *, *, #24312, .T. ) ;
#31643 = LINE ( 'NONE', #3263, #32743 ) ;
#31644 = PRODUCT_DEFINITION_CONTEXT ( 'detailed design', #25032, 'design' ) ;
#31645 = ORIENTED_EDGE ( 'NONE', *, *, #27265, .T. ) ;
#31646 = CARTESIAN_POINT ( 'NONE',  ( 1.749140210850987920, -26.17027969752984973, 6.894806418505346812 ) ) ;
#31647 = EDGE_LOOP ( 'NONE', ( #32924, #19912, #860, #37863 ) ) ;
#31648 = CARTESIAN_POINT ( 'NONE',  ( 78.94919473400545940, 65.41189549592658636, -2.864416008774570699 ) ) ;
#31649 = CARTESIAN_POINT ( 'NONE',  ( 1.700390093233090871, -29.56993018339339940, 6.000000000000001776 ) ) ;
#31650 = CARTESIAN_POINT ( 'NONE',  ( 78.77165107407959965, 65.73683965358550552, 2.311104455577570604 ) ) ;
#31653 = ORIENTED_EDGE ( 'NONE', *, *, #18735, .T. ) ;
#31652 = ORIENTED_EDGE ( 'NONE', *, *, #11092, .F. ) ;
#31651 = CARTESIAN_POINT ( 'NONE',  ( -1.342127135714882957, -31.08752830403540557, 6.979335674598002193 ) ) ;
#31654 = AXIS2_PLACEMENT_3D ( 'NONE', #32345, #10686, #29832 ) ;
#31655 = CYLINDRICAL_SURFACE ( 'NONE', #29779, 0.09010775117052882699 ) ;
#31656 = CARTESIAN_POINT ( 'NONE',  ( 28.67087680535204797, -4.024283280459782119, 4.110896467804376009 ) ) ;
#31657 = CARTESIAN_POINT ( 'NONE',  ( 3.420189869592383580, -26.52160375395355629, 7.678495282201400762 ) ) ;
#31658 = DIRECTION ( 'NONE',  ( -1.000000000000000000, 0.000000000000000000, 0.000000000000000000 ) ) ;
#31659 = CARTESIAN_POINT ( 'NONE',  ( 24.37313411410375963, 3.148815130053465250, -3.340199359379649291 ) ) ;
#31660 = VERTEX_POINT ( 'NONE', #7738 ) ;
#31661 = DIRECTION ( 'NONE',  ( -1.000000000000000000, 0.000000000000000000, 0.000000000000000000 ) ) ;
#31662 = CARTESIAN_POINT ( 'NONE',  ( -1.024514293572082568, -31.60337457229856639, 6.903372536218459921 ) ) ;
#31663 = DIRECTION ( 'NONE',  ( -0.9396926207859057634, -0.3420201433256757073, -0.000000000000000000 ) ) ;
#31664 = CARTESIAN_POINT ( 'NONE',  ( -80.91031161377242142, -5.699894439238891941, -0.6008404087775605085 ) ) ;
#31665 = CARTESIAN_POINT ( 'NONE',  ( -17.69482985384421880, -29.56993018339339940, 6.000000000000000000 ) ) ;
#31666 = CYLINDRICAL_SURFACE ( 'NONE', #24771, 0.09010775117052798044 ) ;
#31667 = CARTESIAN_POINT ( 'NONE',  ( 81.34140156818916978, 61.66514490546133942, 2.058202901128784568 ) ) ;
#31668 = CARTESIAN_POINT ( 'NONE',  ( 85.71231987865445490, 0.7872592507033150389, 5.912482239253596283 ) ) ;
#31669 = CARTESIAN_POINT ( 'NONE',  ( 22.37949047700085359, 4.044367784810037669, -2.563457211823029880 ) ) ;
#31670 = VERTEX_POINT ( 'NONE', #17193 ) ;
#31671 = PLANE ( 'NONE',  #39138 ) ;
#31672 = DIRECTION ( 'NONE',  ( 0.7660444431189770143, 0.6427876096865404731, -0.000000000000000000 ) ) ;
#31673 = ORIENTED_EDGE ( 'NONE', *, *, #32503, .T. ) ;
#31674 = CARTESIAN_POINT ( 'NONE',  ( 1.817877310917768607, -26.17195987680828750, 7.759451378593095860 ) ) ;
#31675 = DIRECTION ( 'NONE',  ( 0.6502177225477844269, 0.3754033771448388457, -0.6605219282605403475 ) ) ;
#31676 = CARTESIAN_POINT ( 'NONE',  ( 4.638438299886373350, -27.85881714212312588, 7.756377446753168314 ) ) ;
#31677 = CYLINDRICAL_SURFACE ( 'NONE', #355, 2.500000000000000000 ) ;
#31678 = CARTESIAN_POINT ( 'NONE',  ( 31.71832800154010457, -0.5603227101564068890, 5.156810213938597620 ) ) ;
#31679 = CARTESIAN_POINT ( 'NONE',  ( 86.82658554816774199, 0.8299826706514633612, -5.353109082705294952 ) ) ;
#31680 = EDGE_CURVE ( 'NONE', #21394, #11548, #16588, .T. ) ;
#31681 = VERTEX_POINT ( 'NONE', #979 ) ;
#31683 = CARTESIAN_POINT ( 'NONE',  ( -63.84790524989455918, 35.84013490037983729, 7.344445564913357316 ) ) ;
#31682 = CARTESIAN_POINT ( 'NONE',  ( 79.33528816075221357, 65.72664079943768911, -2.661900242191241439 ) ) ;
#31684 = CARTESIAN_POINT ( 'NONE',  ( -69.72909178707443800, -48.03897060390835350, 9.928799107400003265 ) ) ;
#31685 = CARTESIAN_POINT ( 'NONE',  ( -69.50501670448861091, -46.63360808430513060, 9.898256799676488527 ) ) ;
#31686 = DIRECTION ( 'NONE',  ( 0.000000000000000000, -0.6662082868431817850, 0.7457657263118712132 ) ) ;
#31687 = VERTEX_POINT ( 'NONE', #28969 ) ;
#31688 = CARTESIAN_POINT ( 'NONE',  ( -6.878675913592188884, -26.64985754041175525, 6.700000000000000178 ) ) ;
#31689 = ORIENTED_EDGE ( 'NONE', *, *, #36400, .F. ) ;
#31690 = CARTESIAN_POINT ( 'NONE',  ( -80.66421687884188430, -6.623080169578322796, 2.321096592483072651 ) ) ;
#31691 = VECTOR ( 'NONE', #33993, 1000.000000000000114 ) ;
#31692 = ORIENTED_EDGE ( 'NONE', *, *, #336, .T. ) ;
#31693 = CARTESIAN_POINT ( 'NONE',  ( 78.63380675089919691, 66.01840951946610403, -1.252362053669528796 ) ) ;
#31694 = CYLINDRICAL_SURFACE ( 'NONE', #19475, 0.1000000000000028644 ) ;
#31696 = CARTESIAN_POINT ( 'NONE',  ( 33.45749450797183044, -3.829747548865578555, 5.093667367007288505 ) ) ;
#31695 = CARTESIAN_POINT ( 'NONE',  ( 23.25599683166147713, 2.300726602830819978, 4.579218281655972334 ) ) ;
#31698 = ORIENTED_EDGE ( 'NONE', *, *, #4447, .T. ) ;
#31697 = VERTEX_POINT ( 'NONE', #19893 ) ;
#31699 = CARTESIAN_POINT ( 'NONE',  ( 81.83803008603277362, 64.28563725689721764, -2.776691787112390397 ) ) ;
#31700 = CARTESIAN_POINT ( 'NONE',  ( 4.742723045254528813, -28.05196766440798939, 6.929923840112063971 ) ) ;
#31702 = CARTESIAN_POINT ( 'NONE',  ( -32.24874870218063450, -26.64985754041175525, 6.700000000000000178 ) ) ;
#31701 = CARTESIAN_POINT ( 'NONE',  ( -69.92837670882107659, -0.7829914368874778541, 5.916079783099612577 ) ) ;
#31703 = DIRECTION ( 'NONE',  ( 0.000000000000000000, 0.000000000000000000, 1.000000000000000000 ) ) ;
#31704 = CARTESIAN_POINT ( 'NONE',  ( -64.08758708074091714, 41.79021386906870816, -3.815602545441736826 ) ) ;
#31705 = CARTESIAN_POINT ( 'NONE',  ( 71.95566904218743787, 60.28642714153433957, 3.942504219403033527 ) ) ;
#31706 = EDGE_CURVE ( 'NONE', #7366, #34454, #26612, .T. ) ;
#31707 = CARTESIAN_POINT ( 'NONE',  ( 23.87821936093323316, 3.129464447930911941, -3.683058660101061754 ) ) ;
#31708 = ORIENTED_EDGE ( 'NONE', *, *, #15249, .T. ) ;
#31709 = CARTESIAN_POINT ( 'NONE',  ( 21.85643539959774273, 8.980655621775115449, -3.220279653634019468 ) ) ;
#31710 = B_SPLINE_CURVE_WITH_KNOTS ( 'NONE', 3,
 ( #9840, #37618, #6562, #6957, #3694, #19108, #22216, #31676, #6760, #13319, #3296, #38235, #10032, #38431, #3900, #25492, #19717, #19311, #32292, #16217, #183, #4090, #22614, #22006, #31473 ),
 .UNSPECIFIED., .F., .F.,
 ( 4, 3, 3, 3, 3, 3, 3, 3, 4 ),
 ( 6.468151674593523946E-05, 9.076621574722267710E-05, 0.0001210204262067974651, 0.0001512763324577462215, 0.0001815301820994238426, 0.0002117781465860725217, 0.0002420274594459753432, 0.0002722905548971158969, 0.0002816827545175557522 ),
 .UNSPECIFIED. ) ;
#31711 = LINE ( 'NONE', #18518, #38751 ) ;
#31712 = DIRECTION ( 'NONE',  ( 0.000000000000000000, 0.000000000000000000, -1.000000000000000000 ) ) ;
#31713 = CARTESIAN_POINT ( 'NONE',  ( 79.69124582246557509, 65.94093779614271966, 2.443770662203109900 ) ) ;
#31714 = CARTESIAN_POINT ( 'NONE',  ( 87.25532471891827413, 0.3484024848758522364, -5.186905954794287510 ) ) ;
#31715 = EDGE_LOOP ( 'NONE', ( #3627, #28598, #2124, #15622 ) ) ;
#31716 = B_SPLINE_CURVE_WITH_KNOTS ( 'NONE', 3,
 ( #8859, #18535, #24726, #2310, #2521, #9070, #27401, #8656, #40161, #36467 ),
 .UNSPECIFIED., .F., .F.,
 ( 4, 3, 3, 4 ),
 ( 0.0005050348086185288150, 0.0005143352185143272798, 0.0005445898203825178321, 0.0005634294782181692223 ),
 .UNSPECIFIED. ) ;
#31717 = CARTESIAN_POINT ( 'NONE',  ( -63.08758708074093136, 41.04287353446839859, -4.000000000000000000 ) ) ;
#31718 = ORIENTED_EDGE ( 'NONE', *, *, #39409, .T. ) ;
#31719 = CARTESIAN_POINT ( 'NONE',  ( 14.77519537498673685, -4.508227731834313801, 2.512005464107180952 ) ) ;
#31720 = ADVANCED_FACE ( 'NONE', ( #32670 ), #1188, .F. ) ;
#31721 = CARTESIAN_POINT ( 'NONE',  ( 36.91112720548292714, -2.639121728185907845, -5.967272118037208806 ) ) ;
#31722 = CARTESIAN_POINT ( 'NONE',  ( 5.100336825931343299, -29.54976608050401410, 7.643333865083955736 ) ) ;
#31723 = CARTESIAN_POINT ( 'NONE',  ( -60.75950795826495465, 23.17721540975219696, 12.49999999999999645 ) ) ;
#31724 = CARTESIAN_POINT ( 'NONE',  ( 4.398201893633324033, -31.79968808245589429, 7.737115613922529889 ) ) ;
#31725 = CARTESIAN_POINT ( 'NONE',  ( -28.44874870218064444, -26.64985754041175525, 6.700000000000000178 ) ) ;
#31726 = CARTESIAN_POINT ( 'NONE',  ( -23.07867591359219617, -26.64985754041175525, 6.700000000000000178 ) ) ;
#31727 = CARTESIAN_POINT ( 'NONE',  ( 30.69436886186574398, -3.339171598047946610, 4.972328070349530726 ) ) ;
#31728 = EDGE_CURVE ( 'NONE', #26477, #40182, #29565, .T. ) ;
#31729 = ORIENTED_EDGE ( 'NONE', *, *, #36326, .F. ) ;
#31730 = AXIS2_PLACEMENT_3D ( 'NONE', #12426, #24995, #34690 ) ;
#31731 = ORIENTED_EDGE ( 'NONE', *, *, #2071, .T. ) ;
#31732 = CARTESIAN_POINT ( 'NONE',  ( 36.49318449278427323, -3.558291934896485653, 5.797216874782107787 ) ) ;
#31733 = CARTESIAN_POINT ( 'NONE',  ( -42.34874870218063592, -26.64985754041175525, 6.700000000000000178 ) ) ;
#31734 = CARTESIAN_POINT ( 'NONE',  ( 66.42198539279098668, 57.79096248115614998, -4.000000000000016875 ) ) ;
#31735 = ORIENTED_EDGE ( 'NONE', *, *, #26328, .F. ) ;
#31736 = CARTESIAN_POINT ( 'NONE',  ( 88.34504873523731305, -0.8756272516756123947, 0.6794260907704854358 ) ) ;
#31737 = LINE ( 'NONE', #38098, #952 ) ;
#31738 = CARTESIAN_POINT ( 'NONE',  ( 4.961196182289759449, -28.60704703087472112, 6.949473656533217358 ) ) ;
#31739 = EDGE_LOOP ( 'NONE', ( #814, #35789, #19530, #25546 ) ) ;
#31740 = FACE_BOUND ( 'NONE', #14863, .T. ) ;
#31741 = SURFACE_STYLE_USAGE ( .BOTH. , #10502 ) ;
#31742 = ORIENTED_EDGE ( 'NONE', *, *, #23966, .T. ) ;
#31743 = CARTESIAN_POINT ( 'NONE',  ( 23.98072841137014777, 3.290854757922614393, 3.413282162417366816 ) ) ;
#31744 = CARTESIAN_POINT ( 'NONE',  ( 79.33847868486726895, 66.30689617902910982, -1.090531591958677327 ) ) ;
#31745 = EDGE_CURVE ( 'NONE', #36954, #5967, #5978, .T. ) ;
#31746 = CARTESIAN_POINT ( 'NONE',  ( 80.83002518733269426, 62.39751428130118427, 3.213872034465152350 ) ) ;
#31747 = DIRECTION ( 'NONE',  ( 0.000000000000000000, 0.000000000000000000, 1.000000000000000000 ) ) ;
#31748 = VERTEX_POINT ( 'NONE', #7140 ) ;
#31749 = ORIENTED_EDGE ( 'NONE', *, *, #40163, .F. ) ;
#31750 = CARTESIAN_POINT ( 'NONE',  ( 76.28050337382489943, 62.76811984040514858, -3.753756190325745035 ) ) ;
#31752 = DIRECTION ( 'NONE',  ( 1.000000000000000000, 0.000000000000000000, 0.000000000000000000 ) ) ;
#31751 = CARTESIAN_POINT ( 'NONE',  ( -71.84378200722045449, -45.92474028164770772, 5.930323375109142425 ) ) ;
#31753 = CARTESIAN_POINT ( 'NONE',  ( 15.99242138985683681, 10.20549556836962779, -2.702402154696804004 ) ) ;
#31754 = CARTESIAN_POINT ( 'NONE',  ( 81.14353007428546505, 63.18723978346947945, -3.330128783915603297 ) ) ;
#31755 = CARTESIAN_POINT ( 'NONE',  ( 77.97077402951191516, 60.66921691151922857, 3.160174624583325986 ) ) ;
#31756 = AXIS2_PLACEMENT_3D ( 'NONE', #36944, #33049, #27071 ) ;
#31757 = EDGE_LOOP ( 'NONE', ( #19922, #29674, #26856, #287 ) ) ;
#31758 = CARTESIAN_POINT ( 'NONE',  ( -12.24874870218063627, -26.64985754041175525, 6.700000000000000178 ) ) ;
#31759 = CARTESIAN_POINT ( 'NONE',  ( -64.08758708074093136, 24.84364830758653397, -3.800414904976364028 ) ) ;
#31760 = CARTESIAN_POINT ( 'NONE',  ( 82.20862031248780966, 64.47799227860164706, 2.164558651853291771 ) ) ;
#31762 = CARTESIAN_POINT ( 'NONE',  ( 2.737092283054774811, -32.91287029198328185, 7.013842709614101167 ) ) ;
#31761 = CARTESIAN_POINT ( 'NONE',  ( -0.1973417567568397646, -32.51078328414810414, 7.009310105710488514 ) ) ;
#31763 = CARTESIAN_POINT ( 'NONE',  ( 28.08579234408868786, -0.7886013899455160958, -6.074239229908586779 ) ) ;
#31764 = EDGE_CURVE ( 'NONE', #14437, #4780, #19700, .T. ) ;
#31765 = ADVANCED_FACE ( 'NONE', ( #14708 ), #14510, .T. ) ;
#31766 = CARTESIAN_POINT ( 'NONE',  ( -1.413520448806379726, -31.16791775245024354, 7.009310105710485850 ) ) ;
#31767 = CARTESIAN_POINT ( 'NONE',  ( -64.42495406928411228, 36.58927325464082259, 5.700117363500042167 ) ) ;
#31768 = EDGE_CURVE ( 'NONE', #35369, #14571, #28792, .T. ) ;
#31769 = CARTESIAN_POINT ( 'NONE',  ( 4.740160921379847458, -31.30480577326951064, 7.750000000000000000 ) ) ;
#31770 = DIRECTION ( 'NONE',  ( 0.000000000000000000, 1.000000000000000000, 0.000000000000000000 ) ) ;
#31771 = CARTESIAN_POINT ( 'NONE',  ( 69.57070405849451333, 58.21122316646445682, 3.900048895444411023 ) ) ;
#31772 = CARTESIAN_POINT ( 'NONE',  ( -70.92837670882107659, -45.61702805680359063, 6.000000000000002665 ) ) ;
#31773 = CARTESIAN_POINT ( 'NONE',  ( 35.61928182240458796, -1.517342461334751036, -5.701831105538472499 ) ) ;
#31774 = CARTESIAN_POINT ( 'NONE',  ( -42.24874870218063450, -26.64985754041175525, 6.700000000000000178 ) ) ;
#31775 = CARTESIAN_POINT ( 'NONE',  ( 4.358324848093442228, -27.29278661098419079, 7.698786668945015066 ) ) ;
#31776 = B_SPLINE_CURVE_WITH_KNOTS ( 'NONE', 3,
 ( #15021, #37856, #15637, #37047 ),
 .UNSPECIFIED., .F., .F.,
 ( 4, 4 ),
 ( 4.336808689942017736E-19, 6.391136169992664923E-06 ),
 .UNSPECIFIED. ) ;
#31777 = CARTESIAN_POINT ( 'NONE',  ( 1.700390093233090871, -29.56993018339339940, 7.750000000000000888 ) ) ;
#31778 = CARTESIAN_POINT ( 'NONE',  ( -81.79890681550139675, 10.46299657128043314, 0.6911394749367771873 ) ) ;
#31779 = AXIS2_PLACEMENT_3D ( 'NONE', #21773, #18881, #34152 ) ;
#31780 = CARTESIAN_POINT ( 'NONE',  ( 21.99697979076537990, -11.79337463441197720, -2.500000000000000000 ) ) ;
#31781 = CARTESIAN_POINT ( 'NONE',  ( 22.01888982478448042, -11.64019164401367945, 2.500000000000000000 ) ) ;
#31782 = ORIENTED_EDGE ( 'NONE', *, *, #40621, .T. ) ;
#31783 = ORIENTED_EDGE ( 'NONE', *, *, #37990, .T. ) ;
#31784 = CARTESIAN_POINT ( 'NONE',  ( -2.772340841568255776, -28.07161080258395103, 7.754798119455333705 ) ) ;
#31785 = CARTESIAN_POINT ( 'NONE',  ( 68.69556364554829031, 58.38064408996493171, -3.985059344218202515 ) ) ;
#31786 = VECTOR ( 'NONE', #22142, 1000.000000000000000 ) ;
#31787 = ORIENTED_EDGE ( 'NONE', *, *, #8590, .T. ) ;
#31788 = CARTESIAN_POINT ( 'NONE',  ( -26.87867591359219333, -26.64985754041175525, 6.800000000000000711 ) ) ;
#31789 = CARTESIAN_POINT ( 'NONE',  ( -1.597345864091041623, -28.39734911814382201, 7.737115613922534330 ) ) ;
#31790 = CARTESIAN_POINT ( 'NONE',  ( 23.96637146509650407, 2.887031144839279584, 3.870854377651337330 ) ) ;
#31791 = B_SPLINE_CURVE_WITH_KNOTS ( 'NONE', 3,
 ( #7565, #32699, #4499, #19529 ),
 .UNSPECIFIED., .F., .F.,
 ( 4, 4 ),
 ( 0.05274299500989229617, 0.1795419177415450984 ),
 .UNSPECIFIED. ) ;
#31792 = CARTESIAN_POINT ( 'NONE',  ( 3.605735085879740343, -26.63400187606387703, 6.912143950357348743 ) ) ;
#31793 = CARTESIAN_POINT ( 'NONE',  ( 5.051944483554787091, -30.14184203736685674, 7.748216051605119503 ) ) ;
#31794 = ORIENTED_EDGE ( 'NONE', *, *, #5627, .F. ) ;
#31795 = PLANE ( 'NONE',  #29381 ) ;
#31796 = CARTESIAN_POINT ( 'NONE',  ( 19.46067669853512783, -3.065043108541300132, 3.182343406304090294 ) ) ;
#31798 = AXIS2_PLACEMENT_3D ( 'NONE', #40303, #24883, #18686 ) ;
#31797 = CARTESIAN_POINT ( 'NONE',  ( 78.84693035237091863, 66.01116107573028557, 1.842213953838237384 ) ) ;
#31799 = ORIENTED_EDGE ( 'NONE', *, *, #16501, .F. ) ;
#31800 = DIRECTION ( 'NONE',  ( -0.000000000000000000, -1.000000000000000000, -0.000000000000000000 ) ) ;
#31801 = ORIENTED_EDGE ( 'NONE', *, *, #28450, .T. ) ;
#31802 = CARTESIAN_POINT ( 'NONE',  ( 79.36252896413687097, 63.71833510339342155, -3.756013696796374202 ) ) ;
#31804 = CARTESIAN_POINT ( 'NONE',  ( -1.661437721498786990, -30.07797914175773002, 6.870716933885664623 ) ) ;
#31803 = CARTESIAN_POINT ( 'NONE',  ( 26.60903577415927757, 1.048885659047656960, 4.376956920250358429 ) ) ;
#31805 = CARTESIAN_POINT ( 'NONE',  ( 81.68688842593499544, 61.98347795596144749, -2.134710458528695121 ) ) ;
#31806 = CARTESIAN_POINT ( 'NONE',  ( 79.98243830041433000, 63.02105934045280833, 3.686141857899485341 ) ) ;
#31807 = EDGE_LOOP ( 'NONE', ( #37357, #9846, #6067, #39793 ) ) ;
#31808 = ADVANCED_FACE ( 'NONE', ( #18213 ), #39970, .T. ) ;
#31809 = ADVANCED_FACE ( 'NONE', ( #23777 ), #38451, .F. ) ;
#31810 = CARTESIAN_POINT ( 'NONE',  ( -1.589597924990603817, -30.72125543040018769, 7.785096263473211486 ) ) ;
#31811 = CARTESIAN_POINT ( 'NONE',  ( -63.16167114476460398, 41.43486696125795277, 4.000000000000000000 ) ) ;
#31812 = CARTESIAN_POINT ( 'NONE',  ( 22.81652408475101979, -6.765098194116612618, -2.522738730058198264 ) ) ;
#31813 = CARTESIAN_POINT ( 'NONE',  ( -30.34874870218063947, -25.49307895267003587, 6.700000000000000178 ) ) ;
#31814 = ORIENTED_EDGE ( 'NONE', *, *, #2356, .T. ) ;
#31815 = CARTESIAN_POINT ( 'NONE',  ( -76.06923559113667466, 8.888346553459479438, 10.02136333681344027 ) ) ;
#31816 = CARTESIAN_POINT ( 'NONE',  ( 24.11609145789137543, 0.4541001735588878763, -5.103011939257064533 ) ) ;
#31817 = ORIENTED_EDGE ( 'NONE', *, *, #19712, .T. ) ;
#31818 = EDGE_CURVE ( 'NONE', #33155, #33614, #3837, .T. ) ;
#31819 = CARTESIAN_POINT ( 'NONE',  ( -30.24874870218063450, -26.64985754041175525, 6.700000000000000178 ) ) ;
#31820 = VERTEX_POINT ( 'NONE', #7893 ) ;
#31821 = CARTESIAN_POINT ( 'NONE',  ( 1.735061201785046414, -32.96975431474913876, 7.712764235869103757 ) ) ;
#31822 = CARTESIAN_POINT ( 'NONE',  ( 30.75021987934201206, -3.703070994598137045, -4.640474062878059414 ) ) ;
#31823 = CARTESIAN_POINT ( 'NONE',  ( 29.48879446675499949, 1.220267147247336981, -4.220664948178088238 ) ) ;
#31824 = CARTESIAN_POINT ( 'NONE',  ( -79.95330471031414277, 33.71485196875532608, -8.800414904976364028 ) ) ;
#31825 = CARTESIAN_POINT ( 'NONE',  ( 16.14458128353912869, 10.33471859280096083, 2.711087558826402510 ) ) ;
#31826 = DIRECTION ( 'NONE',  ( 1.000000000000000000, -0.000000000000000000, -0.000000000000000000 ) ) ;
#31827 = DIRECTION ( 'NONE',  ( 0.000000000000000000, 0.000000000000000000, 1.000000000000000000 ) ) ;
#31828 = DIRECTION ( 'NONE',  ( 0.000000000000000000, 0.000000000000000000, -1.000000000000000000 ) ) ;
#31829 = VECTOR ( 'NONE', #15726, 1000.000000000000114 ) ;
#31830 = DIRECTION ( 'NONE',  ( 1.000000000000000000, 0.000000000000000000, 0.000000000000000000 ) ) ;
#31831 = CARTESIAN_POINT ( 'NONE',  ( 30.82885584354832886, 0.7157400049436221101, -4.487457763936902211 ) ) ;
#31832 = CYLINDRICAL_SURFACE ( 'NONE', #23586, 0.09010775117053029803 ) ;
#31833 = ORIENTED_EDGE ( 'NONE', *, *, #6530, .T. ) ;
#31834 = ORIENTED_EDGE ( 'NONE', *, *, #31085, .F. ) ;
#31835 = CARTESIAN_POINT ( 'NONE',  ( 66.86527468745164526, 57.93417386730686758, 3.999594749379963066 ) ) ;
#31836 = VECTOR ( 'NONE', #37081, 1000.000000000000000 ) ;
#31837 = CARTESIAN_POINT ( 'NONE',  ( -0.2487487021806331078, -25.49307895267003587, 6.700000000000000178 ) ) ;
#31838 = CARTESIAN_POINT ( 'NONE',  ( 87.06807637922989329, 0.009568187950425697044, -5.830412620327568796 ) ) ;
#31839 = VECTOR ( 'NONE', #22496, 1000.000000000000000 ) ;
#31840 = EDGE_LOOP ( 'NONE', ( #12907, #32324, #8895, #39913, #6171, #15473 ) ) ;
#31841 = CARTESIAN_POINT ( 'NONE',  ( 24.58836688147599503, 2.713802262352938310, 3.887621106702806362 ) ) ;
#31842 = CARTESIAN_POINT ( 'NONE',  ( 1.123288416806107026, -32.92059484209399045, 7.635761828346577573 ) ) ;
#31843 = CARTESIAN_POINT ( 'NONE',  ( -1.766085975226569404, -30.05319374170961666, 7.750000000000000888 ) ) ;
#31844 = ORIENTED_EDGE ( 'NONE', *, *, #12933, .F. ) ;
#31845 = CARTESIAN_POINT ( 'NONE',  ( 3.944592287501505368, -26.88591301102037434, 7.762796336881261361 ) ) ;
#31846 = ORIENTED_EDGE ( 'NONE', *, *, #10083, .T. ) ;
#31847 = VERTEX_POINT ( 'NONE', #2146 ) ;
#31848 = CARTESIAN_POINT ( 'NONE',  ( 78.87073352949229843, 65.61655597148102004, -2.590854534519451580 ) ) ;
#31849 = CARTESIAN_POINT ( 'NONE',  ( -1.734658545019058140, -28.94585822693442978, 7.778495531946296282 ) ) ;
#31850 = CARTESIAN_POINT ( 'NONE',  ( 80.86726794284579967, 61.90233618827342355, 2.830664096605171931 ) ) ;
#31852 = ORIENTED_EDGE ( 'NONE', *, *, #22474, .F. ) ;
#31851 = CARTESIAN_POINT ( 'NONE',  ( 3.300000000000000711, 0.000000000000000000, 0.000000000000000000 ) ) ;
#31853 = AXIS2_PLACEMENT_3D ( 'NONE', #17422, #27729, #14971 ) ;
#31854 = CARTESIAN_POINT ( 'NONE',  ( -0.05419868157304204986, -26.54308200390424588, 7.762796336881261361 ) ) ;
#31855 = CARTESIAN_POINT ( 'NONE',  ( -14.34874870218063769, -26.64985754041175525, 6.700000000000000178 ) ) ;
#31856 = DIRECTION ( 'NONE',  ( 0.1736481776669361321, -0.9848077530122070211, 0.000000000000000000 ) ) ;
#31857 = CARTESIAN_POINT ( 'NONE',  ( 33.85503891423564227, -5.198044821503557067, -2.407580783687792714 ) ) ;
#31858 = CARTESIAN_POINT ( 'NONE',  ( 22.00038671397952328, 5.557044130675768301, -3.122614658259094345 ) ) ;
#31859 = EDGE_LOOP ( 'NONE', ( #21416, #13646, #4248, #221 ) ) ;
#31860 = CARTESIAN_POINT ( 'NONE',  ( -64.94969296618683074, 34.86786693855481900, -6.612442482648054565 ) ) ;
#31861 = EDGE_CURVE ( 'NONE', #11926, #29061, #5625, .T. ) ;
#31862 = ORIENTED_EDGE ( 'NONE', *, *, #8343, .F. ) ;
#31863 = EDGE_CURVE ( 'NONE', #12351, #39112, #13681, .T. ) ;
#31864 = AXIS2_PLACEMENT_3D ( 'NONE', #22157, #37568, #3443 ) ;
#31865 = CARTESIAN_POINT ( 'NONE',  ( -1.755591130170437664, -30.12327797952368513, 6.875671892026062437 ) ) ;
#31866 = CARTESIAN_POINT ( 'NONE',  ( -0.5477105494940386343, -32.24823869409008381, 7.767720160662275219 ) ) ;
#31867 = ADVANCED_BREP_SHAPE_REPRESENTATION ( '', ( #39399, #30744 ), #27429 ) ;
#31868 = ADVANCED_FACE ( 'NONE', ( #23739 ), #36709, .F. ) ;
#31869 = CARTESIAN_POINT ( 'NONE',  ( -78.21354329911019931, -5.182362620687199772, -8.529621072396848191 ) ) ;
#31870 = CARTESIAN_POINT ( 'NONE',  ( 3.691161820386744008, -26.80493765813324103, 7.505001789837627335 ) ) ;
#31871 = CARTESIAN_POINT ( 'NONE',  ( 5.133587308272485217, -30.25056153508439394, 6.867280401193709416 ) ) ;
#31872 = CARTESIAN_POINT ( 'NONE',  ( 79.22467975445889010, 65.90355157830849464, 2.361823859647586232 ) ) ;
#31873 = CARTESIAN_POINT ( 'NONE',  ( -94.24726447194083789, -65.19654454972992141, 8.800414904976364028 ) ) ;
#31874 =( BOUNDED_CURVE ( )  B_SPLINE_CURVE ( 3, ( #28583, #28988, #38640, #1206 ),
 .UNSPECIFIED., .F., .T. ) 
 B_SPLINE_CURVE_WITH_KNOTS ( ( 4, 4 ),
 ( 4.708531083176467291, 4.895802057644188743 ),
 .UNSPECIFIED. ) 
 CURVE ( )  GEOMETRIC_REPRESENTATION_ITEM ( )  RATIONAL_B_SPLINE_CURVE ( ( 1.000000000000000000, 0.9970795998553221295, 0.9970795998553221295, 1.000000000000000000 ) ) 
 REPRESENTATION_ITEM ( '' )  );
#31875 = FACE_OUTER_BOUND ( 'NONE', #13599, .T. ) ;
#31876 = ORIENTED_EDGE ( 'NONE', *, *, #27265, .F. ) ;
#31877 = CARTESIAN_POINT ( 'NONE',  ( -70.92837670882107659, 13.37661300689599742, 0.000000000000000000 ) ) ;
#31878 = CARTESIAN_POINT ( 'NONE',  ( 24.93859128955816118, 3.471607954000472507, 1.313953044955986638 ) ) ;
#31879 = B_SPLINE_CURVE_WITH_KNOTS ( 'NONE', 3,
 ( #7832, #24078, #4951, #17478, #30070, #1882, #33582, #5359, #17897, #8633 ),
 .UNSPECIFIED., .F., .F.,
 ( 4, 3, 3, 4 ),
 ( 9.697399036122160616E-19, 3.025570593003099799E-05, 6.051145698343934779E-05, 6.468151674593381644E-05 ),
 .UNSPECIFIED. ) ;
#31880 = CARTESIAN_POINT ( 'NONE',  ( 1.820100332811088739, -26.17203762333147310, 7.757178535559534183 ) ) ;
#31881 = CARTESIAN_POINT ( 'NONE',  ( 14.61802081865033642, -65.19654454972992141, -3.500000000000000000 ) ) ;
#31882 = LINE ( 'NONE', #6357, #19541 ) ;
#31883 = CARTESIAN_POINT ( 'NONE',  ( -26.97867591359219475, -26.64985754041175525, 6.700000000000000178 ) ) ;
#31884 = EDGE_LOOP ( 'NONE', ( #7321, #17476, #31846, #38912 ) ) ;
#31885 = CARTESIAN_POINT ( 'NONE',  ( 68.64726599134355922, 58.50818873767699557, 3.992679187475169922 ) ) ;
#31886 = CARTESIAN_POINT ( 'NONE',  ( 36.63360656337776788, -3.080934146991386235, 5.923958309974630687 ) ) ;
#31887 = AXIS2_PLACEMENT_3D ( 'NONE', #10932, #16909, #23511 ) ;
#31888 = VECTOR ( 'NONE', #27744, 1000.000000000000000 ) ;
#31889 = CARTESIAN_POINT ( 'NONE',  ( 86.52980085923458375, 1.163345319512251841, 5.105528906334227734 ) ) ;
#31890 = ORIENTED_EDGE ( 'NONE', *, *, #2688, .F. ) ;
#31892 = CARTESIAN_POINT ( 'NONE',  ( 14.77114201464572751, -5.163092950663593861, 2.500000000000000000 ) ) ;
#31891 = CARTESIAN_POINT ( 'NONE',  ( 81.20826633916702519, 61.35171532218112844, -1.496866203714589449 ) ) ;
#31893 = CARTESIAN_POINT ( 'NONE',  ( 2.931185808669444448, -32.84638282411071941, 7.695279973900954751 ) ) ;
#31894 = FACE_OUTER_BOUND ( 'NONE', #38091, .T. ) ;
#31895 = ORIENTED_EDGE ( 'NONE', *, *, #32245, .F. ) ;
#31896 = CARTESIAN_POINT ( 'NONE',  ( -1.652919361092105577, -29.00839296038465065, 7.730758795053803034 ) ) ;
#31897 = AXIS2_PLACEMENT_3D ( 'NONE', #16771, #19277, #10406 ) ;
#31898 = VERTEX_POINT ( 'NONE', #17341 ) ;
#31899 = DIRECTION ( 'NONE',  ( 1.000000000000000000, -0.000000000000000000, -0.000000000000000000 ) ) ;
#31900 = ORIENTED_EDGE ( 'NONE', *, *, #22261, .F. ) ;
#31901 = CARTESIAN_POINT ( 'NONE',  ( 78.62614802285547455, 66.01297166972811681, -1.268354304253246800 ) ) ;
#31902 = CARTESIAN_POINT ( 'NONE',  ( 24.05450016081345055, 3.308680331767146043, 3.188065492737387707 ) ) ;
#31903 = CARTESIAN_POINT ( 'NONE',  ( 25.20701090240159559, 1.570586567452724180, 4.374205870625836212 ) ) ;
#31905 = EDGE_LOOP ( 'NONE', ( #38650, #31495, #9875, #806 ) ) ;
#31904 = ORIENTED_EDGE ( 'NONE', *, *, #7349, .T. ) ;
#31906 = CARTESIAN_POINT ( 'NONE',  ( 79.43434746088962584, 66.19712225821032803, -1.744953761006743598 ) ) ;
#31907 = CARTESIAN_POINT ( 'NONE',  ( 4.737000972096239160, -28.04055306496577771, 6.903372536218456368 ) ) ;
#31909 = CARTESIAN_POINT ( 'NONE',  ( 85.73540692764241555, 2.055646287687114881, 3.760641883467473967 ) ) ;
#31908 = CARTESIAN_POINT ( 'NONE',  ( -57.37156913083832421, 30.38049303703153470, -3.770258250959034996 ) ) ;
#31910 = CARTESIAN_POINT ( 'NONE',  ( 81.16957891225059996, 61.30398062001309256, 4.000000000000000000 ) ) ;
#31911 = CARTESIAN_POINT ( 'NONE',  ( -64.08758708074093136, 42.61892514857068193, -2.587732768873741929 ) ) ;
#31912 = CARTESIAN_POINT ( 'NONE',  ( 69.57837460818548436, 59.54477471642375974, 3.931953536312648989 ) ) ;
#31913 = CARTESIAN_POINT ( 'NONE',  ( 22.40668529979953405, 3.759187042868666673, -4.020463199049926217 ) ) ;
#31914 = ORIENTED_EDGE ( 'NONE', *, *, #29741, .T. ) ;
#31915 = VERTEX_POINT ( 'NONE', #8490 ) ;
#31916 = AXIS2_PLACEMENT_3D ( 'NONE', #21029, #11940, #33185 ) ;
#31917 = CARTESIAN_POINT ( 'NONE',  ( 21.85643539959776760, -10.46150609831112455, 5.349806725441734301 ) ) ;
#31918 = AXIS2_PLACEMENT_3D ( 'NONE', #21452, #5800, #27008 ) ;
#31920 = EDGE_CURVE ( 'NONE', #31037, #35202, #20445, .T. ) ;
#31919 = CARTESIAN_POINT ( 'NONE',  ( 17.09067283330163178, 14.51200607630100947, 6.135166493427014844E-13 ) ) ;
#31921 = CARTESIAN_POINT ( 'NONE',  ( 1.905688531271448882, -26.06911211313256160, 7.387053503561885393 ) ) ;
#31922 = CARTESIAN_POINT ( 'NONE',  ( 79.46506916754634631, 66.04886526173142158, 2.198649373794023809 ) ) ;
#31923 = AXIS2_PLACEMENT_3D ( 'NONE', #7705, #8502, #10981 ) ;
#31924 = CARTESIAN_POINT ( 'NONE',  ( 88.76896161869186130, -1.545781173472005943, 2.128395682968124092 ) ) ;
#31925 = ORIENTED_EDGE ( 'NONE', *, *, #13852, .F. ) ;
#31926 = CARTESIAN_POINT ( 'NONE',  ( 2.737092283054774811, -32.91287029198328185, 7.013842709614101167 ) ) ;
#31927 = ORIENTED_EDGE ( 'NONE', *, *, #26203, .F. ) ;
#31928 = CARTESIAN_POINT ( 'NONE',  ( 15.54228167590041387, -3.627593571885062929, 2.632146965663780591 ) ) ;
#31929 = CARTESIAN_POINT ( 'NONE',  ( 37.05019957443847289, -2.827376547557467923, 5.988977724690694338 ) ) ;
#31930 = CARTESIAN_POINT ( 'NONE',  ( 31.09877180861311174, -3.763035568191606561, 4.622249389808555264 ) ) ;
#31931 = CARTESIAN_POINT ( 'NONE',  ( 35.45376175006065722, -1.914248393079300614, -5.739814992201846877 ) ) ;
#31932 = CARTESIAN_POINT ( 'NONE',  ( 5.164678889462458677, -29.07712452480497589, 7.761113333117546809 ) ) ;
#31933 = CARTESIAN_POINT ( 'NONE',  ( -4.878675913592187108, -24.55319635012989110, 6.800000000000000711 ) ) ;
#31934 = CARTESIAN_POINT ( 'NONE',  ( -2.448748702180640446, -26.64985754041175525, 6.700000000000000178 ) ) ;
#31935 = EDGE_LOOP ( 'NONE', ( #17081, #23591, #20249, #17101 ) ) ;
#31936 = CARTESIAN_POINT ( 'NONE',  ( -1.237658113420181394, -31.28104322466368359, 7.756377446753165650 ) ) ;
#31937 = DIRECTION ( 'NONE',  ( 1.000000000000000000, 0.000000000000000000, 0.000000000000000000 ) ) ;
#31938 = ORIENTED_EDGE ( 'NONE', *, *, #21970, .T. ) ;
#31939 = ORIENTED_EDGE ( 'NONE', *, *, #8866, .T. ) ;
#31940 = CARTESIAN_POINT ( 'NONE',  ( 36.88774144847645431, -3.350387819064732042, 5.910883484843293623 ) ) ;
#31941 = CARTESIAN_POINT ( 'NONE',  ( 1.590611208492059170, -33.06561673995959438, 7.766640943994648438 ) ) ;
#31942 = ADVANCED_FACE ( 'NONE', ( #27445 ), #11370, .F. ) ;
#31943 = CARTESIAN_POINT ( 'NONE',  ( 66.70577848186255210, 57.91700714588437648, -3.999628797553631543 ) ) ;
#31944 = AXIS2_PLACEMENT_3D ( 'NONE', #21176, #23832, #40100 ) ;
#31945 = VERTEX_POINT ( 'NONE', #36509 ) ;
#31946 = B_SPLINE_CURVE_WITH_KNOTS ( 'NONE', 3,
 ( #23587, #39214, #11001, #30380 ),
 .UNSPECIFIED., .F., .F.,
 ( 4, 4 ),
 ( 0.000000000000000000, 6.391136169992754709E-06 ),
 .UNSPECIFIED. ) ;
#31947 = CARTESIAN_POINT ( 'NONE',  ( -80.93488670107193172, 11.45404655845930897, -0.2160027379189757291 ) ) ;
#31948 = DIRECTION ( 'NONE',  ( -0.000000000000000000, -1.000000000000000000, -0.000000000000000000 ) ) ;
#31949 = CARTESIAN_POINT ( 'NONE',  ( -0.8675331577758178536, -27.19174302261571086, 7.011627023500183853 ) ) ;
#31950 = ORIENTED_EDGE ( 'NONE', *, *, #30683, .T. ) ;
#31951 = FACE_BOUND ( 'NONE', #24534, .T. ) ;
#31952 = LINE ( 'NONE', #7224, #36378 ) ;
#31953 = ORIENTED_EDGE ( 'NONE', *, *, #20915, .F. ) ;
#31954 = CARTESIAN_POINT ( 'NONE',  ( 22.45301647707092130, 4.683739370715508166, 3.229772300555033393 ) ) ;
#31955 = VECTOR ( 'NONE', #12048, 1000.000000000000000 ) ;
#31956 = CARTESIAN_POINT ( 'NONE',  ( 82.49284700683510607, 64.23424719397910110, -1.468380750528963663 ) ) ;
#31957 = CARTESIAN_POINT ( 'NONE',  ( -0.7996099067669091287, -29.56993018339339940, 6.800000000000000711 ) ) ;
#31958 = EDGE_CURVE ( 'NONE', #10407, #33823, #11808, .T. ) ;
#31959 = CARTESIAN_POINT ( 'NONE',  ( -28.24874870218063805, -26.64985754041175525, 6.700000000000000178 ) ) ;
#31960 = ORIENTED_EDGE ( 'NONE', *, *, #26217, .T. ) ;
#31961 = ORIENTED_EDGE ( 'NONE', *, *, #36491, .F. ) ;
#31962 = CARTESIAN_POINT ( 'NONE',  ( 75.90485726080815709, 62.11260916716577185, -3.867068906737686440 ) ) ;
#31964 = CARTESIAN_POINT ( 'NONE',  ( 4.370302737341240196, -27.30684236520528785, 7.750000000000000000 ) ) ;
#31963 = CARTESIAN_POINT ( 'NONE',  ( 2.492297145206303632, -26.16069239315658379, 6.925313231306332362 ) ) ;
#31965 = CARTESIAN_POINT ( 'NONE',  ( 14.82829946762850604, 12.56923040459623131, -2.515064524949301550 ) ) ;
#31966 = CARTESIAN_POINT ( 'NONE',  ( 79.64653587341230434, 65.62447382577089172, -2.816708194897767026 ) ) ;
#31967 = CARTESIAN_POINT ( 'NONE',  ( 75.98741087703858454, 61.93803417815122003, 3.887901781367217424 ) ) ;
#31968 = ORIENTED_EDGE ( 'NONE', *, *, #17621, .F. ) ;
#31969 = CARTESIAN_POINT ( 'NONE',  ( -4.348748702180639469, -26.64985754041175525, 6.700000000000000178 ) ) ;
#31971 = ADVANCED_FACE ( 'NONE', ( #6651 ), #2174, .T. ) ;
#31970 = DIRECTION ( 'NONE',  ( 0.000000000000000000, -1.000000000000000000, 0.000000000000000000 ) ) ;
#31972 = CARTESIAN_POINT ( 'NONE',  ( 81.48599817137706225, 65.27445208842065938, 2.474249079298665777 ) ) ;
#31974 = LINE ( 'NONE', #477, #18962 ) ;
#31973 = FACE_OUTER_BOUND ( 'NONE', #4206, .T. ) ;
#31975 = CARTESIAN_POINT ( 'NONE',  ( 26.56634348862415251, 2.991955253353971500, -0.5426703667890996341 ) ) ;
#31976 = CARTESIAN_POINT ( 'NONE',  ( -1.699525402281838682, -29.59462277852799161, 7.740055089680398126 ) ) ;
#31977 = CARTESIAN_POINT ( 'NONE',  ( 3.578431782309205111, -26.73568126667343847, 6.939395833800440450 ) ) ;
#31978 = ORIENTED_EDGE ( 'NONE', *, *, #11125, .T. ) ;
#31979 = AXIS2_PLACEMENT_3D ( 'NONE', #27092, #33077, #39638 ) ;
#31980 = CARTESIAN_POINT ( 'NONE',  ( -1.432293644835494373, -27.47664038617742577, -1.000000000000000000 ) ) ;
#31981 = TOROIDAL_SURFACE ( 'NONE', #40485, 31.02204673211315011, 3.000000000000000000 ) ;
#31982 = DIRECTION ( 'NONE',  ( -0.3420201433256601087, -0.9396926207859114255, -0.000000000000000000 ) ) ;
#31983 = DIRECTION ( 'NONE',  ( 0.4690749385695657803, 0.8831583674551003460, 0.000000000000000000 ) ) ;
#31984 = CARTESIAN_POINT ( 'NONE',  ( 36.94055750684482575, -3.101496826522602834, -5.970271882717379519 ) ) ;
#31985 = CARTESIAN_POINT ( 'NONE',  ( -61.24591834330252027, -23.80776546975053520, -2.500000000000000000 ) ) ;
#31986 = CARTESIAN_POINT ( 'NONE',  ( 4.358291535071521672, -27.29274773012506827, 7.695279973900954751 ) ) ;
#31987 = FACE_OUTER_BOUND ( 'NONE', #8683, .T. ) ;
#31988 = CARTESIAN_POINT ( 'NONE',  ( -78.24496198277260817, 10.07981855400444893, 8.538017541507711528 ) ) ;
#31989 = AXIS2_PLACEMENT_3D ( 'NONE', #28673, #9515, #18570 ) ;
#31990 = CARTESIAN_POINT ( 'NONE',  ( 21.85643539959775694, -14.32925462369614777, -2.499999999999999112 ) ) ;
#31991 = EDGE_CURVE ( 'NONE', #37655, #22978, #19210, .T. ) ;
#31992 = CARTESIAN_POINT ( 'NONE',  ( -1.487489740686422257, -28.38776406769778760, 7.779495906702012853 ) ) ;
#31993 = ORIENTED_EDGE ( 'NONE', *, *, #23183, .T. ) ;
#31994 = DIRECTION ( 'NONE',  ( 0.000000000000000000, -0.6834397476448816899, -0.7300069255418748515 ) ) ;
#31995 = CARTESIAN_POINT ( 'NONE',  ( 68.07944445521805221, 58.24657026194513776, -3.992939643064505439 ) ) ;
#31996 = ORIENTED_EDGE ( 'NONE', *, *, #15623, .T. ) ;
#31997 = CARTESIAN_POINT ( 'NONE',  ( -0.9307968965437027897, -27.28455060704449053, 7.785593909369613819 ) ) ;
#31998 = CARTESIAN_POINT ( 'NONE',  ( 30.24633204896981198, -2.992142132496548701, 4.927069645183380864 ) ) ;
#31999 = CARTESIAN_POINT ( 'NONE',  ( 22.79610047791596728, 3.604602707705051756, 3.842052490992408753 ) ) ;
#32000 = CARTESIAN_POINT ( 'NONE',  ( 5.013941773504689614, -28.44277561705024127, 6.867280401193707640 ) ) ;
#32001 = EDGE_CURVE ( 'NONE', #23756, #11841, #32184, .T. ) ;
#32002 = EDGE_CURVE ( 'NONE', #30063, #35253, #4176, .T. ) ;
#32003 = DIRECTION ( 'NONE',  ( -1.000000000000000000, 0.000000000000000000, 0.000000000000000000 ) ) ;
#32004 = CARTESIAN_POINT ( 'NONE',  ( 1.185865733544545941, -26.10794094692920098, 6.863805608295730387 ) ) ;
#32005 = ORIENTED_EDGE ( 'NONE', *, *, #11636, .F. ) ;
#32006 = EDGE_CURVE ( 'NONE', #15320, #5482, #19807, .T. ) ;
#32007 = CARTESIAN_POINT ( 'NONE',  ( 24.40382785946252397, 3.162689046678688332, 3.275147752357558062 ) ) ;
#32008 = CARTESIAN_POINT ( 'NONE',  ( 5.021324086407805254, -24.55319635012989110, 6.800000000000000711 ) ) ;
#32009 = CARTESIAN_POINT ( 'NONE',  ( 78.65660921518627902, 66.03460256502702919, 1.194943971655634929 ) ) ;
#32010 = CARTESIAN_POINT ( 'NONE',  ( -1.311841453708477045, -31.36551672632207399, 7.255881584735163869 ) ) ;
#32011 = ORIENTED_EDGE ( 'NONE', *, *, #31024, .F. ) ;
#32012 = CARTESIAN_POINT ( 'NONE',  ( 80.13677637144074595, 61.33843513727118335, -2.660685394430965189 ) ) ;
#32014 = CARTESIAN_POINT ( 'NONE',  ( -1.712551861494080008, -28.79415494940930742, 7.011348038664006133 ) ) ;
#32013 = CARTESIAN_POINT ( 'NONE',  ( 24.73856604073376531, 0.6067268420280569341, 4.778954243596831297 ) ) ;
#32015 =( GEOMETRIC_REPRESENTATION_CONTEXT ( 3 ) GLOBAL_UNCERTAINTY_ASSIGNED_CONTEXT ( ( #9388 ) ) GLOBAL_UNIT_ASSIGNED_CONTEXT ( ( #29902, #32408, #1319 ) ) REPRESENTATION_CONTEXT ( 'NONE', 'WORKASPACE' ) );
#32016 = CARTESIAN_POINT ( 'NONE',  ( 78.68665600826857087, 66.05594492867547274, -1.065084354002965528 ) ) ;
#32017 = CARTESIAN_POINT ( 'NONE',  ( 78.59948840878007559, 65.10367658859402695, 3.015657119755321691 ) ) ;
#32018 = DIRECTION ( 'NONE',  ( 0.000000000000000000, 0.000000000000000000, 1.000000000000000000 ) ) ;
#32019 = EDGE_CURVE ( 'NONE', #31580, #36975, #14270, .T. ) ;
#32020 = CARTESIAN_POINT ( 'NONE',  ( 82.44648106056955328, 62.87232481290445918, 1.233992409460102690 ) ) ;
#32021 = CARTESIAN_POINT ( 'NONE',  ( -64.08758708074091714, 41.42074089612427912, 3.928585658033465489 ) ) ;
#32022 = DIRECTION ( 'NONE',  ( 0.1736481776669404897, -0.9848077530122062440, -0.000000000000000000 ) ) ;
#32023 = CARTESIAN_POINT ( 'NONE',  ( 24.08269697565317813, 2.216436711090640888, -5.807619368686713024 ) ) ;
#32024 = LINE ( 'NONE', #31405, #25944 ) ;
#32025 = ORIENTED_EDGE ( 'NONE', *, *, #17454, .T. ) ;
#32026 = CARTESIAN_POINT ( 'NONE',  ( -73.03051304180658576, -2.422576877779497817, 9.778627833697271399 ) ) ;
#32027 = CARTESIAN_POINT ( 'NONE',  ( 4.401417849205680355, -27.34407100962124559, 6.894806418505347700 ) ) ;
#32028 = EDGE_LOOP ( 'NONE', ( #37861, #36725, #31698, #26769, #10065, #7368, #2278 ) ) ;
#32029 = DIRECTION ( 'NONE',  ( 0.000000000000000000, 0.000000000000000000, 1.000000000000000000 ) ) ;
#32030 = ORIENTED_EDGE ( 'NONE', *, *, #13387, .F. ) ;
#32031 = CARTESIAN_POINT ( 'NONE',  ( -64.08758708074093136, 35.93730870640388275, 3.800414904976363140 ) ) ;
#32032 = CARTESIAN_POINT ( 'NONE',  ( 33.45255242130070172, -3.771379754131906736, -5.158309509446562302 ) ) ;
#32033 = CARTESIAN_POINT ( 'NONE',  ( 23.38581192113748131, 3.559989847120099249, -3.092800859860194596 ) ) ;
#32034 = CARTESIAN_POINT ( 'NONE',  ( -75.45330471031414277, 33.71485196875532608, -46.17089178453873188 ) ) ;
#32035 = CARTESIAN_POINT ( 'NONE',  ( 18.39192889356358052, 7.837295566124166335, 3.076903332958516479 ) ) ;
#32036 = DIRECTION ( 'NONE',  ( 0.01395351027862084224, -0.9999026450364577601, 0.000000000000000000 ) ) ;
#32037 = CARTESIAN_POINT ( 'NONE',  ( -0.5627839327029573457, -26.90008998972287202, 7.640616322432102869 ) ) ;
#32038 = DIRECTION ( 'NONE',  ( 0.000000000000000000, 0.000000000000000000, -1.000000000000000000 ) ) ;
#32039 = CIRCLE ( 'NONE', #22191, 0.9999999999999988898 ) ;
#32040 = DIRECTION ( 'NONE',  ( 0.000000000000000000, 1.000000000000000000, 0.000000000000000000 ) ) ;
#32041 = CARTESIAN_POINT ( 'NONE',  ( 21.77265313641114730, 1.017649519091238020, -7.447328431849799202 ) ) ;
#32042 = CARTESIAN_POINT ( 'NONE',  ( 29.60103149450674209, 1.174864541282398811, -4.249889681204039427 ) ) ;
#32043 = CARTESIAN_POINT ( 'NONE',  ( 4.984179672459081445, -25.57221830738312107, 7.695279973900954751 ) ) ;
#32044 = EDGE_LOOP ( 'NONE', ( #24463, #3433, #31337, #10689 ) ) ;
#32046 = ORIENTED_EDGE ( 'NONE', *, *, #31401, .F. ) ;
#32045 = VECTOR ( 'NONE', #32107, 1000.000000000000000 ) ;
#32047 = CARTESIAN_POINT ( 'NONE',  ( 66.55026548882318593, 57.88912323611526034, 3.999530551066472039 ) ) ;
#32048 = AXIS2_PLACEMENT_3D ( 'NONE', #28101, #40656, #18420 ) ;
#32049 = EDGE_CURVE ( 'NONE', #4500, #21616, #16500, .T. ) ;
#32050 = CIRCLE ( 'NONE', #484, 0.1000000000000028644 ) ;
#32052 = EDGE_CURVE ( 'NONE', #36134, #6701, #18244, .T. ) ;
#32051 = CARTESIAN_POINT ( 'NONE',  ( 84.76444386024292044, 2.549623173165235457, -3.635552437183829699 ) ) ;
#32053 = ORIENTED_EDGE ( 'NONE', *, *, #12883, .T. ) ;
#32054 = CARTESIAN_POINT ( 'NONE',  ( -75.56641529447675509, 8.489127916099096893, -10.26308220464040311 ) ) ;
#32055 = DIRECTION ( 'NONE',  ( 0.000000000000000000, 0.000000000000000000, 1.000000000000000000 ) ) ;
#32056 = CARTESIAN_POINT ( 'NONE',  ( 2.260952969954654446, -32.92340140904028800, 7.782167645815905033 ) ) ;
#32057 = EDGE_CURVE ( 'NONE', #28636, #11806, #18998, .T. ) ;
#32058 = LINE ( 'NONE', #3863, #14139 ) ;
#32059 = VERTEX_POINT ( 'NONE', #28674 ) ;
#32060 = PLANE ( 'NONE',  #5690 ) ;
#32061 = FACE_OUTER_BOUND ( 'NONE', #28191, .T. ) ;
#32062 = EDGE_LOOP ( 'NONE', ( #17412, #21579, #4907, #2465 ) ) ;
#32063 = CARTESIAN_POINT ( 'NONE',  ( 80.53991883815804442, 62.31343731104870898, -3.289664858626423438 ) ) ;
#32064 = CARTESIAN_POINT ( 'NONE',  ( -1.723525986837113777, -28.84815947364171151, 7.761113333116789192 ) ) ;
#32067 = ORIENTED_EDGE ( 'NONE', *, *, #39734, .T. ) ;
#32066 = ORIENTED_EDGE ( 'NONE', *, *, #17231, .F. ) ;
#32065 = CARTESIAN_POINT ( 'NONE',  ( -66.99872204295122913, 28.48507918597134037, -9.800414904976365804 ) ) ;
#32068 = DIRECTION ( 'NONE',  ( 1.000000000000000000, 0.000000000000000000, 0.000000000000000000 ) ) ;
#32069 = CARTESIAN_POINT ( 'NONE',  ( -0.5218218403989531851, -32.27395942177513888, 7.700536657684219577 ) ) ;
#32070 = LINE ( 'NONE', #13111, #4485 ) ;
#32071 = VECTOR ( 'NONE', #36336, 1000.000000000000000 ) ;
#32072 = CARTESIAN_POINT ( 'NONE',  ( 33.81879998282443722, -5.004485781189142557, -3.047669085721047111 ) ) ;
#32073 = AXIS2_PLACEMENT_3D ( 'NONE', #38930, #4968, #29673 ) ;
#32074 = CARTESIAN_POINT ( 'NONE',  ( 23.43185404716432529, 3.785464407461396341, -3.124690735438692801 ) ) ;
#32075 = ORIENTED_EDGE ( 'NONE', *, *, #7749, .F. ) ;
#32076 = CARTESIAN_POINT ( 'NONE',  ( 5.200237804508150319, -29.53704989087483668, 7.720710062488890912 ) ) ;
#32077 = CIRCLE ( 'NONE', #1825, 0.1000000000000028644 ) ;
#32078 = ORIENTED_EDGE ( 'NONE', *, *, #35521, .F. ) ;
#32079 = CARTESIAN_POINT ( 'NONE',  ( 2.325325312725053717, -33.01368626817038887, 7.750000000000001776 ) ) ;
#32080 = LINE ( 'NONE', #25678, #1793 ) ;
#32081 = CARTESIAN_POINT ( 'NONE',  ( -72.89874933986990868, 1.445529238484094980, -9.863921881214876564 ) ) ;
#32082 = PLANE ( 'NONE',  #34694 ) ;
#32083 = DIRECTION ( 'NONE',  ( 0.9848077530122080203, 0.1736481776669307198, -0.000000000000000000 ) ) ;
#32084 = CARTESIAN_POINT ( 'NONE',  ( 79.98672868146593373, 65.19218680485846562, 3.233552917234622015 ) ) ;
#32085 = CARTESIAN_POINT ( 'NONE',  ( 86.59537683758360060, -0.3992097724244685342, -5.811584838773467432 ) ) ;
#32086 = DIRECTION ( 'NONE',  ( 1.000000000000000000, 0.000000000000000000, 0.000000000000000000 ) ) ;
#32087 = CARTESIAN_POINT ( 'NONE',  ( -1.301617225954079693, -27.79589018266816680, 7.783750581861600182 ) ) ;
#32088 = B_SPLINE_CURVE_WITH_KNOTS ( 'NONE', 3,
 ( #15709, #9121, #24987, #21697, #35083, #34276, #24779, #278, #21894, #9736, #2773, #37522, #25390, #2985, #6045, #34884, #28471, #9317, #37715, #28061, #37929, #15503 ),
 .UNSPECIFIED., .F., .F.,
 ( 4, 2, 2, 2, 2, 2, 2, 2, 2, 2, 4 ),
 ( -6.342348469680895344E-05, 0.003936570167042379408, 0.007936563818781567498, 0.009936560644651162844, 0.01193655747052075992, 0.01293655588345555413, 0.01393655429639035007, 0.01493655270932514427, 0.01543655191579252316, 0.01568655151902622474, 0.01593655112225992460 ),
 .UNSPECIFIED. ) ;
#32089 = CYLINDRICAL_SURFACE ( 'NONE', #13031, 7.744449365083023729 ) ;
#32090 = CARTESIAN_POINT ( 'NONE',  ( 33.60298752457206461, -1.218802016134334920, 5.450956913170565521 ) ) ;
#32091 = B_SPLINE_CURVE_WITH_KNOTS ( 'NONE', 3,
 ( #32490, #38847, #17215, #16817, #13939, #29786, #1601, #4290, #29396, #1214, #26312, #17014, #19919, #35395, #32299, #38244, #10840, #13749, #35782, #23416, #29591, #29194, #10641, #3911, #25701, #7761, #10045, #19727, #35980, #28996, #22626 ),
 .UNSPECIFIED., .F., .F.,
 ( 4, 3, 3, 3, 3, 3, 3, 3, 3, 3, 4 ),
 ( 2.453269466693398698E-18, 3.077658087705499807E-05, 6.152638666998692973E-05, 9.267501192706385880E-05, 0.0001241882240135157561, 0.0001556618703051645773, 0.0001866161554452180210, 0.0002167966385860964666, 0.0002463805737537765679, 0.0002758761370306512975, 0.0002847094172290078680 ),
 .UNSPECIFIED. ) ;
#32092 = ORIENTED_EDGE ( 'NONE', *, *, #2506, .F. ) ;
#32093 = ADVANCED_FACE ( 'NONE', ( #884 ), #23299, .T. ) ;
#32094 = CARTESIAN_POINT ( 'NONE',  ( -63.99293516169446150, 35.89893413629674512, 7.506047544094574420 ) ) ;
#32095 = CARTESIAN_POINT ( 'NONE',  ( -0.3330542956720734526, -26.84502579658822086, 6.903372536218457256 ) ) ;
#32096 = DIRECTION ( 'NONE',  ( 0.000000000000000000, -1.000000000000000000, 0.000000000000000000 ) ) ;
#32097 = LINE ( 'NONE', #3901, #18095 ) ;
#32098 = CARTESIAN_POINT ( 'NONE',  ( 68.75960254727382903, 58.21139355255508008, 3.964410623304020831 ) ) ;
#32099 = CARTESIAN_POINT ( 'NONE',  ( 36.64607077520608414, -2.461557252482897695, 5.925903651678381401 ) ) ;
#32100 = AXIS2_PLACEMENT_3D ( 'NONE', #36116, #17545, #5420 ) ;
#32101 = DIRECTION ( 'NONE',  ( -1.000000000000000000, 0.000000000000000000, 0.000000000000000000 ) ) ;
#32103 = EDGE_CURVE ( 'NONE', #35810, #17652, #2050, .T. ) ;
#32102 = CARTESIAN_POINT ( 'NONE',  ( 85.82060591106392167, 1.959946745720340777, 4.199140470389015611 ) ) ;
#32104 = ORIENTED_EDGE ( 'NONE', *, *, #27458, .T. ) ;
#32106 = CARTESIAN_POINT ( 'NONE',  ( 0.4869470754961160996, -26.28701135364670805, 7.750000000000001776 ) ) ;
#32105 = CARTESIAN_POINT ( 'NONE',  ( 78.87101214850903830, 66.02979514927503146, -1.817988788077136375 ) ) ;
#32107 = DIRECTION ( 'NONE',  ( 0.000000000000000000, 1.000000000000000000, 0.000000000000000000 ) ) ;
#32108 = ORIENTED_EDGE ( 'NONE', *, *, #36271, .T. ) ;
#32109 = ADVANCED_FACE ( 'NONE', ( #4967 ), #20594, .F. ) ;
#32110 = PLANE ( 'NONE',  #5662 ) ;
#32111 = EDGE_CURVE ( 'NONE', #23738, #29737, #7422, .T. ) ;
#32112 = VERTEX_POINT ( 'NONE', #39128 ) ;
#32113 = CARTESIAN_POINT ( 'NONE',  ( -76.18567808263772179, -5.622137304219937626, 8.514488760352879382 ) ) ;
#32114 = EDGE_CURVE ( 'NONE', #142, #31547, #10926, .T. ) ;
#32115 = ORIENTED_EDGE ( 'NONE', *, *, #33850, .F. ) ;
#32116 = CARTESIAN_POINT ( 'NONE',  ( 81.11594168931695492, 61.32525408782629484, -1.607835478472321444 ) ) ;
#32117 = CARTESIAN_POINT ( 'NONE',  ( 5.151971482861160467, -30.15011427130464483, 7.733670252284492008 ) ) ;
#32118 = CARTESIAN_POINT ( 'NONE',  ( 23.32705478529917187, 2.029264981615857444, 4.738981897168647706 ) ) ;
#32120 = VERTEX_POINT ( 'NONE', #7847 ) ;
#32119 = EDGE_LOOP ( 'NONE', ( #25164, #4812, #31022, #15820 ) ) ;
#32121 = CARTESIAN_POINT ( 'NONE',  ( -6.348748702180634140, -26.64985754041175525, 6.700000000000000178 ) ) ;
#32122 =( BOUNDED_CURVE ( )  B_SPLINE_CURVE ( 3, ( #26650, #35925, #39386, #32836 ),
 .UNSPECIFIED., .F., .T. ) 
 B_SPLINE_CURVE_WITH_KNOTS ( ( 4, 4 ),
 ( 4.748221474220560623, 4.941946782021394924 ),
 .UNSPECIFIED. ) 
 CURVE ( )  GEOMETRIC_REPRESENTATION_ITEM ( )  RATIONAL_B_SPLINE_CURVE ( ( 1.000000000000000000, 0.9968749865767494445, 0.9968749865767494445, 1.000000000000000000 ) ) 
 REPRESENTATION_ITEM ( '' )  );
#32123 = VECTOR ( 'NONE', #39008, 1000.000000000000000 ) ;
#32125 = CARTESIAN_POINT ( 'NONE',  ( 86.44490267695917396, 1.258706987354809348, 4.883621451348188813 ) ) ;
#32124 = CARTESIAN_POINT ( 'NONE',  ( 14.74978830686065301, 12.47633826711700600, -2.508459208900547743 ) ) ;
#32126 = CARTESIAN_POINT ( 'NONE',  ( -4.248748702180636272, -25.49307895267003587, 6.800000000000000711 ) ) ;
#32127 = CARTESIAN_POINT ( 'NONE',  ( -63.47040772160210054, 43.09577237655619797, -3.381599148487555162 ) ) ;
#32128 = CARTESIAN_POINT ( 'NONE',  ( 70.60245471852235255, 60.31942058782808402, 3.837797619696055929 ) ) ;
#32129 = ORIENTED_EDGE ( 'NONE', *, *, #26681, .F. ) ;
#32130 = B_SPLINE_CURVE_WITH_KNOTS ( 'NONE', 3,
 ( #10359, #16717, #29307, #32607, #38549, #9952 ),
 .UNSPECIFIED., .F., .F.,
 ( 4, 2, 4 ),
 ( 0.000000000000000000, 0.001088541862127112049, 0.002177083724254224098 ),
 .UNSPECIFIED. ) ;
#32131 = CARTESIAN_POINT ( 'NONE',  ( 22.21620953772258744, 3.796930799149246472, -4.142915743477519896 ) ) ;
#32132 = ORIENTED_EDGE ( 'NONE', *, *, #23306, .T. ) ;
#32133 = ORIENTED_EDGE ( 'NONE', *, *, #18114, .T. ) ;
#32134 = CARTESIAN_POINT ( 'NONE',  ( 21.85643539959778181, 1.552649203755968488, -12.31912549844641447 ) ) ;
#32135 = CARTESIAN_POINT ( 'NONE',  ( 21.76122352785010605, 6.560793838968803193, 3.350653129119654405 ) ) ;
#32136 = CARTESIAN_POINT ( 'NONE',  ( 1.128064129311358244, -33.02281926226938680, 7.695279973900954751 ) ) ;
#32137 = CARTESIAN_POINT ( 'NONE',  ( 81.64294641038151212, 62.46883698080834790, 2.647945256410963566 ) ) ;
#32138 = CARTESIAN_POINT ( 'NONE',  ( 87.43361094620441065, 0.1481429324132612357, -5.028924837761966415 ) ) ;
#32139 = EDGE_LOOP ( 'NONE', ( #18298, #1174, #12599, #21981 ) ) ;
#32140 = CARTESIAN_POINT ( 'NONE',  ( 2.731683849345822424, -32.91454274520125267, 7.006908160621413195 ) ) ;
#32141 = AXIS2_PLACEMENT_3D ( 'NONE', #4038, #18844, #6904 ) ;
#32142 = VERTEX_POINT ( 'NONE', #2670 ) ;
#32143 = CARTESIAN_POINT ( 'NONE',  ( 14.60763624620907919, -5.047772731472147889, 2.486272941875335984 ) ) ;
#32144 = CARTESIAN_POINT ( 'NONE',  ( 33.05017804490641709, -3.814651194816198743, 5.008230371610723708 ) ) ;
#32145 = CARTESIAN_POINT ( 'NONE',  ( 21.25451605427406676, 3.323545792246858976, -3.523679291319553375 ) ) ;
#32146 = LINE ( 'NONE', #6807, #4946 ) ;
#32147 = CARTESIAN_POINT ( 'NONE',  ( -42.24874870218063450, -26.64985754041175525, 6.800000000000000711 ) ) ;
#32148 = ORIENTED_EDGE ( 'NONE', *, *, #22949, .F. ) ;
#32149 = PRODUCT_DEFINITION ( 'UNKNOWN', '', #18247, #31644 ) ;
#32150 = CARTESIAN_POINT ( 'NONE',  ( -12.97867591359219297, -26.64985754041175525, 6.700000000000000178 ) ) ;
#32151 = CARTESIAN_POINT ( 'NONE',  ( 28.39362077150625296, -3.972643944815215988, 4.268989596475896597 ) ) ;
#32152 = VECTOR ( 'NONE', #9315, 1000.000000000000000 ) ;
#32153 = ORIENTED_EDGE ( 'NONE', *, *, #13097, .F. ) ;
#32154 = ORIENTED_EDGE ( 'NONE', *, *, #28790, .T. ) ;
#32155 = CARTESIAN_POINT ( 'NONE',  ( 34.63654108703977386, -0.7829625105204697233, 5.276317761283050523 ) ) ;
#32156 = DIRECTION ( 'NONE',  ( -0.4999999999999927836, -0.8660254037844429265, 0.000000000000000000 ) ) ;
#32157 = CARTESIAN_POINT ( 'NONE',  ( 66.42099604079466246, 57.79375748135241508, -4.000000000000017764 ) ) ;
#32158 = CARTESIAN_POINT ( 'NONE',  ( 87.33285498545190251, -1.784623943069521435, 4.108613016059194045 ) ) ;
#32159 = EDGE_CURVE ( 'NONE', #20726, #34939, #33179, .T. ) ;
#32160 = ORIENTED_EDGE ( 'NONE', *, *, #15855, .T. ) ;
#32161 = EDGE_CURVE ( 'NONE', #6354, #2342, #36069, .T. ) ;
#32162 = DIRECTION ( 'NONE',  ( 0.6427876096865379196, 0.7660444431189792347, -0.000000000000000000 ) ) ;
#32163 = ORIENTED_EDGE ( 'NONE', *, *, #22057, .T. ) ;
#32164 = FACE_BOUND ( 'NONE', #21051, .T. ) ;
#32165 = CARTESIAN_POINT ( 'NONE',  ( 3.817505324021141622, -32.35701164965254861, 6.895394898881671786 ) ) ;
#32166 = ORIENTED_EDGE ( 'NONE', *, *, #18840, .T. ) ;
#32167 = CARTESIAN_POINT ( 'NONE',  ( 81.88767907424660564, 65.09350295521461760, -2.164558651854042282 ) ) ;
#32168 = CARTESIAN_POINT ( 'NONE',  ( 2.938587699976823675, -26.40339382889528608, 7.782034975670474530 ) ) ;
#32169 = ORIENTED_EDGE ( 'NONE', *, *, #35632, .T. ) ;
#32170 = CARTESIAN_POINT ( 'NONE',  ( 76.01163379375532259, 60.38783671147731980, -3.615102801931016074 ) ) ;
#32172 = CARTESIAN_POINT ( 'NONE',  ( 4.376572504284961695, -27.31639088417337646, 7.762796336881261361 ) ) ;
#32171 = CARTESIAN_POINT ( 'NONE',  ( -1.689549538493119174, -29.22836755717258228, 7.505001789837627335 ) ) ;
#32173 = FACE_OUTER_BOUND ( 'NONE', #32224, .T. ) ;
#32174 = CARTESIAN_POINT ( 'NONE',  ( 76.68479537131447898, 60.43247505492697513, 3.462570962778594552 ) ) ;
#32175 = ORIENTED_EDGE ( 'NONE', *, *, #7526, .F. ) ;
#32176 = CARTESIAN_POINT ( 'NONE',  ( 4.351715999300050264, -27.44141758656811092, 6.874555630061444766 ) ) ;
#32177 = CARTESIAN_POINT ( 'NONE',  ( 1.735750141597346863, -26.08309558226786962, 7.783750581861601070 ) ) ;
#32178 = AXIS2_PLACEMENT_3D ( 'NONE', #19136, #30896, #28399 ) ;
#32179 = CARTESIAN_POINT ( 'NONE',  ( -0.9146243593313261311, -25.28420110832643886, 7.754798119455333705 ) ) ;
#32180 = CARTESIAN_POINT ( 'NONE',  ( 82.04158296082421487, 62.38656886254267420, 2.040045296073324632 ) ) ;
#32181 = CARTESIAN_POINT ( 'NONE',  ( 4.224974933773748553, -31.84731275619759927, 7.754798119455333705 ) ) ;
#32182 = CARTESIAN_POINT ( 'NONE',  ( 28.36395155556995817, 1.046816072451675517, -4.961098188302698553 ) ) ;
#32183 = DIRECTION ( 'NONE',  ( 0.9396926207859112035, -0.3420201433256609413, 0.000000000000000000 ) ) ;
#32184 = LINE ( 'NONE', #16901, #14990 ) ;
#32185 = CARTESIAN_POINT ( 'NONE',  ( -34.97867591359219830, -26.64985754041175525, 6.800000000000000711 ) ) ;
#32186 = VERTEX_POINT ( 'NONE', #15395 ) ;
#32187 = CARTESIAN_POINT ( 'NONE',  ( 0.7364210922827194583, -26.30944492956864877, 6.969307238440507035 ) ) ;
#32188 = DIRECTION ( 'NONE',  ( 0.000000000000000000, 0.000000000000000000, 1.000000000000000000 ) ) ;
#32189 = CARTESIAN_POINT ( 'NONE',  ( 37.02986127830654084, -2.495646223213518144, -5.974012795379922025 ) ) ;
#32190 = DIRECTION ( 'NONE',  ( 0.000000000000000000, 0.000000000000000000, 1.000000000000000000 ) ) ;
#32191 = DIRECTION ( 'NONE',  ( -0.9848077530122091305, 0.1736481776669241417, -0.000000000000000000 ) ) ;
#32192 = CARTESIAN_POINT ( 'NONE',  ( 3.421732255662511601, -32.50199707566237350, 7.740055089680399902 ) ) ;
#32193 = CARTESIAN_POINT ( 'NONE',  ( 2.208439051597432812, -32.93175799812527771, 6.870716933885664623 ) ) ;
#32194 = CARTESIAN_POINT ( 'NONE',  ( -8.295002936191391285, 28.24537450226321411, 2.500000000000000000 ) ) ;
#32195 = AXIS2_PLACEMENT_3D ( 'NONE', #17706, #2100, #27192 ) ;
#32196 = EDGE_CURVE ( 'NONE', #22737, #2057, #11776, .T. ) ;
#32197 = CARTESIAN_POINT ( 'NONE',  ( -1.456121751345974547, -28.30640807203716491, 7.768425012602593327 ) ) ;
#32198 = ORIENTED_EDGE ( 'NONE', *, *, #27334, .T. ) ;
#32199 = ORIENTED_EDGE ( 'NONE', *, *, #22001, .T. ) ;
#32200 = FACE_OUTER_BOUND ( 'NONE', #5742, .T. ) ;
#32201 = CARTESIAN_POINT ( 'NONE',  ( 68.63113683135277654, 58.55076364936792288, -3.993768376023898448 ) ) ;
#32202 = CARTESIAN_POINT ( 'NONE',  ( -1.339380734913657500, -27.83505459351727396, 7.750000000000002665 ) ) ;
#32203 = ORIENTED_EDGE ( 'NONE', *, *, #29299, .T. ) ;
#32204 = FACE_OUTER_BOUND ( 'NONE', #37819, .T. ) ;
#32206 = EDGE_CURVE ( 'NONE', #34818, #37831, #23521, .T. ) ;
#32205 = CARTESIAN_POINT ( 'NONE',  ( -43.84925787048184986, -39.21126558444150589, 9.800414904976365804 ) ) ;
#32207 = CARTESIAN_POINT ( 'NONE',  ( 24.13130278612604940, 2.937171867363354227, 3.784435561684969418 ) ) ;
#32208 = CARTESIAN_POINT ( 'NONE',  ( -70.92837671539291478, 0.2169278822316458022, 3.999987187540717137 ) ) ;
#32209 = CARTESIAN_POINT ( 'NONE',  ( 1.198593767960137946, -26.20716339874380907, 7.778050822775631090 ) ) ;
#32210 = CARTESIAN_POINT ( 'NONE',  ( 1.216825644920784377, -26.10348059021085376, 6.867199677474203234 ) ) ;
#32211 = VERTEX_POINT ( 'NONE', #786 ) ;
#32212 = DIRECTION ( 'NONE',  ( -0.9999026450364576490, -0.01395351027862084224, 0.000000000000000000 ) ) ;
#32213 = CARTESIAN_POINT ( 'NONE',  ( 81.25428736789773154, 61.63226232517330061, 2.112861953993775632 ) ) ;
#32214 = ORIENTED_EDGE ( 'NONE', *, *, #12515, .T. ) ;
#32215 = CARTESIAN_POINT ( 'NONE',  ( 79.97179536941432332, 60.87748285318664898, -2.061059937946318144 ) ) ;
#32217 = CARTESIAN_POINT ( 'NONE',  ( -1.709192382262307852, -28.77952057895107885, 6.985875436432904095 ) ) ;
#32216 = CARTESIAN_POINT ( 'NONE',  ( 21.99573204474387467, 0.2403451770729164994, 7.663175214092573739 ) ) ;
#32218 = CARTESIAN_POINT ( 'NONE',  ( 78.88661621011567604, 66.15061626711307952, -1.323744132979592925 ) ) ;
#32219 = CARTESIAN_POINT ( 'NONE',  ( 78.20000946334697289, 65.71092203236408125, 1.748505333477076373 ) ) ;
#32220 = ORIENTED_EDGE ( 'NONE', *, *, #15940, .T. ) ;
#32221 = CARTESIAN_POINT ( 'NONE',  ( -4.978675913592189417, -26.64985754041175525, 6.700000000000000178 ) ) ;
#32222 = CARTESIAN_POINT ( 'NONE',  ( 81.60972716517463255, 65.70321483603510160, 1.303631908148715990 ) ) ;
#32224 = EDGE_LOOP ( 'NONE', ( #11682, #10378, #8638, #6028 ) ) ;
#32223 = CARTESIAN_POINT ( 'NONE',  ( -64.08758708074093136, 44.09647857119033176, 1.198844121191492196 ) ) ;
#32225 = CARTESIAN_POINT ( 'NONE',  ( 24.99136039731803294, -2.601164552868876267, 6.036718378868273227 ) ) ;
#32226 = EDGE_CURVE ( 'NONE', #33153, #24052, #16746, .T. ) ;
#32227 = CARTESIAN_POINT ( 'NONE',  ( -63.48867051204953782, 35.67471974816380964, -6.899503081314764863 ) ) ;
#32228 = ORIENTED_EDGE ( 'NONE', *, *, #37782, .F. ) ;
#32229 = CARTESIAN_POINT ( 'NONE',  ( -74.30460642558605855, -2.214477923546239957, 10.70245808945297661 ) ) ;
#32230 = CARTESIAN_POINT ( 'NONE',  ( -62.92837670882106238, -52.49535338866468948, -6.000000000000000000 ) ) ;
#32231 = CARTESIAN_POINT ( 'NONE',  ( -16.34874870218063592, -25.49307895267003587, 6.700000000000000178 ) ) ;
#32232 = B_SPLINE_CURVE_WITH_KNOTS ( 'NONE', 3,
 ( #22090, #30952, #18563, #21474, #3179, #31149, #34257, #24758, #34456, #22299 ),
 .UNSPECIFIED., .F., .F.,
 ( 4, 3, 3, 4 ),
 ( 0.0002170292169044720702, 0.0002420761345915905356, 0.0002723302478206952697, 0.0002816811360866739822 ),
 .UNSPECIFIED. ) ;
#32233 = CARTESIAN_POINT ( 'NONE',  ( -66.99872204295122913, 28.48507918597134037, 6.999999999999999112 ) ) ;
#32234 = CIRCLE ( 'NONE', #11814, 2.500000000000002220 ) ;
#32235 = VERTEX_POINT ( 'NONE', #19513 ) ;
#32236 = CARTESIAN_POINT ( 'NONE',  ( 36.20073155144311272, -3.649434425297155116, -5.718600478983131730 ) ) ;
#32237 = SURFACE_STYLE_FILL_AREA ( #26253 ) ;
#32238 = DIRECTION ( 'NONE',  ( -0.7055275666422137215, -0.2567910337120389297, 0.6605219282605379050 ) ) ;
#32239 = CARTESIAN_POINT ( 'NONE',  ( 17.35308537373412108, 8.839742678962347000, 2.914766677163659558 ) ) ;
#32240 = DIRECTION ( 'NONE',  ( 0.9999026450364576490, 0.01395351027862084051, 0.000000000000000000 ) ) ;
#32241 = CARTESIAN_POINT ( 'NONE',  ( -4.890026461918809630, -25.50263309590217276, 27.90461065042423527 ) ) ;
#32242 = EDGE_CURVE ( 'NONE', #38497, #15627, #563, .T. ) ;
#32243 = CARTESIAN_POINT ( 'NONE',  ( 3.472881818119431863, -32.58792320592009162, 7.737115613922532553 ) ) ;
#32244 = B_SPLINE_CURVE_WITH_KNOTS ( 'NONE', 3,
 ( #3013, #2801, #40425, #25219, #12645, #9345, #15325, #38159, #40641, #6487 ),
 .UNSPECIFIED., .F., .F.,
 ( 4, 3, 3, 4 ),
 ( 0.0001585009270395785694, 0.0001815657551981846821, 0.0002118214035944131018, 0.0002170292169044822075 ),
 .UNSPECIFIED. ) ;
#32245 = EDGE_CURVE ( 'NONE', #24852, #38011, #28822, .T. ) ;
#32246 = ADVANCED_FACE ( 'NONE', ( #15604 ), #32089, .T. ) ;
#32247 = DIRECTION ( 'NONE',  ( 0.000000000000000000, -1.000000000000000000, 0.000000000000000000 ) ) ;
#32248 = CARTESIAN_POINT ( 'NONE',  ( 23.87443714975944431, 1.367339853345398426, -4.872535488811999826 ) ) ;
#32249 = CARTESIAN_POINT ( 'NONE',  ( 35.49974038668526077, -1.192779227918109086, -5.483795844434342648 ) ) ;
#32250 = DIRECTION ( 'NONE',  ( 1.385724075720358314E-16, -1.000000000000000000, 0.000000000000000000 ) ) ;
#32251 = ORIENTED_EDGE ( 'NONE', *, *, #15845, .F. ) ;
#32252 = CARTESIAN_POINT ( 'NONE',  ( 86.28404140065768502, 0.1054103399587360407, 6.008803426180587159 ) ) ;
#32253 = ADVANCED_FACE ( 'NONE', ( #6756 ), #31628, .F. ) ;
#32254 = ORIENTED_EDGE ( 'NONE', *, *, #33048, .T. ) ;
#32255 = CARTESIAN_POINT ( 'NONE',  ( -81.82457292829037954, 10.46020204711655843, -0.1745755204938225225 ) ) ;
#32256 = PRODUCT_CONTEXT ( 'NONE', #11825, 'mechanical' ) ;
#32257 = DIRECTION ( 'NONE',  ( 1.000000000000000000, 0.000000000000000000, 0.000000000000000000 ) ) ;
#32258 = DIRECTION ( 'NONE',  ( -0.000000000000000000, -1.000000000000000000, -0.000000000000000000 ) ) ;
#32259 = VERTEX_POINT ( 'NONE', #10027 ) ;
#32260 = CARTESIAN_POINT ( 'NONE',  ( 3.968771540420744870, -26.92158891409267696, 7.783750581861600182 ) ) ;
#32261 = EDGE_LOOP ( 'NONE', ( #22128, #15737 ) ) ;
#32262 = CIRCLE ( 'NONE', #25017, 0.1000000000000028644 ) ;
#32263 = ORIENTED_EDGE ( 'NONE', *, *, #40430, .F. ) ;
#32264 = CARTESIAN_POINT ( 'NONE',  ( 78.83205648568244328, 65.58035453618786903, -2.615973384261010448 ) ) ;
#32265 = CARTESIAN_POINT ( 'NONE',  ( 80.85043593073658030, 61.68942038033306829, 2.615973384260630308 ) ) ;
#32267 = ORIENTED_EDGE ( 'NONE', *, *, #17105, .F. ) ;
#32266 = DIRECTION ( 'NONE',  ( -0.000000000000000000, -0.000000000000000000, -1.000000000000000000 ) ) ;
#32268 = ADVANCED_FACE ( 'NONE', ( #25889 ), #34371, .F. ) ;
#32269 = CARTESIAN_POINT ( 'NONE',  ( 27.40513141245228468, 1.065180075448391772, 4.483631571157760121 ) ) ;
#32270 = CARTESIAN_POINT ( 'NONE',  ( 27.37917897173983661, -4.430804881127424544, 3.681097677848294669 ) ) ;
#32271 = CARTESIAN_POINT ( 'NONE',  ( 3.757339589042690164, -26.85389010558039757, 7.139196562012272373 ) ) ;
#32272 = CARTESIAN_POINT ( 'NONE',  ( 21.85643539959773207, -2.612013071670181041, -15.99649826491319971 ) ) ;
#32273 = CARTESIAN_POINT ( 'NONE',  ( 24.04917647243221879, 3.336295066126922393, -3.255249733571578652 ) ) ;
#32274 = ORIENTED_EDGE ( 'NONE', *, *, #17278, .T. ) ;
#32275 = CARTESIAN_POINT ( 'NONE',  ( 5.200346647029098435, -29.55249110255828882, 7.749999999999999112 ) ) ;
#32276 = ORIENTED_EDGE ( 'NONE', *, *, #21391, .T. ) ;
#32277 = CARTESIAN_POINT ( 'NONE',  ( -4.266520354791871306, -48.67644278316300444, -2.500000000000000444 ) ) ;
#32278 = DIRECTION ( 'NONE',  ( 0.000000000000000000, 0.000000000000000000, -1.000000000000000000 ) ) ;
#32279 = CARTESIAN_POINT ( 'NONE',  ( -76.09606208423944906, -4.068416357244072579, -8.586815735137202310 ) ) ;
#32280 = FACE_OUTER_BOUND ( 'NONE', #37130, .T. ) ;
#32281 = CARTESIAN_POINT ( 'NONE',  ( -2.383717838810009759, -31.00696599979863066, 6.954324564059724878 ) ) ;
#32282 = CARTESIAN_POINT ( 'NONE',  ( 81.37039951255474080, 61.83949519909547377, 2.349509806045097182 ) ) ;
#32283 = CARTESIAN_POINT ( 'NONE',  ( 85.92174427069515730, 0.4035765525155806666, 6.008818417626160979 ) ) ;
#32284 = DIRECTION ( 'NONE',  ( 0.000000000000000000, 0.000000000000000000, 1.000000000000000000 ) ) ;
#32285 = CARTESIAN_POINT ( 'NONE',  ( -1.321461783636408649, -27.81506318992830984, 7.773839561854630986 ) ) ;
#32286 = CARTESIAN_POINT ( 'NONE',  ( 3.933165243051754523, -26.87461258339965298, 7.743886751744253338 ) ) ;
#32287 = EDGE_CURVE ( 'NONE', #774, #12399, #31468, .T. ) ;
#32288 =( BOUNDED_CURVE ( )  B_SPLINE_CURVE ( 3, ( #24894, #22223, #28590, #12937 ),
 .UNSPECIFIED., .F., .T. ) 
 B_SPLINE_CURVE_WITH_KNOTS ( ( 4, 4 ),
 ( 3.394272908731871485, 3.785093762383077820 ),
 .UNSPECIFIED. ) 
 CURVE ( )  GEOMETRIC_REPRESENTATION_ITEM ( )  RATIONAL_B_SPLINE_CURVE ( ( 1.000000000000000000, 0.9873120399594201846, 0.9873120399594201846, 1.000000000000000000 ) ) 
 REPRESENTATION_ITEM ( '' )  );
#32289 = EDGE_CURVE ( 'NONE', #29356, #27310, #12921, .T. ) ;
#32290 = FACE_OUTER_BOUND ( 'NONE', #18292, .T. ) ;
#32291 = CARTESIAN_POINT ( 'NONE',  ( -0.3716677413943337838, -26.87427139008162058, 6.868387053540520704 ) ) ;
#32292 = CARTESIAN_POINT ( 'NONE',  ( 4.688732775102122829, -27.94826190174027047, 7.778050822775631090 ) ) ;
#32293 = FACE_OUTER_BOUND ( 'NONE', #4, .T. ) ;
#32294 = CARTESIAN_POINT ( 'NONE',  ( 68.42229528291726126, 59.10113456467039583, 3.941639393089738874 ) ) ;
#32295 = CARTESIAN_POINT ( 'NONE',  ( 36.97963125324073275, -2.956583467688224776, 5.977963831466492906 ) ) ;
#32296 = LINE ( 'NONE', #17212, #13508 ) ;
#32297 = CARTESIAN_POINT ( 'NONE',  ( 87.11756278340992310, 0.5031432294147388795, -4.836983121871330837 ) ) ;
#32299 = CARTESIAN_POINT ( 'NONE',  ( -0.4222643637383041715, -26.78705640903759644, 6.887547729233686411 ) ) ;
#32298 = CARTESIAN_POINT ( 'NONE',  ( 81.19854122754009040, 61.34870327520655309, -1.508787936435542099 ) ) ;
#32300 = EDGE_CURVE ( 'NONE', #21657, #1177, #18207, .T. ) ;
#32301 = DIRECTION ( 'NONE',  ( 0.4826092789263541349, 0.5751513419797977811, -0.6605219282605403475 ) ) ;
#32302 = CARTESIAN_POINT ( 'NONE',  ( 4.371499634827735292, -27.30825421931019648, 7.638132480492517473 ) ) ;
#32303 = ORIENTED_EDGE ( 'NONE', *, *, #3163, .F. ) ;
#32304 = AXIS2_PLACEMENT_3D ( 'NONE', #32150, #28010, #40557 ) ;
#32305 = DIRECTION ( 'NONE',  ( 0.000000000000000000, 0.000000000000000000, -1.000000000000000000 ) ) ;
#32306 = ORIENTED_EDGE ( 'NONE', *, *, #16362, .T. ) ;
#32307 = CARTESIAN_POINT ( 'NONE',  ( -80.82372619930970359, -6.607616770128094785, 1.502042499036972734 ) ) ;
#32308 = VERTEX_POINT ( 'NONE', #17002 ) ;
#32309 = CARTESIAN_POINT ( 'NONE',  ( 80.83002518733226793, 62.39751428130106348, -3.213872034465284244 ) ) ;
#32310 = DIRECTION ( 'NONE',  ( 1.000000000000000000, -0.000000000000000000, 0.000000000000000000 ) ) ;
#32311 = CARTESIAN_POINT ( 'NONE',  ( 23.15964026960165967, 1.239783467617344037, 5.376747259291860814 ) ) ;
#32313 = EDGE_LOOP ( 'NONE', ( #29021, #25526, #11242, #14793 ) ) ;
#32312 = ORIENTED_EDGE ( 'NONE', *, *, #3716, .T. ) ;
#32314 = LINE ( 'NONE', #817, #34760 ) ;
#32315 = AXIS2_PLACEMENT_3D ( 'NONE', #20718, #39243, #24426 ) ;
#32316 = CARTESIAN_POINT ( 'NONE',  ( 5.036944646152517358, -30.22373891335575635, 6.880147297696979969 ) ) ;
#32318 = CARTESIAN_POINT ( 'NONE',  ( 85.15051256642057353, 2.712627394972505268, -0.4824498372492339593 ) ) ;
#32317 = CARTESIAN_POINT ( 'NONE',  ( 4.559135941322734809, -31.41048459562103545, 6.876076431790004939 ) ) ;
#32319 = CARTESIAN_POINT ( 'NONE',  ( 1.700390093233090871, -29.56993018339339940, 7.750000000000000888 ) ) ;
#32320 = CARTESIAN_POINT ( 'NONE',  ( 71.82805326594559858, 60.58951223549524201, 3.882941974849172695 ) ) ;
#32321 = B_SPLINE_CURVE_WITH_KNOTS ( 'NONE', 3,
 ( #13026, #40613, #16116, #31572, #3397, #87, #12817, #38328, #34885, #22716, #18581, #9319, #2987, #6248, #37524, #12618, #28472, #15505, #12418, #28882, #3592, #31370, #19211, #22316, #6659 ),
 .UNSPECIFIED., .F., .F.,
 ( 4, 3, 3, 3, 3, 3, 3, 3, 4 ),
 ( 6.468151674593860048E-05, 9.076621574722655312E-05, 0.0001210204262068023304, 0.0001512763324577563588, 0.0001815301820994311068, 0.0002117781465860803008, 0.0002420274594459839897, 0.0002722905548971226190, 0.0002816827545175647511 ),
 .UNSPECIFIED. ) ;
#32322 = ORIENTED_EDGE ( 'NONE', *, *, #39527, .F. ) ;
#32323 = CARTESIAN_POINT ( 'NONE',  ( 22.20600778403895248, 3.972696832848836124, -4.026605987857512226 ) ) ;
#32324 = ORIENTED_EDGE ( 'NONE', *, *, #24184, .F. ) ;
#32325 = ADVANCED_FACE ( 'NONE', ( #29578 ), #7151, .F. ) ;
#32326 = ORIENTED_EDGE ( 'NONE', *, *, #20262, .T. ) ;
#32327 = CARTESIAN_POINT ( 'NONE',  ( 21.85643539959775694, 5.081979399238238493, 12.23420521612613143 ) ) ;
#32328 = EDGE_CURVE ( 'NONE', #2177, #24757, #30495, .T. ) ;
#32329 = CARTESIAN_POINT ( 'NONE',  ( 18.10407751945326638, 13.71956107779235268, -3.198739209383718585 ) ) ;
#32330 = ORIENTED_EDGE ( 'NONE', *, *, #36524, .F. ) ;
#32331 = CARTESIAN_POINT ( 'NONE',  ( 0.4918310210129015481, -32.74788313599579936, 6.894806418505344148 ) ) ;
#32332 = CARTESIAN_POINT ( 'NONE',  ( 80.63952753653605043, 65.18836132072121359, 3.079343812564430127 ) ) ;
#32333 = CARTESIAN_POINT ( 'NONE',  ( 86.63338141420044280, 0.5786414684654883622, -5.958757720264261870 ) ) ;
#32334 = CARTESIAN_POINT ( 'NONE',  ( -1.796469343894664394, -29.56974349003418112, 7.767441775592068609 ) ) ;
#32335 = ORIENTED_EDGE ( 'NONE', *, *, #7909, .F. ) ;
#32336 = EDGE_CURVE ( 'NONE', #36841, #18445, #36883, .T. ) ;
#32337 = CARTESIAN_POINT ( 'NONE',  ( 33.11221513172080932, -3.162643624533764353, 5.374360011888029476 ) ) ;
#32338 = CARTESIAN_POINT ( 'NONE',  ( 30.31286271484965766, -3.794529559310727329, 4.460666598210623057 ) ) ;
#32339 = ADVANCED_FACE ( 'NONE', ( #7547 ), #10825, .F. ) ;
#32340 = CARTESIAN_POINT ( 'NONE',  ( 31.37671975378950151, -3.077845645974021771, -5.103493985049731840 ) ) ;
#32341 = CARTESIAN_POINT ( 'NONE',  ( 29.10125458543393862, 0.3582796436202419499, -4.748352613195486960 ) ) ;
#32342 = CARTESIAN_POINT ( 'NONE',  ( 5.166053052204034657, -29.08252373668924307, 7.754798119455333705 ) ) ;
#32343 = CARTESIAN_POINT ( 'NONE',  ( 84.19306202100948155, 2.904934786060358487, -1.717472329190754543 ) ) ;
#32344 = DIRECTION ( 'NONE',  ( 0.000000000000000000, 1.000000000000000000, 0.000000000000000000 ) ) ;
#32345 = CARTESIAN_POINT ( 'NONE',  ( 9.703489126596464232, 56.50623631086179444, -1.000000000000000000 ) ) ;
#32346 = AXIS2_PLACEMENT_3D ( 'NONE', #10893, #23471, #8007 ) ;
#32347 = CARTESIAN_POINT ( 'NONE',  ( 33.43971231075012440, -3.588053834546123255, 5.336497937005737491 ) ) ;
#32348 = ORIENTED_EDGE ( 'NONE', *, *, #3214, .T. ) ;
#32349 = VERTEX_POINT ( 'NONE', #16600 ) ;
#32350 = CARTESIAN_POINT ( 'NONE',  ( 33.45677177907953848, -3.832870168856042703, 5.089957537689628886 ) ) ;
#32351 = CARTESIAN_POINT ( 'NONE',  ( 4.748301322462879170, -28.04738229536728156, 7.386948897581448570 ) ) ;
#32352 = DIRECTION ( 'NONE',  ( 1.000000000000000000, 0.000000000000000000, 0.000000000000000000 ) ) ;
#32353 = CARTESIAN_POINT ( 'NONE',  ( 87.44940651735645076, -1.930920027091641122, 3.725338843608501094 ) ) ;
#32354 = VERTEX_POINT ( 'NONE', #23401 ) ;
#32355 = CARTESIAN_POINT ( 'NONE',  ( -64.08758708074093136, 38.13199975834722721, -3.043809435734133650 ) ) ;
#32356 =( NAMED_UNIT ( * ) SI_UNIT ( $, .STERADIAN. ) SOLID_ANGLE_UNIT ( ) );
#32357 =( BOUNDED_CURVE ( )  B_SPLINE_CURVE ( 3, ( #32535, #13786, #22317, #10879 ),
 .UNSPECIFIED., .F., .T. ) 
 B_SPLINE_CURVE_WITH_KNOTS ( ( 4, 4 ),
 ( 1.570796326794894560, 1.718934167276706892 ),
 .UNSPECIFIED. ) 
 CURVE ( )  GEOMETRIC_REPRESENTATION_ITEM ( )  RATIONAL_B_SPLINE_CURVE ( ( 1.000000000000000000, 0.9981721009331441241, 0.9981721009331441241, 1.000000000000000000 ) ) 
 REPRESENTATION_ITEM ( '' )  );
#32358 = VERTEX_POINT ( 'NONE', #23010 ) ;
#32359 = DIRECTION ( 'NONE',  ( 0.000000000000000000, 0.000000000000000000, 1.000000000000000000 ) ) ;
#32360 = ORIENTED_EDGE ( 'NONE', *, *, #30227, .F. ) ;
#32361 = CARTESIAN_POINT ( 'NONE',  ( 82.21758965863715218, 62.47540435105895540, -1.725837398063455819 ) ) ;
#32362 = CARTESIAN_POINT ( 'NONE',  ( 4.460814650971867579, -27.41817363093848314, 7.750000000000000888 ) ) ;
#32363 = ORIENTED_EDGE ( 'NONE', *, *, #27168, .F. ) ;
#32364 = CARTESIAN_POINT ( 'NONE',  ( 74.85245598970902847, 62.88263772385705153, -3.424891502433893287 ) ) ;
#32366 = DIRECTION ( 'NONE',  ( 0.000000000000000000, 0.000000000000000000, -1.000000000000000000 ) ) ;
#32365 = CARTESIAN_POINT ( 'NONE',  ( -1.595110958568865422, -28.39108633556104522, 7.643192810543823157 ) ) ;
#32367 = CARTESIAN_POINT ( 'NONE',  ( 2.881058359821971226, -26.27508231979332010, 7.750000000000000000 ) ) ;
#32368 = CARTESIAN_POINT ( 'NONE',  ( 77.90315483005272768, 60.81789388943186481, 3.308002540436142169 ) ) ;
#32369 = ORIENTED_EDGE ( 'NONE', *, *, #20263, .T. ) ;
#32370 = CYLINDRICAL_SURFACE ( 'NONE', #24076, 0.1000000000000028644 ) ;
#32371 = CARTESIAN_POINT ( 'NONE',  ( 5.196299276553091318, -29.73910164073445017, 7.013842709614101167 ) ) ;
#32372 = CARTESIAN_POINT ( 'NONE',  ( 25.83191277475825132, 1.872540234882475785, -4.238092754309072951 ) ) ;
#32373 = CARTESIAN_POINT ( 'NONE',  ( -53.21549048184568420, -30.38627270959228710, 6.000000000000000000 ) ) ;
#32374 = CARTESIAN_POINT ( 'NONE',  ( 79.82775505260907778, 66.24998868310150613, 1.780213741554581786 ) ) ;
#32375 = CARTESIAN_POINT ( 'NONE',  ( -0.9597769704937348934, -31.84446556299579001, 7.670465701733750308 ) ) ;
#32376 = CARTESIAN_POINT ( 'NONE',  ( 28.41236345070440805, -1.224654026667450157, -6.045523132457580218 ) ) ;
#32377 = CARTESIAN_POINT ( 'NONE',  ( -1.699609906766908596, -29.56993018339339940, 7.767301406074262893 ) ) ;
#32378 = CARTESIAN_POINT ( 'NONE',  ( 3.540944505460754232, -26.71118433530377345, 6.876076431790004939 ) ) ;
#32379 = AXIS2_PLACEMENT_3D ( 'NONE', #36034, #8004, #39499 ) ;
#32380 = ADVANCED_FACE ( 'NONE', ( #35966 ), #19905, .F. ) ;
#32381 = ADVANCED_FACE ( 'NONE', ( #1200 ), #38832, .F. ) ;
#32382 = CARTESIAN_POINT ( 'NONE',  ( 4.733332635154806844, -31.31396321282658235, 7.762796336881264025 ) ) ;
#32383 = ORIENTED_EDGE ( 'NONE', *, *, #3800, .T. ) ;
#32384 = CARTESIAN_POINT ( 'NONE',  ( 0.7375069407144074773, -26.30912409433673105, 6.949473656533218247 ) ) ;
#32385 = DIRECTION ( 'NONE',  ( 0.3757233601570965087, 0.9267318687906770380, 0.000000000000000000 ) ) ;
#32386 = EDGE_CURVE ( 'NONE', #12201, #18006, #29770, .T. ) ;
#32387 = CARTESIAN_POINT ( 'NONE',  ( 32.98356798830028680, -0.3891095675782572649, -5.239434360015620129 ) ) ;
#32388 = CARTESIAN_POINT ( 'NONE',  ( 1.813491020413509069, -25.25237680967872578, 6.894806418505347700 ) ) ;
#32389 = DIRECTION ( 'NONE',  ( 0.000000000000000000, 1.000000000000000000, -0.000000000000000000 ) ) ;
#32390 = CARTESIAN_POINT ( 'NONE',  ( 3.299688604277355886, -32.57030420550657368, 7.761597726988850532 ) ) ;
#32391 = CARTESIAN_POINT ( 'NONE',  ( -63.54340798299629256, 43.49363706015520137, -3.059022540971626736 ) ) ;
#32392 = DIRECTION ( 'NONE',  ( -1.000000000000000000, 0.000000000000000000, -0.000000000000000000 ) ) ;
#32393 = CARTESIAN_POINT ( 'NONE',  ( -0.4574971862840269687, -32.19738569945798901, 7.691066658568940895 ) ) ;
#32394 = DIRECTION ( 'NONE',  ( -0.9396926207859104263, 0.3420201433256631063, -0.000000000000000000 ) ) ;
#32395 = ORIENTED_EDGE ( 'NONE', *, *, #31958, .F. ) ;
#32396 = CARTESIAN_POINT ( 'NONE',  ( 29.26500471863120367, 0.8173314802168033522, 4.740106445390345868 ) ) ;
#32397 = CARTESIAN_POINT ( 'NONE',  ( -2.340808619595282636, -26.33796619817592699, 7.754798119455333705 ) ) ;
#32398 = CARTESIAN_POINT ( 'NONE',  ( 67.35228065126028696, 58.41716755899589941, -3.985038673850037849 ) ) ;
#32399 = CARTESIAN_POINT ( 'NONE',  ( 3.056873540704305725, -26.34348374009132243, 7.011627023500182965 ) ) ;
#32400 = ORIENTED_EDGE ( 'NONE', *, *, #10235, .T. ) ;
#32401 = DIRECTION ( 'NONE',  ( 1.000000000000000000, 0.000000000000000000, 0.000000000000000000 ) ) ;
#32402 = DIRECTION ( 'NONE',  ( -0.7660444431189800119, -0.6427876096865369204, 0.000000000000000000 ) ) ;
#32403 = CARTESIAN_POINT ( 'NONE',  ( 22.57817341642408238, 3.872950795758598463, 3.791059833831656345 ) ) ;
#32404 = CARTESIAN_POINT ( 'NONE',  ( 0.4707025585334126960, -26.29306066231216477, 7.678495282201402539 ) ) ;
#32405 = CARTESIAN_POINT ( 'NONE',  ( 3.614139375300875923, -26.63947566482720219, 6.951256099901591767 ) ) ;
#32406 = CARTESIAN_POINT ( 'NONE',  ( -1.744308430292528911, -30.22698574235089808, 7.255881584735163869 ) ) ;
#32407 = VERTEX_POINT ( 'NONE', #6685 ) ;
#32408 =( NAMED_UNIT ( * ) PLANE_ANGLE_UNIT ( ) SI_UNIT ( $, .RADIAN. ) );
#32409 = CARTESIAN_POINT ( 'NONE',  ( 81.14373266700285114, 62.24431303712577090, 2.911438267503737354 ) ) ;
#32410 = DIRECTION ( 'NONE',  ( -0.000000000000000000, -0.000000000000000000, 1.000000000000000000 ) ) ;
#32411 = VERTEX_POINT ( 'NONE', #19035 ) ;
#32412 = CARTESIAN_POINT ( 'NONE',  ( 78.56694041390316841, 64.50177951359142980, -3.424416364708429583 ) ) ;
#32414 = CARTESIAN_POINT ( 'NONE',  ( -1.715256444303578709, -28.80609991944411163, 6.884455691889194817 ) ) ;
#32413 = CARTESIAN_POINT ( 'NONE',  ( 24.74432928415070521, 0.5874317898091796497, 4.777574746359165125 ) ) ;
#32415 = CARTESIAN_POINT ( 'NONE',  ( 80.90131254180703024, 64.57540998626842565, -3.341858160548295764 ) ) ;
#32416 = CARTESIAN_POINT ( 'NONE',  ( 79.84787171156668251, 62.37423782317881660, 3.536670452273173559 ) ) ;
#32417 = CARTESIAN_POINT ( 'NONE',  ( 82.23130663822968245, 64.88126268290433529, 1.480606629405690544 ) ) ;
#32418 = CARTESIAN_POINT ( 'NONE',  ( -64.08758708074093136, 43.59044912937621774, 1.299988725260725841 ) ) ;
#32419 = CARTESIAN_POINT ( 'NONE',  ( 24.68629359590044459, -1.668547755296895696, 6.687296101055469677 ) ) ;
#32420 = CARTESIAN_POINT ( 'NONE',  ( -64.17177837788925387, 36.63861034030102815, -5.251833000746768398 ) ) ;
#32421 = VERTEX_POINT ( 'NONE', #22542 ) ;
#32422 = VECTOR ( 'NONE', #22192, 1000.000000000000000 ) ;
#32423 = CARTESIAN_POINT ( 'NONE',  ( -80.18991991861095414, -5.669444215152338096, 3.791920745091341249 ) ) ;
#32424 = DIRECTION ( 'NONE',  ( -0.000000000000000000, -0.000000000000000000, 1.000000000000000000 ) ) ;
#32425 = CARTESIAN_POINT ( 'NONE',  ( -70.92837670882107659, 13.87661300689599386, 0.000000000000000000 ) ) ;
#32426 = DIRECTION ( 'NONE',  ( -0.000000000000000000, -0.000000000000000000, 1.000000000000000000 ) ) ;
#32427 = EDGE_CURVE ( 'NONE', #3771, #16635, #16655, .T. ) ;
#32428 = CARTESIAN_POINT ( 'NONE',  ( 30.88365314066634326, 0.6996741485792697945, -4.491056140736914060 ) ) ;
#32429 =( NAMED_UNIT ( * ) SI_UNIT ( $, .STERADIAN. ) SOLID_ANGLE_UNIT ( ) );
#32430 = PLANE ( 'NONE',  #13038 ) ;
#32431 = CARTESIAN_POINT ( 'NONE',  ( -1.094195156875065189, -31.67713398147757431, 6.912143950357348743 ) ) ;
#32432 = CARTESIAN_POINT ( 'NONE',  ( 5.195729446393100304, -29.75058702122511889, 6.998987538705429223 ) ) ;
#32433 = CARTESIAN_POINT ( 'NONE',  ( -0.8980191362577285563, -27.22509128144364610, 7.750000000000000888 ) ) ;
#32434 = CARTESIAN_POINT ( 'NONE',  ( 2.538853852545528866, -32.87225273861094621, 7.505001789837629111 ) ) ;
#32435 = CIRCLE ( 'NONE', #5468, 10.00000000000000888 ) ;
#32436 = FACE_OUTER_BOUND ( 'NONE', #424, .T. ) ;
#32437 = LINE ( 'NONE', #339, #3261 ) ;
#32438 = VERTEX_POINT ( 'NONE', #6270 ) ;
#32439 = ORIENTED_EDGE ( 'NONE', *, *, #26643, .T. ) ;
#32440 = CARTESIAN_POINT ( 'NONE',  ( 66.82989622468531365, 58.03237508814455481, 3.998112125426342978 ) ) ;
#32441 = CARTESIAN_POINT ( 'NONE',  ( -63.06903391669437298, 38.60168910470056147, 3.999999999999999112 ) ) ;
#32442 = AXIS2_PLACEMENT_3D ( 'NONE', #40250, #28315, #24614 ) ;
#32443 = CARTESIAN_POINT ( 'NONE',  ( 84.96089493372460311, 1.928984934743871449, -4.835719925821683418 ) ) ;
#32444 = CARTESIAN_POINT ( 'NONE',  ( 1.300000000000000044, 0.000000000000000000, -4.075022672948151126 ) ) ;
#32445 = ORIENTED_EDGE ( 'NONE', *, *, #17912, .T. ) ;
#32446 = CARTESIAN_POINT ( 'NONE',  ( -73.39348799458949202, 5.379232413676362512, -10.89378155313290897 ) ) ;
#32447 = ADVANCED_FACE ( 'NONE', ( #15736 ), #19233, .F. ) ;
#32448 = DIRECTION ( 'NONE',  ( -0.000000000000000000, -0.000000000000000000, -1.000000000000000000 ) ) ;
#32449 = CARTESIAN_POINT ( 'NONE',  ( 1.145807735209343869, -26.12896870525112192, 7.785344483711591934 ) ) ;
#32450 = VERTEX_POINT ( 'NONE', #28288 ) ;
#32451 = ORIENTED_EDGE ( 'NONE', *, *, #34523, .T. ) ;
#32452 = VERTEX_POINT ( 'NONE', #34911 ) ;
#32453 = CARTESIAN_POINT ( 'NONE',  ( 78.90889979212947480, 65.37513451817237353, -2.884918531047277135 ) ) ;
#32454 = CARTESIAN_POINT ( 'NONE',  ( -22.24874870218063450, -25.49307895267003587, 6.700000000000000178 ) ) ;
#32455 = CARTESIAN_POINT ( 'NONE',  ( 80.62613562354553665, 62.33752749645049818, 3.268578535636590399 ) ) ;
#32457 = ORIENTED_EDGE ( 'NONE', *, *, #37374, .T. ) ;
#32456 = CARTESIAN_POINT ( 'NONE',  ( 2.926619159346142141, -26.29176571567377607, 6.894806418505347700 ) ) ;
#32458 = EDGE_CURVE ( 'NONE', #23165, #30342, #21953, .T. ) ;
#32459 = DIRECTION ( 'NONE',  ( 0.000000000000000000, 0.000000000000000000, -1.000000000000000000 ) ) ;
#32460 = SHAPE_REPRESENTATION ( 'Fixed Die', ( #30744 ), #27429 ) ;
#32461 = CARTESIAN_POINT ( 'NONE',  ( 0.9044129672056784308, -32.97821799810775190, 6.965379264086542399 ) ) ;
#32462 = CARTESIAN_POINT ( 'NONE',  ( 3.388683086819756163, -26.61871572696936994, 7.635761828346577573 ) ) ;
#32463 = CARTESIAN_POINT ( 'NONE',  ( 33.87028684928710476, -5.289643708110279618, -1.965944456772101390 ) ) ;
#32464 = CARTESIAN_POINT ( 'NONE',  ( 3.402870446324275822, -26.62687723664940620, 7.769368695748491760 ) ) ;
#32465 = CARTESIAN_POINT ( 'NONE',  ( 76.98021629873809957, 64.85258827439523088, -2.378915702215372185 ) ) ;
#32466 = EDGE_LOOP ( 'NONE', ( #8764, #5281, #6490, #37850 ) ) ;
#32467 = CARTESIAN_POINT ( 'NONE',  ( -1.768673557917413319, -30.03425483734397972, 6.875780273367531059 ) ) ;
#32468 = DIRECTION ( 'NONE',  ( 0.4582725098355734938, -0.8888117386314180468, -0.000000000000000000 ) ) ;
#32469 = VECTOR ( 'NONE', #21857, 1000.000000000000000 ) ;
#32470 = CARTESIAN_POINT ( 'NONE',  ( -74.88476387340585916, -2.943434482340918645, -9.227807331241843158 ) ) ;
#32471 = ADVANCED_FACE ( 'NONE', ( #3420 ), #38155, .T. ) ;
#32472 = FACE_OUTER_BOUND ( 'NONE', #22483, .T. ) ;
#32473 = CARTESIAN_POINT ( 'NONE',  ( -12.97867591359219297, -24.55319635012989110, 6.800000000000000711 ) ) ;
#32474 = CARTESIAN_POINT ( 'NONE',  ( 79.08570711028919220, 65.99300539798554155, 2.058202901128779239 ) ) ;
#32475 = DIRECTION ( 'NONE',  ( 0.000000000000000000, 0.000000000000000000, 1.000000000000000000 ) ) ;
#32476 = PLANE ( 'NONE',  #4911 ) ;
#32477 = CARTESIAN_POINT ( 'NONE',  ( -0.8809241381359119716, -31.78280542688255395, 7.692469944509201518 ) ) ;
#32478 = CARTESIAN_POINT ( 'NONE',  ( -40.34874870218063592, -26.64985754041175525, 6.700000000000000178 ) ) ;
#32479 = VECTOR ( 'NONE', #21563, 1000.000000000000000 ) ;
#32480 = DIRECTION ( 'NONE',  ( -1.000000000000000000, 0.000000000000000000, 0.000000000000000000 ) ) ;
#32481 = CARTESIAN_POINT ( 'NONE',  ( 1.300000000000000044, 0.5999999999999995337, -4.250000000000000000 ) ) ;
#32482 = CARTESIAN_POINT ( 'NONE',  ( 4.899153066642030652, -28.41754821824075705, 7.775108481317161591 ) ) ;
#32483 = CARTESIAN_POINT ( 'NONE',  ( 4.921324086407802056, -24.55319635012989110, 6.700000000000000178 ) ) ;
#32484 = ORIENTED_EDGE ( 'NONE', *, *, #23654, .T. ) ;
#32485 = CARTESIAN_POINT ( 'NONE',  ( 35.86950732074304682, -2.085441397799345786, 5.804702143351438970 ) ) ;
#32486 = EDGE_CURVE ( 'NONE', #2342, #13356, #25852, .T. ) ;
#32487 = CARTESIAN_POINT ( 'NONE',  ( -64.08758708074093136, 42.21690229009149675, -2.785273621577612158 ) ) ;
#32488 = CARTESIAN_POINT ( 'NONE',  ( 87.34032947353671261, 0.2529211099193515166, 5.122688537971352929 ) ) ;
#32490 = CARTESIAN_POINT ( 'NONE',  ( -0.5254690805390769270, -26.86890242742082080, 6.894806418505347700 ) ) ;
#32489 = CARTESIAN_POINT ( 'NONE',  ( 80.06561887301042191, 64.50783488872740179, -3.572022490087452873 ) ) ;
#32491 = CARTESIAN_POINT ( 'NONE',  ( -70.73005440458344140, -48.61702805680356931, 10.00000000000000533 ) ) ;
#32492 = CARTESIAN_POINT ( 'NONE',  ( -1.311566454172203189, -27.78718944202504915, 6.887161170156906209 ) ) ;
#32493 = CARTESIAN_POINT ( 'NONE',  ( -58.66072975137505807, 29.93711237438063222, 5.396324374907178978 ) ) ;
#32494 = ORIENTED_EDGE ( 'NONE', *, *, #1832, .F. ) ;
#32495 = CARTESIAN_POINT ( 'NONE',  ( 4.906207855869877399, -30.70250798326520680, 7.721096864323906850 ) ) ;
#32496 = ORIENTED_EDGE ( 'NONE', *, *, #1371, .T. ) ;
#32497 = CARTESIAN_POINT ( 'NONE',  ( -75.45330471031414277, 33.71485196875532608, -46.17089178453873188 ) ) ;
#32498 = AXIS2_PLACEMENT_3D ( 'NONE', #26218, #38748, #20017 ) ;
#32499 = VECTOR ( 'NONE', #37045, 1000.000000000000000 ) ;
#32501 = ORIENTED_EDGE ( 'NONE', *, *, #33763, .F. ) ;
#32500 = VERTEX_POINT ( 'NONE', #35306 ) ;
#32502 = CARTESIAN_POINT ( 'NONE',  ( 80.44862750795371653, 63.21300062201452619, -3.624000857162081424 ) ) ;
#32503 = EDGE_CURVE ( 'NONE', #18803, #35245, #23199, .T. ) ;
#32504 = LINE ( 'NONE', #13759, #24667 ) ;
#32505 = EDGE_CURVE ( 'NONE', #24741, #20380, #27395, .T. ) ;
#32506 = CARTESIAN_POINT ( 'NONE',  ( 81.09516781258611218, 61.58556622376321599, 2.215902410107942977 ) ) ;
#32507 = CARTESIAN_POINT ( 'NONE',  ( 22.77511887918089784, 1.984009684073128943, 5.106421591786454606 ) ) ;
#32508 = ORIENTED_EDGE ( 'NONE', *, *, #16507, .F. ) ;
#32509 = EDGE_CURVE ( 'NONE', #12694, #8980, #31150, .T. ) ;
#32510 = AXIS2_PLACEMENT_3D ( 'NONE', #4821, #29929, #1746 ) ;
#32511 = CARTESIAN_POINT ( 'NONE',  ( -32.44874870218063734, -25.49307895267003587, 6.800000000000000711 ) ) ;
#32513 = CARTESIAN_POINT ( 'NONE',  ( 6.041439283768642809, -29.54977971180056784, 7.013842709614101167 ) ) ;
#32512 = CARTESIAN_POINT ( 'NONE',  ( 14.77315594796849574, 13.19392823276453441, -2.500000000000005773 ) ) ;
#32514 = CARTESIAN_POINT ( 'NONE',  ( 4.392721987511531978, -31.80629977964779442, 7.749999999999998224 ) ) ;
#32515 = CARTESIAN_POINT ( 'NONE',  ( -64.08758708074093136, 42.98405160848505346, -2.320550955811203853 ) ) ;
#32516 = CARTESIAN_POINT ( 'NONE',  ( 71.99851445618389789, 60.18445664521269123, 3.955776929956314358 ) ) ;
#32517 = VERTEX_POINT ( 'NONE', #28496 ) ;
#32518 = CARTESIAN_POINT ( 'NONE',  ( 22.55565315994001097, 4.076294750019800794, -3.649699173882503977 ) ) ;
#32519 = ORIENTED_EDGE ( 'NONE', *, *, #19424, .T. ) ;
#32520 = CARTESIAN_POINT ( 'NONE',  ( 1.700390093233090871, -29.56993018339339940, 7.750000000000000888 ) ) ;
#32521 = ORIENTED_EDGE ( 'NONE', *, *, #33251, .F. ) ;
#32522 = CARTESIAN_POINT ( 'NONE',  ( 21.85643539959775339, -5.954433958055524556, -11.26730592371362505 ) ) ;
#32523 = CARTESIAN_POINT ( 'NONE',  ( 21.80882946371355047, 5.293150380064015614, -3.367598806138242917 ) ) ;
#32524 = CARTESIAN_POINT ( 'NONE',  ( 1.115020328647592152, -33.02063188575903752, 7.742274884880761654 ) ) ;
#32525 = CARTESIAN_POINT ( 'NONE',  ( 81.75671479976297462, 62.52433184976159453, 2.563845612517931194 ) ) ;
#32526 = CARTESIAN_POINT ( 'NONE',  ( 88.25293897076788596, -0.9571425830051931705, -4.167473131139645126 ) ) ;
#32527 = CARTESIAN_POINT ( 'NONE',  ( -1.784512137809761700, -29.51577928193536593, 7.785387725071483800 ) ) ;
#32528 = ORIENTED_EDGE ( 'NONE', *, *, #34855, .F. ) ;
#32529 = CARTESIAN_POINT ( 'NONE',  ( -80.25993260945720920, -5.625204836179395151, 5.971172885161660560 ) ) ;
#32530 = VERTEX_POINT ( 'NONE', #19641 ) ;
#32531 = CARTESIAN_POINT ( 'NONE',  ( 15.04281356191366292, -4.011470685753230292, 2.554192886794166117 ) ) ;
#32532 = VECTOR ( 'NONE', #22106, 1000.000000000000000 ) ;
#32533 = VECTOR ( 'NONE', #35116, 1000.000000000000000 ) ;
#32534 = CARTESIAN_POINT ( 'NONE',  ( 5.077579250296520463, -29.17672728242957803, 6.997764925645182821 ) ) ;
#32535 = CARTESIAN_POINT ( 'NONE',  ( -63.08758708074093136, 38.76906266698303227, 4.000000000000000000 ) ) ;
#32536 = CARTESIAN_POINT ( 'NONE',  ( 31.71772644211463188, -0.5622319885707789400, -5.156716326041481224 ) ) ;
#32537 = CARTESIAN_POINT ( 'NONE',  ( 0.5564878831059402176, -32.77173156853538671, 7.643333865083955736 ) ) ;
#32538 = CARTESIAN_POINT ( 'NONE',  ( 84.47597663471815110, 2.555392163460764809, -3.359472611266297815 ) ) ;
#32539 = CARTESIAN_POINT ( 'NONE',  ( -0.5115343435586707788, -26.98779995897780637, 7.712764235869101981 ) ) ;
#32540 = AXIS2_PLACEMENT_3D ( 'NONE', #17056, #4533, #25948 ) ;
#32541 = CARTESIAN_POINT ( 'NONE',  ( -1.642218429049665529, -30.19199791826050117, 7.721096864323902409 ) ) ;
#32542 = CARTESIAN_POINT ( 'NONE',  ( 4.989036686621270533, -28.41059008988207424, 7.783750581861599294 ) ) ;
#32543 = ORIENTED_EDGE ( 'NONE', *, *, #20044, .T. ) ;
#32544 = ORIENTED_EDGE ( 'NONE', *, *, #19112, .T. ) ;
#32545 = CARTESIAN_POINT ( 'NONE',  ( 37.00854049623069386, -3.246023182758657200, 5.947063170885879657 ) ) ;
#32546 = CARTESIAN_POINT ( 'NONE',  ( -1.643142028458829396, -30.60472337334698878, 7.011627023500186517 ) ) ;
#32547 = CARTESIAN_POINT ( 'NONE',  ( 66.27376694609004915, 57.73522568913436004, -4.000000000000000000 ) ) ;
#32548 = ADVANCED_FACE ( 'NONE', ( #6482 ), #16333, .T. ) ;
#32549 = CARTESIAN_POINT ( 'NONE',  ( 87.92225447513270353, -2.506640933623296430, 0.2833183356762295491 ) ) ;
#32550 = ORIENTED_EDGE ( 'NONE', *, *, #21847, .F. ) ;
#32551 = EDGE_CURVE ( 'NONE', #6774, #16841, #19297, .T. ) ;
#32552 = CARTESIAN_POINT ( 'NONE',  ( 5.141357650781797517, -28.92980723922511288, 7.720710062488889136 ) ) ;
#32553 =( LENGTH_UNIT ( ) NAMED_UNIT ( * ) SI_UNIT ( .MILLI., .METRE. ) );
#32554 = ORIENTED_EDGE ( 'NONE', *, *, #39961, .F. ) ;
#32555 = CARTESIAN_POINT ( 'NONE',  ( -56.50908310466265050, 29.95896301100017567, -1.719924897558571697 ) ) ;
#32556 =( LENGTH_UNIT ( ) NAMED_UNIT ( * ) SI_UNIT ( .MILLI., .METRE. ) );
#32557 = ORIENTED_EDGE ( 'NONE', *, *, #34344, .F. ) ;
#32558 = CARTESIAN_POINT ( 'NONE',  ( 22.14223375496702317, 4.765437392088810675, 3.533749582433190817 ) ) ;
#32559 = EDGE_CURVE ( 'NONE', #4035, #23856, #1036, .T. ) ;
#32560 = CARTESIAN_POINT ( 'NONE',  ( 82.43454424851934448, 64.20405324974024097, -1.755995906648851079 ) ) ;
#32561 = VECTOR ( 'NONE', #690, 1000.000000000000114 ) ;
#32562 = VECTOR ( 'NONE', #23786, 1000.000000000000000 ) ;
#32563 = EDGE_CURVE ( 'NONE', #30107, #26569, #34706, .T. ) ;
#32564 = CARTESIAN_POINT ( 'NONE',  ( 3.855327937537480487, -32.32757912347058493, 7.754798119455333705 ) ) ;
#32565 = EDGE_LOOP ( 'NONE', ( #28130, #17670, #9278, #19175 ) ) ;
#32566 = CARTESIAN_POINT ( 'NONE',  ( 76.30453859000765249, 59.72919098693703432, -3.074209570828594362 ) ) ;
#32567 = VECTOR ( 'NONE', #35877, 1000.000000000000000 ) ;
#32569 = DIRECTION ( 'NONE',  ( -0.000000000000000000, -1.000000000000000000, -0.000000000000000000 ) ) ;
#32568 = CARTESIAN_POINT ( 'NONE',  ( 2.488040083129651414, -26.15970915046665723, 6.916197352289366052 ) ) ;
#32570 = CYLINDRICAL_SURFACE ( 'NONE', #32981, 0.09010775117052928496 ) ;
#32571 = CARTESIAN_POINT ( 'NONE',  ( 75.82377327987001081, 62.28299708301691595, 3.825872951952284051 ) ) ;
#32572 = ORIENTED_EDGE ( 'NONE', *, *, #39130, .T. ) ;
#32573 = CARTESIAN_POINT ( 'NONE',  ( -64.08758708074093136, 37.27332153486386090, 4.546479763849019307 ) ) ;
#32574 = VECTOR ( 'NONE', #26768, 1000.000000000000114 ) ;
#32575 = DIRECTION ( 'NONE',  ( 0.8660254037844450359, -0.4999999999999888978, -0.000000000000000000 ) ) ;
#32576 = CARTESIAN_POINT ( 'NONE',  ( -16.97867591359219475, -24.55319635012989110, 6.700000000000000178 ) ) ;
#32577 = LINE ( 'NONE', #32972, #6377 ) ;
#32578 = CARTESIAN_POINT ( 'NONE',  ( 81.80771926544794326, 61.88353390887446182, 1.601045042264324092 ) ) ;
#32579 = CARTESIAN_POINT ( 'NONE',  ( 4.077682286559045188, -32.01059352804590219, 7.505001789837624671 ) ) ;
#32580 = CARTESIAN_POINT ( 'NONE',  ( 32.04447592720433136, -5.114560573210904515, 0.4782324236124577688 ) ) ;
#32581 = CARTESIAN_POINT ( 'NONE',  ( 4.746899557684813864, -27.84691535960167030, 6.894806418505347700 ) ) ;
#32582 = CARTESIAN_POINT ( 'NONE',  ( -70.12927831234416942, -21.39817538196428615, 9.968450010350149881 ) ) ;
#32583 = CARTESIAN_POINT ( 'NONE',  ( 4.670958646267747483, -31.41922106168711082, 7.761113333116791857 ) ) ;
#32584 = CARTESIAN_POINT ( 'NONE',  ( 0.7369679840504070878, -26.30928333966162569, 6.959317978105165281 ) ) ;
#32585 = CARTESIAN_POINT ( 'NONE',  ( 75.39030949273650606, 59.47930393830225171, 3.241331962143158663 ) ) ;
#32586 = CARTESIAN_POINT ( 'NONE',  ( 29.26503589862772969, 0.8173198370404799462, -4.740111391064184332 ) ) ;
#32587 = CARTESIAN_POINT ( 'NONE',  ( 1.021790419572949915, -32.90152176744273049, 7.778050822775632867 ) ) ;
#32588 = CARTESIAN_POINT ( 'NONE',  ( 4.703510412144804143, -31.36750308876875337, 6.875671892026064214 ) ) ;
#32589 = CARTESIAN_POINT ( 'NONE',  ( 5.153279172109078488, -30.14225614731512337, 7.695279973900954751 ) ) ;
#32590 = CARTESIAN_POINT ( 'NONE',  ( -1.556861139293656660, -28.32973185486151735, 7.785344483711591934 ) ) ;
#32591 = B_SPLINE_CURVE_WITH_KNOTS ( 'NONE', 3,
 ( #22422, #31892, #37626, #34589, #9641, #31076, #6767, #28798, #6364, #9023, #15826, #24827, #601, #2884 ),
 .UNSPECIFIED., .F., .F.,
 ( 4, 2, 2, 2, 2, 2, 4 ),
 ( 0.000000000000000000, 2.311601343512421228E-05, 4.623202687024842455E-05, 9.246405374049915303E-05, 0.0001849281074810030223, 0.0003698562149620148267, 0.0007397124299240395197 ),
 .UNSPECIFIED. ) ;
#32592 = EDGE_CURVE ( 'NONE', #31945, #25222, #16935, .T. ) ;
#32593 = DIRECTION ( 'NONE',  ( 1.000000000000000000, 0.000000000000000000, 0.000000000000000000 ) ) ;
#32594 = VECTOR ( 'NONE', #19081, 1000.000000000000000 ) ;
#32595 = ORIENTED_EDGE ( 'NONE', *, *, #916, .T. ) ;
#32596 = CARTESIAN_POINT ( 'NONE',  ( 29.34598460277089060, 0.9961803144104202090, 4.626948874399350764 ) ) ;
#32597 =( BOUNDED_CURVE ( )  B_SPLINE_CURVE ( 3, ( #11850, #33514, #11641, #14132 ),
 .UNSPECIFIED., .F., .T. ) 
 B_SPLINE_CURVE_WITH_KNOTS ( ( 4, 4 ),
 ( 4.708531083176467291, 4.895802057644188743 ),
 .UNSPECIFIED. ) 
 CURVE ( )  GEOMETRIC_REPRESENTATION_ITEM ( )  RATIONAL_B_SPLINE_CURVE ( ( 1.000000000000000000, 0.9970795998553221295, 0.9970795998553221295, 1.000000000000000000 ) ) 
 REPRESENTATION_ITEM ( '' )  );
#32598 = CARTESIAN_POINT ( 'NONE',  ( -70.29787437547823004, 0.001187990818876110462, 3.967530720604707462 ) ) ;
#32599 = CARTESIAN_POINT ( 'NONE',  ( 67.21358634547439692, 57.88870193986200974, -3.993497817183393472 ) ) ;
#32600 = CARTESIAN_POINT ( 'NONE',  ( -59.01947560891952804, 27.90920910948504385, 6.147301388271928957 ) ) ;
#32601 = ORIENTED_EDGE ( 'NONE', *, *, #40, .F. ) ;
#32602 = CARTESIAN_POINT ( 'NONE',  ( 4.978554560952730412, -30.79615924950642025, 6.894806418505347700 ) ) ;
#32603 = CARTESIAN_POINT ( 'NONE',  ( 30.74057244063293481, -3.574220798478507710, 4.805827853833087637 ) ) ;
#32604 = CARTESIAN_POINT ( 'NONE',  ( 85.45652069754405034, 1.208412679805325407, -5.653737850026661071 ) ) ;
#32605 = CARTESIAN_POINT ( 'NONE',  ( 2.325611040346713398, -32.91195037927720790, 7.680992449362118002 ) ) ;
#32606 = CARTESIAN_POINT ( 'NONE',  ( 3.610820004061922717, -26.63731061109791654, 6.980586498568969844 ) ) ;
#32608 = EDGE_CURVE ( 'NONE', #4319, #31687, #10343, .T. ) ;
#32607 = CARTESIAN_POINT ( 'NONE',  ( -56.10469124525552331, 30.75883671979821443, 2.489329600088167727 ) ) ;
#32609 = ORIENTED_EDGE ( 'NONE', *, *, #29943, .T. ) ;
#32610 = CARTESIAN_POINT ( 'NONE',  ( 24.74156297819196482, 3.012697116509819306, 3.382074263075999010 ) ) ;
#32611 = ADVANCED_FACE ( 'NONE', ( #7878 ), #26231, .T. ) ;
#32612 = CARTESIAN_POINT ( 'NONE',  ( -42.83131703149249603, -27.06993018339339585, 6.800000000000000711 ) ) ;
#32613 = CARTESIAN_POINT ( 'NONE',  ( 79.61290006553409171, 65.30841326124827617, 3.134554000843265520 ) ) ;
#32614 = EDGE_CURVE ( 'NONE', #27830, #2431, #6924, .T. ) ;
#32615 = CARTESIAN_POINT ( 'NONE',  ( -0.02141235007780225783, -32.61712501572831968, 7.670465701733753860 ) ) ;
#32616 = ORIENTED_EDGE ( 'NONE', *, *, #28742, .F. ) ;
#32617 = CARTESIAN_POINT ( 'NONE',  ( 79.08256350411643609, 63.89089281391859032, -3.718817779187653549 ) ) ;
#32619 = CARTESIAN_POINT ( 'NONE',  ( -1.711148526671566250, -28.78798112472082238, 7.003794266797748413 ) ) ;
#32618 = CARTESIAN_POINT ( 'NONE',  ( 21.78676948381099976, 0.2189784557031426993, 8.380332209910813290 ) ) ;
#32620 = CARTESIAN_POINT ( 'NONE',  ( 81.38764266124616142, 63.30759111148670826, -3.202775791559302476 ) ) ;
#32621 = CARTESIAN_POINT ( 'NONE',  ( 80.72640005664072760, 61.14345848406946260, 1.640065189519674282 ) ) ;
#32622 = ORIENTED_EDGE ( 'NONE', *, *, #20871, .F. ) ;
#32623 = AXIS2_PLACEMENT_3D ( 'NONE', #23794, #11429, #7753 ) ;
#32624 = DIRECTION ( 'NONE',  ( 0.000000000000000000, 1.000000000000000000, 0.000000000000000000 ) ) ;
#32625 = AXIS2_PLACEMENT_3D ( 'NONE', #31081, #6161, #9030 ) ;
#32626 = CARTESIAN_POINT ( 'NONE',  ( 81.34501148009313454, 65.92776879248955879, 1.287552078897677976 ) ) ;
#32628 = ORIENTED_EDGE ( 'NONE', *, *, #35988, .T. ) ;
#32627 = FACE_OUTER_BOUND ( 'NONE', #34944, .T. ) ;
#32629 = CARTESIAN_POINT ( 'NONE',  ( 24.43802896994273510, -0.4903351684736660387, 6.966919456710074954 ) ) ;
#32630 = ORIENTED_EDGE ( 'NONE', *, *, #28665, .F. ) ;
#32631 = CARTESIAN_POINT ( 'NONE',  ( -74.78555365388220366, -2.834168353914430671, 10.55874562434718378 ) ) ;
#32632 = CARTESIAN_POINT ( 'NONE',  ( 26.06260999411897217, 0.7785562455270252924, -4.421375452052825672 ) ) ;
#32633 = AXIS2_PLACEMENT_3D ( 'NONE', #6449, #15903, #28051 ) ;
#32634 = CARTESIAN_POINT ( 'NONE',  ( 0.9904113513190105911, -32.89497607571279758, 7.754798119455333705 ) ) ;
#32635 = CARTESIAN_POINT ( 'NONE',  ( 4.200390093233091093, -29.56993018339339940, -15.49999999999999822 ) ) ;
#32636 = CARTESIAN_POINT ( 'NONE',  ( 33.11348551397914974, -0.1515143186654732133, -4.942515107159420218 ) ) ;
#32637 = SURFACE_SIDE_STYLE ('',( #32237 ) ) ;
#32638 = DIRECTION ( 'NONE',  ( 0.9396926207859126468, -0.3420201433256568335, -0.000000000000000000 ) ) ;
#32639 = CARTESIAN_POINT ( 'NONE',  ( 5.108657383620684556, -30.36599178733747095, 6.951256099901588215 ) ) ;
#32640 = PLANE ( 'NONE',  #24549 ) ;
#32641 = DIRECTION ( 'NONE',  ( 0.000000000000000000, 0.000000000000000000, -1.000000000000000000 ) ) ;
#32642 = CARTESIAN_POINT ( 'NONE',  ( 5.094538413962854229, -29.76940238803287286, 6.911401339314959813 ) ) ;
#32643 = CARTESIAN_POINT ( 'NONE',  ( 1.875215828509756655, -26.07429920139816559, 7.006908160621413195 ) ) ;
#32644 = ORIENTED_EDGE ( 'NONE', *, *, #26327, .T. ) ;
#32645 = EDGE_LOOP ( 'NONE', ( #8883, #17274, #31895, #965 ) ) ;
#32646 = CARTESIAN_POINT ( 'NONE',  ( 66.67928806435183731, 57.99078996168128697, 3.997717836774547617 ) ) ;
#32647 = CARTESIAN_POINT ( 'NONE',  ( 73.54169881536046205, 59.75047131450637750, -3.824679913398719044 ) ) ;
#32648 = CARTESIAN_POINT ( 'NONE',  ( 86.89103086197154369, -0.8412156502217053022, -5.497997349500185926 ) ) ;
#32649 = CARTESIAN_POINT ( 'NONE',  ( -1.506684114051581647, -28.44091511309124343, 7.695279973900954751 ) ) ;
#32650 = CIRCLE ( 'NONE', #18823, 5.000000000000000000 ) ;
#32651 = CARTESIAN_POINT ( 'NONE',  ( -77.50089735354119114, 9.756467026281873345, -9.131598822715689678 ) ) ;
#32652 = CARTESIAN_POINT ( 'NONE',  ( -75.45330471031414277, 33.71485196875497792, 18.79999999999999716 ) ) ;
#32653 = AXIS2_PLACEMENT_3D ( 'NONE', #24716, #22405, #37264 ) ;
#32654 = CARTESIAN_POINT ( 'NONE',  ( 2.933187319672341253, -26.30959554060986605, 7.785096263473211486 ) ) ;
#32655 = DIRECTION ( 'NONE',  ( 0.000000000000000000, 0.000000000000000000, 1.000000000000000000 ) ) ;
#32656 = ORIENTED_EDGE ( 'NONE', *, *, #5391, .T. ) ;
#32657 = ADVANCED_FACE ( 'NONE', ( #7275 ), #1932, .F. ) ;
#32658 = CARTESIAN_POINT ( 'NONE',  ( -51.21549048184567710, -30.94667987854474234, 6.000000000000000000 ) ) ;
#32659 = EDGE_CURVE ( 'NONE', #3202, #3667, #1928, .T. ) ;
#32660 = VERTEX_POINT ( 'NONE', #27021 ) ;
#32661 = CARTESIAN_POINT ( 'NONE',  ( 78.56188500726528900, 65.90376500477491106, -1.760837461004926663 ) ) ;
#32662 = CARTESIAN_POINT ( 'NONE',  ( 33.77937656451339166, -4.816664999545909431, 3.541921615443311744 ) ) ;
#32663 = CARTESIAN_POINT ( 'NONE',  ( 80.48490785079584953, 62.58389448792968324, 3.438247877890441728 ) ) ;
#32664 = CARTESIAN_POINT ( 'NONE',  ( 2.748053412748273860, -32.80449376584813592, 7.754798119455333705 ) ) ;
#32665 = CARTESIAN_POINT ( 'NONE',  ( 24.13226474559606416, 2.704999742398795259, 3.972821573215394864 ) ) ;
#32666 = CARTESIAN_POINT ( 'NONE',  ( 3.972262043637318385, -27.04038519645078864, 6.864276522220859711 ) ) ;
#32667 = DIRECTION ( 'NONE',  ( 1.000000000000000000, -0.000000000000000000, 0.000000000000000000 ) ) ;
#32668 = CARTESIAN_POINT ( 'NONE',  ( 33.88647134759106194, -5.391981279974441321, -1.346411692250225833 ) ) ;
#32669 = ORIENTED_EDGE ( 'NONE', *, *, #31531, .T. ) ;
#32670 = FACE_OUTER_BOUND ( 'NONE', #37055, .T. ) ;
#32671 = CARTESIAN_POINT ( 'NONE',  ( 5.046365345827218185, -28.96623356337001809, 7.635761828346577573 ) ) ;
#32672 = CARTESIAN_POINT ( 'NONE',  ( -73.77129911634021653, -3.508482060268308889, -9.588404479166415584 ) ) ;
#32673 = CARTESIAN_POINT ( 'NONE',  ( 4.713340623123058570, -27.78888299018493058, 7.697032948437506406 ) ) ;
#32674 = DIRECTION ( 'NONE',  ( -1.000000000000000000, 0.000000000000000000, 0.000000000000000000 ) ) ;
#32675 = CARTESIAN_POINT ( 'NONE',  ( 81.13213036240664167, 62.83067685251092627, 3.261148789966860306 ) ) ;
#32676 = CARTESIAN_POINT ( 'NONE',  ( -74.92283640148291113, 18.87330372387140187, -46.17089178453873188 ) ) ;
#32677 = CARTESIAN_POINT ( 'NONE',  ( 3.888061725287626391, -26.96722143474251610, 7.769368695748485543 ) ) ;
#32678 = CARTESIAN_POINT ( 'NONE',  ( -0.8911589727531790128, -31.77082041573498472, 7.643333865083956624 ) ) ;
#32679 = CARTESIAN_POINT ( 'NONE',  ( 3.922483456672745561, -26.86580350659783178, 7.697032948437509070 ) ) ;
#32680 = AXIS2_PLACEMENT_3D ( 'NONE', #14046, #16722, #23720 ) ;
#32681 = EDGE_CURVE ( 'NONE', #26319, #1142, #10752, .T. ) ;
#32682 = CIRCLE ( 'NONE', #37276, 3.499999999999999556 ) ;
#32683 = VECTOR ( 'NONE', #13132, 1000.000000000000227 ) ;
#32684 = CARTESIAN_POINT ( 'NONE',  ( 3.970022674624412051, -32.23428315255819854, 7.737115613922534330 ) ) ;
#32685 = CARTESIAN_POINT ( 'NONE',  ( 19.21360371875379514, 6.947362734548907071, -3.205145561710191160 ) ) ;
#32686 = FACE_OUTER_BOUND ( 'NONE', #19501, .T. ) ;
#32687 = DIRECTION ( 'NONE',  ( 1.000000000000000000, -8.921435019309294079E-15, 0.000000000000000000 ) ) ;
#32688 = CARTESIAN_POINT ( 'NONE',  ( 69.09457860630368486, 59.08023000801873081, 3.976370928559271878 ) ) ;
#32689 = CARTESIAN_POINT ( 'NONE',  ( 37.04408834714948995, -2.892981267788033772, 5.988023919871666934 ) ) ;
#32690 = ADVANCED_FACE ( 'NONE', ( #11351 ), #23331, .F. ) ;
#32691 = CARTESIAN_POINT ( 'NONE',  ( -64.08758708074093136, 41.34489873040477903, -2.999999999999999556 ) ) ;
#32692 = CARTESIAN_POINT ( 'NONE',  ( 84.90669483503786807, 2.936226605105188625, 1.856525974524364297 ) ) ;
#32694 = FACE_OUTER_BOUND ( 'NONE', #23667, .T. ) ;
#32693 = CARTESIAN_POINT ( 'NONE',  ( 80.57402935197538341, 63.63785766202913408, -3.625945587094183686 ) ) ;
#32695 = CARTESIAN_POINT ( 'NONE',  ( -1.242285469042155643, -27.67502635069157435, 6.895394898881668233 ) ) ;
#32696 = CARTESIAN_POINT ( 'NONE',  ( -57.31959649706901416, 29.49889766843901029, 4.251262061546403181 ) ) ;
#32697 = ORIENTED_EDGE ( 'NONE', *, *, #26380, .F. ) ;
#32698 = FACE_OUTER_BOUND ( 'NONE', #20259, .T. ) ;
#32699 = CARTESIAN_POINT ( 'NONE',  ( 21.76158951578306144, 5.855693934973000836, 3.369080518218454667 ) ) ;
#32700 = VERTEX_POINT ( 'NONE', #4602 ) ;
#32701 = CARTESIAN_POINT ( 'NONE',  ( -71.90933819610624766, -21.00662979218648374, 5.931425411825924421 ) ) ;
#32702 = AXIS2_PLACEMENT_3D ( 'NONE', #29454, #16668, #38703 ) ;
#32704 = ORIENTED_EDGE ( 'NONE', *, *, #4157, .F. ) ;
#32703 = VERTEX_POINT ( 'NONE', #29311 ) ;
#32705 = EDGE_CURVE ( 'NONE', #6115, #37067, #14689, .T. ) ;
#32706 = CARTESIAN_POINT ( 'NONE',  ( 80.76107640992933057, 62.37607017537882115, -3.233326467035619878 ) ) ;
#32707 =( BOUNDED_CURVE ( )  B_SPLINE_CURVE ( 3, ( #29046, #12776, #32351, #9695 ),
 .UNSPECIFIED., .F., .T. ) 
 B_SPLINE_CURVE_WITH_KNOTS ( ( 4, 4 ),
 ( 1.381924640371167579, 1.574767692156077148 ),
 .UNSPECIFIED. ) 
 CURVE ( )  GEOMETRIC_REPRESENTATION_ITEM ( )  RATIONAL_B_SPLINE_CURVE ( ( 1.000000000000000000, 0.9969033633783032089, 0.9969033633783032089, 1.000000000000000000 ) ) 
 REPRESENTATION_ITEM ( '' )  );
#32708 = VECTOR ( 'NONE', #37787, 1000.000000000000114 ) ;
#32709 = DIRECTION ( 'NONE',  ( 0.9728983447892854963, -0.2312332387574689563, 0.000000000000000000 ) ) ;
#32710 = CARTESIAN_POINT ( 'NONE',  ( 81.11523045952516497, 61.59071516775627231, 2.202709653501095488 ) ) ;
#32711 = CARTESIAN_POINT ( 'NONE',  ( 24.64619019099651354, 0.7543582096408616433, 4.794156199316148559 ) ) ;
#32712 = EDGE_LOOP ( 'NONE', ( #22189, #18330, #25064, #1872, #28162 ) ) ;
#32713 = VECTOR ( 'NONE', #30218, 1000.000000000000000 ) ;
#32714 = CARTESIAN_POINT ( 'NONE',  ( 5.031298139653363144, -30.25194762213318356, 6.866852738645442322 ) ) ;
#32716 = FACE_OUTER_BOUND ( 'NONE', #3705, .T. ) ;
#32715 = CARTESIAN_POINT ( 'NONE',  ( 39.57450465021913999, -13.08403409140692553, -6.000000000000000000 ) ) ;
#32717 = DIRECTION ( 'NONE',  ( 0.000000000000000000, 0.000000000000000000, -1.000000000000000000 ) ) ;
#32718 = CARTESIAN_POINT ( 'NONE',  ( -40.97867591359219119, -24.55319635012989110, 6.800000000000000711 ) ) ;
#32719 = CARTESIAN_POINT ( 'NONE',  ( 24.57161973902774221, 2.977233313421253413, -3.583713660848351523 ) ) ;
#32720 = EDGE_LOOP ( 'NONE', ( #21403, #10411, #36641 ) ) ;
#32721 = CARTESIAN_POINT ( 'NONE',  ( -71.92837670882107659, -0.7829914368874778541, 5.916079783099617906 ) ) ;
#32722 = VERTEX_POINT ( 'NONE', #15067 ) ;
#32723 = CARTESIAN_POINT ( 'NONE',  ( 22.53953452546943126, -1.608357795960198677, 9.096105908381383998 ) ) ;
#32724 = CARTESIAN_POINT ( 'NONE',  ( 21.85643539959980330, 4.658110446274656091, 2.545489860561468118E-12 ) ) ;
#32725 = CARTESIAN_POINT ( 'NONE',  ( 15.43177744199658896, 12.90197810732775885, 2.500000000000005773 ) ) ;
#32726 = CARTESIAN_POINT ( 'NONE',  ( 1.126087027002167451, -33.02249097042057713, 7.714178352335856026 ) ) ;
#32727 = CARTESIAN_POINT ( 'NONE',  ( 81.53035370524470693, 63.02147265738407356, 3.059106349699970639 ) ) ;
#32728 = CARTESIAN_POINT ( 'NONE',  ( 84.80723110164849743, 2.854080505324299466, 2.680610459220619912 ) ) ;
#32729 = CARTESIAN_POINT ( 'NONE',  ( -0.5046456199209383708, -26.98191322245490298, 7.652160403243381204 ) ) ;
#32730 = VERTEX_POINT ( 'NONE', #14854 ) ;
#32731 = CARTESIAN_POINT ( 'NONE',  ( -80.03623703158197600, -5.604753948939747765, 6.344040936181177592 ) ) ;
#32732 = DIRECTION ( 'NONE',  ( -1.000000000000000000, 0.000000000000000000, 0.000000000000000000 ) ) ;
#32733 = VECTOR ( 'NONE', #8384, 1000.000000000000000 ) ;
#32734 = CARTESIAN_POINT ( 'NONE',  ( 21.79474914018651788, 6.321282727555548320, -2.730181469529505023 ) ) ;
#32735 = CARTESIAN_POINT ( 'NONE',  ( 28.89366916224668813, -3.006935889917436988, -4.715953887435873959 ) ) ;
#32736 = CARTESIAN_POINT ( 'NONE',  ( 36.78886185490619454, -3.040240986573045756, -5.948189653081061401 ) ) ;
#32737 = DIRECTION ( 'NONE',  ( 1.000000000000000000, 0.000000000000000000, 0.000000000000000000 ) ) ;
#32738 = CARTESIAN_POINT ( 'NONE',  ( 84.49114003401015793, 2.536390008004397068, -3.421698485768037923 ) ) ;
#32739 = EDGE_CURVE ( 'NONE', #5157, #29043, #11755, .T. ) ;
#32740 = PRODUCT_DEFINITION_FORMATION_WITH_SPECIFIED_SOURCE ( 'ANY', '', #26257, .NOT_KNOWN. ) ;
#32741 = CARTESIAN_POINT ( 'NONE',  ( -0.5125101069461969194, -26.98863734761392053, 7.695279973900954751 ) ) ;
#32742 = CIRCLE ( 'NONE', #15654, 3.499999999999999556 ) ;
#32743 = VECTOR ( 'NONE', #3865, 1000.000000000000000 ) ;
#32744 = B_SPLINE_CURVE_WITH_KNOTS ( 'NONE', 3,
 ( #263, #12804, #34869, #6645, #13014, #19196, #28668, #24760, #38121, #9923, #37308, #9104, #34258, #6030, #31151, #15485, #40595, #12402 ),
 .UNSPECIFIED., .F., .F.,
 ( 4, 2, 2, 2, 2, 2, 2, 2, 4 ),
 ( 0.000000000000000000, 0.0003909910682061002027, 0.0007819821364122004053, 0.001563964272824406882, 0.002345946409236613576, 0.003127928545648820269, 0.004691892818473243632, 0.005473874954885450325, 0.006255857091297657019 ),
 .UNSPECIFIED. ) ;
#32745 = EDGE_CURVE ( 'NONE', #20794, #17373, #27044, .T. ) ;
#32746 = LINE ( 'NONE', #7607, #25065 ) ;
#32747 = CARTESIAN_POINT ( 'NONE',  ( -1.139292474411453204, -27.70010802646186576, 6.911401339314956260 ) ) ;
#32748 = EDGE_LOOP ( 'NONE', ( #11288, #16250, #19375, #2948 ) ) ;
#32749 = ORIENTED_EDGE ( 'NONE', *, *, #36748, .T. ) ;
#32750 = CARTESIAN_POINT ( 'NONE',  ( 36.68534330363475959, -1.915002933638632054, 5.803249200901428040 ) ) ;
#32751 = CARTESIAN_POINT ( 'NONE',  ( -0.5226183895603513374, -32.27330558770101021, 7.678495282201406980 ) ) ;
#32752 = CARTESIAN_POINT ( 'NONE',  ( 66.27376694609004915, 57.73522568913436004, -4.000000000000000000 ) ) ;
#32753 = CARTESIAN_POINT ( 'NONE',  ( 86.00054146471580907, 0.2529338399765344580, 5.999804812770356932 ) ) ;
#32754 = ORIENTED_EDGE ( 'NONE', *, *, #40384, .T. ) ;
#32755 = LINE ( 'NONE', #4352, #4299 ) ;
#32756 = EDGE_CURVE ( 'NONE', #37348, #40076, #1533, .T. ) ;
#32757 = AXIS2_PLACEMENT_3D ( 'NONE', #16785, #19498, #4467 ) ;
#32758 = VERTEX_POINT ( 'NONE', #8675 ) ;
#32759 = DIRECTION ( 'NONE',  ( -0.000000000000000000, -0.000000000000000000, -1.000000000000000000 ) ) ;
#32761 = CARTESIAN_POINT ( 'NONE',  ( 4.301456835768374454, -27.38029081488210181, 7.763628509615287498 ) ) ;
#32760 = CARTESIAN_POINT ( 'NONE',  ( -28.24874870218063805, -26.64985754041175525, 6.800000000000000711 ) ) ;
#32762 = EDGE_LOOP ( 'NONE', ( #16296, #5952, #39093, #35217 ) ) ;
#32763 = CARTESIAN_POINT ( 'NONE',  ( 23.88456871391472092, 3.166956515880607892, 3.639194615745996675 ) ) ;
#32764 = CARTESIAN_POINT ( 'NONE',  ( 81.91393161461809314, 61.93681595580208210, -1.358135763685572206 ) ) ;
#32765 = AXIS2_PLACEMENT_3D ( 'NONE', #18260, #11461, #27329 ) ;
#32766 = DIRECTION ( 'NONE',  ( -0.3420201433256725987, 0.9396926207859068736, -0.000000000000000000 ) ) ;
#32767 = ORIENTED_EDGE ( 'NONE', *, *, #5175, .T. ) ;
#32769 = CARTESIAN_POINT ( 'NONE',  ( -70.92837670882107659, 13.87661300689593880, 6.000000000000005329 ) ) ;
#32768 = LINE ( 'NONE', #9915, #31839 ) ;
#32770 = CARTESIAN_POINT ( 'NONE',  ( -6.348748702180634140, -26.64985754041175525, 6.700000000000000178 ) ) ;
#32771 = CARTESIAN_POINT ( 'NONE',  ( 74.91689101425367880, 62.74844471888588515, 3.527522301306301067 ) ) ;
#32772 = CARTESIAN_POINT ( 'NONE',  ( 23.83171675590329386, 2.746212528099347683, -4.025696239093874418 ) ) ;
#32773 = LINE ( 'NONE', #14412, #36575 ) ;
#32774 = EDGE_CURVE ( 'NONE', #22827, #31513, #25243, .T. ) ;
#32775 = CARTESIAN_POINT ( 'NONE',  ( 16.11725891507163766, 15.27317977277692052, -2.500000000000000000 ) ) ;
#32776 = FACE_OUTER_BOUND ( 'NONE', #15415, .T. ) ;
#32777 = CARTESIAN_POINT ( 'NONE',  ( -1.261861663380802412, -27.90107892266405898, 7.691066658568947112 ) ) ;
#32778 = CARTESIAN_POINT ( 'NONE',  ( -16.44874870218064089, -26.64985754041175525, 6.800000000000000711 ) ) ;
#32779 = CARTESIAN_POINT ( 'NONE',  ( 81.85640814870976101, 64.68575429476388194, 2.512558077907662391 ) ) ;
#32780 = CARTESIAN_POINT ( 'NONE',  ( 86.46420362610733434, 1.237027245193318192, -5.068583899740296772 ) ) ;
#32781 = CARTESIAN_POINT ( 'NONE',  ( 31.96174557538834193, -4.583587016071825282, 3.235063174744643000 ) ) ;
#32782 = CARTESIAN_POINT ( 'NONE',  ( -77.92837670882107659, 2.429809908903242999, 15.50000000000000000 ) ) ;
#32783 = CARTESIAN_POINT ( 'NONE',  ( 3.489554929392924887, -26.67873662699589588, 6.864651958020304257 ) ) ;
#32784 = CARTESIAN_POINT ( 'NONE',  ( -81.53531961795309257, -5.628198604101866565, -2.656554173279100262 ) ) ;
#32785 = EDGE_LOOP ( 'NONE', ( #7026, #1623, #16873, #29340 ) ) ;
#32786 = CARTESIAN_POINT ( 'NONE',  ( -0.5260552471568549215, -32.13955055026278274, 6.889465824494256374 ) ) ;
#32787 = CARTESIAN_POINT ( 'NONE',  ( 0.1138761091961189020, -26.45015881701811011, 6.921725064902953584 ) ) ;
#32788 = CARTESIAN_POINT ( 'NONE',  ( 37.00281670377963650, -2.989080459751201069, -5.981582481765331138 ) ) ;
#32789 = CARTESIAN_POINT ( 'NONE',  ( -4.878675913592187108, -26.64985754041175525, 6.700000000000000178 ) ) ;
#32790 = CARTESIAN_POINT ( 'NONE',  ( -1.645585159361036220, -30.17362680341680203, 7.635761828346577573 ) ) ;
#32791 = DIRECTION ( 'NONE',  ( 0.000000000000000000, 0.000000000000000000, 1.000000000000000000 ) ) ;
#32792 = EDGE_CURVE ( 'NONE', #2057, #19833, #30941, .T. ) ;
#32793 = CARTESIAN_POINT ( 'NONE',  ( 11.29080664838499182, -35.94265729135299381, 2.500000000000000000 ) ) ;
#32794 = CARTESIAN_POINT ( 'NONE',  ( 4.320748559849963755, -31.73643811260259184, 7.740055089680397238 ) ) ;
#32795 = ORIENTED_EDGE ( 'NONE', *, *, #16135, .T. ) ;
#32796 = CARTESIAN_POINT ( 'NONE',  ( 34.78032543754396499, -3.716931077528784044, 5.478572017771286440 ) ) ;
#32797 = DIRECTION ( 'NONE',  ( -0.7541618601367592323, 0.000000000000000000, 0.6566885781822789925 ) ) ;
#32798 = CARTESIAN_POINT ( 'NONE',  ( 67.69980720754315939, 58.37350455430767937, -3.995247128881052046 ) ) ;
#32799 = AXIS2_PLACEMENT_3D ( 'NONE', #11975, #37107, #27837 ) ;
#32800 = CARTESIAN_POINT ( 'NONE',  ( 3.060248756071702214, -26.34490546765821861, 7.006908160621411419 ) ) ;
#32801 = ORIENTED_EDGE ( 'NONE', *, *, #39491, .T. ) ;
#32802 = CARTESIAN_POINT ( 'NONE',  ( -14.34874870218063769, -26.64985754041175525, 6.700000000000000178 ) ) ;
#32803 = DIRECTION ( 'NONE',  ( 0.3420201433256748746, -0.9396926207859060964, 0.000000000000000000 ) ) ;
#32804 = CARTESIAN_POINT ( 'NONE',  ( -2.248748702180634940, -26.64985754041175525, 6.800000000000000711 ) ) ;
#32805 = CARTESIAN_POINT ( 'NONE',  ( 2.326139153815881322, -32.91185150465383202, 7.692469944509197965 ) ) ;
#32806 = CARTESIAN_POINT ( 'NONE',  ( -1.471942004329455544, -28.34666765933866728, 6.880147297696980857 ) ) ;
#32807 = FACE_OUTER_BOUND ( 'NONE', #26752, .T. ) ;
#32808 = CARTESIAN_POINT ( 'NONE',  ( -1.699608699875451379, -29.56706542154453388, 7.769368695748485543 ) ) ;
#32809 = ORIENTED_EDGE ( 'NONE', *, *, #15044, .F. ) ;
#32810 = CARTESIAN_POINT ( 'NONE',  ( 22.38279560817339586, 4.933722530806304185, 3.054152587046873979 ) ) ;
#32811 = CARTESIAN_POINT ( 'NONE',  ( -1.741284284048380426, -30.20623001897737581, 7.730015791551952731 ) ) ;
#32812 = CARTESIAN_POINT ( 'NONE',  ( 79.22373596144829833, 65.64748706429476499, 2.718470589328619624 ) ) ;
#32813 = B_SPLINE_CURVE_WITH_KNOTS ( 'NONE', 3,
 ( #23298, #16499, #17098, #25581, #25989, #38126, #9928, #22510, #35074, #19404, #38523, #31976, #35471, #19806, #22903, #32377 ),
 .UNSPECIFIED., .F., .F.,
 ( 4, 3, 3, 3, 3, 4 ),
 ( 0.000000000000000000, 3.025570593002918873E-05, 6.051145698343720649E-05, 9.076621574721710701E-05, 0.0001210204262067937652, 0.0001477827378591783816 ),
 .UNSPECIFIED. ) ;
#32814 = CARTESIAN_POINT ( 'NONE',  ( -18.34874870218063947, -26.64985754041175525, 6.700000000000000178 ) ) ;
#32815 = ORIENTED_EDGE ( 'NONE', *, *, #9428, .F. ) ;
#32816 = CARTESIAN_POINT ( 'NONE',  ( 78.34436985318809832, 64.89959302631085336, -3.091829831932941808 ) ) ;
#32817 = CARTESIAN_POINT ( 'NONE',  ( 26.05852442447088890, 0.7874726545580505999, 4.421626571207251999 ) ) ;
#32818 = CARTESIAN_POINT ( 'NONE',  ( 81.43955525003346452, 63.33353925140134066, -3.171364025122245689 ) ) ;
#32819 = CARTESIAN_POINT ( 'NONE',  ( 79.60787101065389493, 62.86536646861405586, 3.718817779187657990 ) ) ;
#32820 = ORIENTED_EDGE ( 'NONE', *, *, #19440, .T. ) ;
#32821 = DIRECTION ( 'NONE',  ( -1.000000000000000000, -0.000000000000000000, -0.000000000000000000 ) ) ;
#32822 = CARTESIAN_POINT ( 'NONE',  ( 82.45631153319118312, 62.87735296625318426, 1.118100487915077546 ) ) ;
#32823 = LINE ( 'NONE', #21067, #24877 ) ;
#32824 = CARTESIAN_POINT ( 'NONE',  ( 24.14839210154553584, 1.598524049810922998, 6.350534879451781300 ) ) ;
#32825 = CARTESIAN_POINT ( 'NONE',  ( -64.59661209699989115, 34.69995260619734267, -6.002488439271949083 ) ) ;
#32826 = ORIENTED_EDGE ( 'NONE', *, *, #21184, .F. ) ;
#32827 = CARTESIAN_POINT ( 'NONE',  ( -79.18352549070058899, -5.465004164923950469, 7.520925182975014778 ) ) ;
#32828 = CARTESIAN_POINT ( 'NONE',  ( 27.40045544475674077, 1.045213952888590203, -4.482696246924063210 ) ) ;
#32829 = ADVANCED_FACE ( 'NONE', ( #15472 ), #33430, .F. ) ;
#32830 = AXIS2_PLACEMENT_3D ( 'NONE', #19267, #29142, #13084 ) ;
#32831 = DIRECTION ( 'NONE',  ( 0.9396926207859126468, -0.3420201433256568335, -0.000000000000000000 ) ) ;
#32832 = CARTESIAN_POINT ( 'NONE',  ( -1.323924960262854666, -31.33161076090960151, 7.635761828346577573 ) ) ;
#32833 = EDGE_CURVE ( 'NONE', #141, #40670, #39983, .T. ) ;
#32834 = CARTESIAN_POINT ( 'NONE',  ( 35.83198913069367819, -3.726957495236238760, -5.625159356461098881 ) ) ;
#32835 = DIRECTION ( 'NONE',  ( -0.4690749385695657803, -0.8831583674551003460, 0.000000000000000000 ) ) ;
#32836 = CARTESIAN_POINT ( 'NONE',  ( 3.235878913814441038, -32.60345520914638939, 7.013842709614101167 ) ) ;
#32837 = CARTESIAN_POINT ( 'NONE',  ( 5.111256656961197464, -30.35480174692847655, 6.998987538705433664 ) ) ;
#32838 = CARTESIAN_POINT ( 'NONE',  ( -71.12575595825015284, -48.60721477804613500, 5.997525359197725336 ) ) ;
#32839 = CARTESIAN_POINT ( 'NONE',  ( 2.699327306250907110, -32.81987240510260762, 6.882085323592685100 ) ) ;
#32840 = ADVANCED_FACE ( 'NONE', ( #30525 ), #2334, .T. ) ;
#32841 = CARTESIAN_POINT ( 'NONE',  ( 1.863139223285963597, -26.07370920805947279, 6.887547729233689076 ) ) ;
#32842 = EDGE_CURVE ( 'NONE', #28994, #37415, #3526, .T. ) ;
#32843 = AXIS2_PLACEMENT_3D ( 'NONE', #16245, #618, #38264 ) ;
#32844 = VERTEX_POINT ( 'NONE', #19593 ) ;
#32845 = EDGE_LOOP ( 'NONE', ( #30835, #5543, #31961, #9259 ) ) ;
#32846 = CARTESIAN_POINT ( 'NONE',  ( 66.41505992881667453, 57.81052748253015494, 4.000000000000021316 ) ) ;
#32847 = CARTESIAN_POINT ( 'NONE',  ( 72.12755885004493450, 59.87634726091143023, -3.962431611477345239 ) ) ;
#32848 = ORIENTED_EDGE ( 'NONE', *, *, #33013, .T. ) ;
#32849 = CARTESIAN_POINT ( 'NONE',  ( 0.1708817620810553495, -26.53337799465926494, 7.006423389747790331 ) ) ;
#32850 = CARTESIAN_POINT ( 'NONE',  ( -1.250824363190944588, -27.88163718980674233, 7.635761828346577573 ) ) ;
#32851 = CARTESIAN_POINT ( 'NONE',  ( -79.56308247960363644, 10.39758802068803689, -7.037846573057998434 ) ) ;
#32852 = APPLICATION_PROTOCOL_DEFINITION ( 'draft international standard', 'automotive_design', 1998, #26585 ) ;
#32853 = CARTESIAN_POINT ( 'NONE',  ( 2.303438722708047059, -32.91602753032043438, 7.756377446753163873 ) ) ;
#32854 = DIRECTION ( 'NONE',  ( 1.000000000000000000, 0.000000000000000000, 0.000000000000000000 ) ) ;
#32855 = AXIS2_PLACEMENT_3D ( 'NONE', #4180, #19810, #38131 ) ;
#32856 = LINE ( 'NONE', #32658, #35936 ) ;
#32857 = VERTEX_POINT ( 'NONE', #31959 ) ;
#32858 = ORIENTED_EDGE ( 'NONE', *, *, #10159, .F. ) ;
#32859 = CARTESIAN_POINT ( 'NONE',  ( 78.49831277043062983, 65.85142261852138290, -1.827177995460260718 ) ) ;
#32860 = CARTESIAN_POINT ( 'NONE',  ( 33.84452642184018600, -5.136433483475361328, 2.685500998610346191 ) ) ;
#32861 = CARTESIAN_POINT ( 'NONE',  ( 79.82585920882016239, 63.98597419336261538, 3.710743084827283322 ) ) ;
#32862 = DIRECTION ( 'NONE',  ( 0.000000000000000000, 0.000000000000000000, 1.000000000000000000 ) ) ;
#32863 = CARTESIAN_POINT ( 'NONE',  ( 1.121324086407811338, -24.55319635012989110, 6.800000000000000711 ) ) ;
#32864 = AXIS2_PLACEMENT_3D ( 'NONE', #70, #35665, #7433 ) ;
#32865 = CARTESIAN_POINT ( 'NONE',  ( 17.03316807477964190, 9.497738621113558821, -2.806674216866353433 ) ) ;
#32866 = LINE ( 'NONE', #23976, #37996 ) ;
#32867 = CARTESIAN_POINT ( 'NONE',  ( 21.85643539959777115, -1.425092139247138734, 16.06258187428232986 ) ) ;
#32868 = VERTEX_POINT ( 'NONE', #3761 ) ;
#32869 = DIRECTION ( 'NONE',  ( -0.000000000000000000, 0.000000000000000000, 1.000000000000000000 ) ) ;
#32870 = CARTESIAN_POINT ( 'NONE',  ( 14.68539687963933282, -4.701488008871138824, 2.500000000000806466 ) ) ;
#32871 = CARTESIAN_POINT ( 'NONE',  ( -75.97102281476716712, -3.971666016424915124, -8.662871507693417072 ) ) ;
#32872 = CARTESIAN_POINT ( 'NONE',  ( 1.493410003970609523, -32.96362645543517544, 6.979335674598003969 ) ) ;
#32873 = DIRECTION ( 'NONE',  ( -0.5000000000000039968, 0.8660254037844362651, -0.000000000000000000 ) ) ;
#32874 = CARTESIAN_POINT ( 'NONE',  ( 79.55653453243731121, 65.56957575487831491, 2.861733672647126525 ) ) ;
#32875 = LINE ( 'NONE', #32676, #7132 ) ;
#32876 = CARTESIAN_POINT ( 'NONE',  ( 3.908975219192432515, -26.98494435337591923, 7.782167645815903256 ) ) ;
#32877 = CARTESIAN_POINT ( 'NONE',  ( -1.391086531092725398, -31.21089766107228414, 7.751599049952174525 ) ) ;
#32878 = DIRECTION ( 'NONE',  ( 1.000000000000000000, 0.000000000000000000, 0.000000000000000000 ) ) ;
#32879 = CARTESIAN_POINT ( 'NONE',  ( 0.5828135686266351367, -26.25315121703935972, 6.865554069792297653 ) ) ;
#32880 = CIRCLE ( 'NONE', #29579, 3.784187430299790211 ) ;
#32881 = EDGE_CURVE ( 'NONE', #28588, #15750, #3542, .T. ) ;
#32882 = CARTESIAN_POINT ( 'NONE',  ( 4.489505707918894473, -27.45549474512610644, 7.009310105710486738 ) ) ;
#32883 = CARTESIAN_POINT ( 'NONE',  ( -75.45330471031414277, 33.71485196875532608, -8.800414904976364028 ) ) ;
#32884 = EDGE_CURVE ( 'NONE', #16289, #33366, #15744, .T. ) ;
#32885 = CARTESIAN_POINT ( 'NONE',  ( 5.112373171067981836, -30.38002035509909149, 7.387053503561887169 ) ) ;
#32886 = CARTESIAN_POINT ( 'NONE',  ( 4.268193593992276824, -31.79846898303070191, 6.887041543973309032 ) ) ;
#32887 = CARTESIAN_POINT ( 'NONE',  ( -72.95330471031414277, 33.71485196875532608, -8.800414904976364028 ) ) ;
#32888 = CARTESIAN_POINT ( 'NONE',  ( 68.12732179974642577, 58.11841597887141120, 3.982418445723222789 ) ) ;
#32889 = CARTESIAN_POINT ( 'NONE',  ( 36.91179562721963947, -2.638184243151847852, 5.967376441415058075 ) ) ;
#32890 = CARTESIAN_POINT ( 'NONE',  ( 14.61802081865033642, 12.33286846116284252, -2.500000000000000000 ) ) ;
#32891 = CARTESIAN_POINT ( 'NONE',  ( 87.10205511408864254, 0.5205621796347451591, 5.292648712017772539 ) ) ;
#32892 = VECTOR ( 'NONE', #28660, 1000.000000000000000 ) ;
#32894 = CARTESIAN_POINT ( 'NONE',  ( -80.19065981525226050, 31.27226540113725406, 9.800414904976365804 ) ) ;
#32893 = CARTESIAN_POINT ( 'NONE',  ( 78.96442931663766274, 65.90663607296401949, -2.147349935851027958 ) ) ;
#32895 = CARTESIAN_POINT ( 'NONE',  ( -1.307348999084261276, -27.78007364502682464, 6.880608371227948439 ) ) ;
#32896 = CARTESIAN_POINT ( 'NONE',  ( 2.296057149099136829, -26.12098725511343389, 7.756742906098588186 ) ) ;
#32897 = EDGE_LOOP ( 'NONE', ( #34691, #23556, #16617, #24639 ) ) ;
#32898 = CARTESIAN_POINT ( 'NONE',  ( -78.06330667992513384, 11.25813893609656802, -7.018729043671574352 ) ) ;
#32899 = CARTESIAN_POINT ( 'NONE',  ( 24.31240841717447410, -6.336097543977142976, -2.705716385158337012 ) ) ;
#32900 = ORIENTED_EDGE ( 'NONE', *, *, #5381, .F. ) ;
#32901 = CARTESIAN_POINT ( 'NONE',  ( -71.71319929822489314, -21.40271194095481633, 3.948449672239095598 ) ) ;
#32902 = CARTESIAN_POINT ( 'NONE',  ( 81.09158065085919986, 61.31869227828924807, -1.634613895560571573 ) ) ;
#32903 = LINE ( 'NONE', #35602, #10203 ) ;
#32904 = CARTESIAN_POINT ( 'NONE',  ( 80.08517677095778708, 64.13476336867732641, 3.668443954219271053 ) ) ;
#32905 = CARTESIAN_POINT ( 'NONE',  ( 21.75407835734251805, 0.6912123640297617166, 8.027689290590526383 ) ) ;
#32907 = EDGE_LOOP ( 'NONE', ( #13515, #33343, #36120, #17622 ) ) ;
#32906 = CARTESIAN_POINT ( 'NONE',  ( -0.7753363873652329152, -27.23952712957111544, 6.903372536218459032 ) ) ;
#32908 = CIRCLE ( 'NONE', #15140, 0.1000000000000028644 ) ;
#32910 = DIRECTION ( 'NONE',  ( 1.000000000000000000, 0.000000000000000000, 0.000000000000000000 ) ) ;
#32909 = CARTESIAN_POINT ( 'NONE',  ( 14.69558838330753758, 3.996311804371543985, -6.000000000000000000 ) ) ;
#32911 = CARTESIAN_POINT ( 'NONE',  ( -75.45330471031414277, 33.71485196875532608, 12.49999999999999645 ) ) ;
#32912 = PLANE ( 'NONE',  #29138 ) ;
#32913 = CARTESIAN_POINT ( 'NONE',  ( 23.17722939410916183, 3.712341236063878114, -3.488222722305598822 ) ) ;
#32914 = EDGE_LOOP ( 'NONE', ( #25646, #12722, #17771, #30726 ) ) ;
#32915 = CARTESIAN_POINT ( 'NONE',  ( 1.700390093233090871, -29.56993018339339940, 27.90461065042423527 ) ) ;
#32916 = CARTESIAN_POINT ( 'NONE',  ( 22.31759743831440090, 6.226164879696757026, 1.431367841762869686 ) ) ;
#32917 = CIRCLE ( 'NONE', #38163, 2.500000000000002220 ) ;
#32918 = CARTESIAN_POINT ( 'NONE',  ( 16.61473264793675853, 9.888384249099596346, 2.499999999999963585 ) ) ;
#32919 = ORIENTED_EDGE ( 'NONE', *, *, #11321, .T. ) ;
#32920 = CARTESIAN_POINT ( 'NONE',  ( 0.3430336670258780640, -32.68723412389003613, 6.969307238440504371 ) ) ;
#32921 = CARTESIAN_POINT ( 'NONE',  ( 79.02544788879011151, 66.13175326451143121, 1.679744683813971129 ) ) ;
#32922 = CARTESIAN_POINT ( 'NONE',  ( 86.35968278939613185, 0.3242946576005459325, -6.017936684944984016 ) ) ;
#32923 = DIRECTION ( 'NONE',  ( -1.000000000000000000, 0.000000000000000000, 0.000000000000000000 ) ) ;
#32924 = ORIENTED_EDGE ( 'NONE', *, *, #17073, .T. ) ;
#32925 = PLANE ( 'NONE',  #31944 ) ;
#32926 = ORIENTED_EDGE ( 'NONE', *, *, #12468, .F. ) ;
#32927 = CARTESIAN_POINT ( 'NONE',  ( -1.237321756456247979, -31.28161037787917209, 7.635761828346577573 ) ) ;
#32928 = CARTESIAN_POINT ( 'NONE',  ( -41.07867591359219972, -26.64985754041175525, 6.700000000000000178 ) ) ;
#32929 = CARTESIAN_POINT ( 'NONE',  ( 18.21053797601233981, -2.853449834380734185, -3.048592893318725405 ) ) ;
#32930 = EDGE_CURVE ( 'NONE', #32438, #39701, #4457, .T. ) ;
#32931 = CARTESIAN_POINT ( 'NONE',  ( 36.63295709802978450, -3.078046445090460992, -5.923856945199692525 ) ) ;
#32932 = LINE ( 'NONE', #23455, #19416 ) ;
#32933 = CARTESIAN_POINT ( 'NONE',  ( 84.54498636705716308, 2.468675992724178592, -3.632217660620454147 ) ) ;
#32934 = CARTESIAN_POINT ( 'NONE',  ( 3.916835083226508640, -26.85238689360580011, 7.255881584735162093 ) ) ;
#32935 = ORIENTED_EDGE ( 'NONE', *, *, #7128, .T. ) ;
#32936 = LINE ( 'NONE', #7405, #15816 ) ;
#32937 = AXIS2_PLACEMENT_3D ( 'NONE', #14480, #35930, #36525 ) ;
#32938 = CARTESIAN_POINT ( 'NONE',  ( 3.431434570054125111, -32.49627346798381211, 7.693875151218753317 ) ) ;
#32939 = CARTESIAN_POINT ( 'NONE',  ( 31.83101670608917644, -2.965446787480832569, -5.174398011670120034 ) ) ;
#32940 = ORIENTED_EDGE ( 'NONE', *, *, #4528, .F. ) ;
#32941 = VERTEX_POINT ( 'NONE', #34444 ) ;
#32942 = CARTESIAN_POINT ( 'NONE',  ( 37.00966539048157955, -2.249461300321922597, 5.913205627773911566 ) ) ;
#32943 =( BOUNDED_CURVE ( )  B_SPLINE_CURVE ( 3, ( #11227, #23995, #2422, #11840 ),
 .UNSPECIFIED., .F., .T. ) 
 B_SPLINE_CURVE_WITH_KNOTS ( ( 4, 4 ),
 ( 4.748221474220561511, 4.941946782021395812 ),
 .UNSPECIFIED. ) 
 CURVE ( )  GEOMETRIC_REPRESENTATION_ITEM ( )  RATIONAL_B_SPLINE_CURVE ( ( 1.000000000000000000, 0.9968749865767494445, 0.9968749865767494445, 1.000000000000000000 ) ) 
 REPRESENTATION_ITEM ( '' )  );
#32944 = CARTESIAN_POINT ( 'NONE',  ( -0.5390062018526512455, -32.25974509032589310, 7.635761828346574021 ) ) ;
#32945 = CARTESIAN_POINT ( 'NONE',  ( 33.46455515056310759, -3.089188617792877789, 5.429351193206847448 ) ) ;
#32946 = CARTESIAN_POINT ( 'NONE',  ( 87.82805078818662992, -2.393880730231491061, -1.766410623985958050 ) ) ;
#32947 = ORIENTED_EDGE ( 'NONE', *, *, #2457, .T. ) ;
#32948 = ORIENTED_EDGE ( 'NONE', *, *, #32745, .T. ) ;
#32949 = AXIS2_PLACEMENT_3D ( 'NONE', #38130, #31770, #28057 ) ;
#32950 = CARTESIAN_POINT ( 'NONE',  ( 5.140800898748325132, -28.92683337905274854, 7.698786668945011513 ) ) ;
#32951 =( LENGTH_UNIT ( ) NAMED_UNIT ( * ) SI_UNIT ( .MILLI., .METRE. ) );
#32952 = DIRECTION ( 'NONE',  ( 1.000000000000000000, -8.959828616340678715E-16, 0.000000000000000000 ) ) ;
#32953 = ADVANCED_FACE ( 'NONE', ( #3168 ), #9709, .F. ) ;
#32954 = CARTESIAN_POINT ( 'NONE',  ( 4.797166834205789598, -27.93896158646020211, 6.870724624169667116 ) ) ;
#32955 = VERTEX_POINT ( 'NONE', #3560 ) ;
#32956 = CARTESIAN_POINT ( 'NONE',  ( 23.41651709676641246, 3.612060057188777318, 3.413386634271887932 ) ) ;
#32957 = CARTESIAN_POINT ( 'NONE',  ( 81.45638069295013395, 61.46019730367517298, -1.134074597586742783 ) ) ;
#32958 = CARTESIAN_POINT ( 'NONE',  ( -1.321941654078521378, -31.33501114731328130, 7.749999999999999112 ) ) ;
#32959 = VERTEX_POINT ( 'NONE', #6830 ) ;
#32961 = CARTESIAN_POINT ( 'NONE',  ( 16.18297655557976711, -3.318851087015777690, -2.732142896901965656 ) ) ;
#32960 = CARTESIAN_POINT ( 'NONE',  ( -0.01583764436594936598, -26.63487271330943784, 7.748216051605115950 ) ) ;
#32962 = CARTESIAN_POINT ( 'NONE',  ( -72.84815947045233031, 2.429809908903243443, 12.50000000000000000 ) ) ;
#32963 = CARTESIAN_POINT ( 'NONE',  ( 76.01163379375532259, 60.38783671147731980, 3.615102801931016074 ) ) ;
#32964 = ORIENTED_EDGE ( 'NONE', *, *, #36302, .T. ) ;
#32965 = CARTESIAN_POINT ( 'NONE',  ( 23.54860076899586119, 2.870803210893150048, -4.024937523241188586 ) ) ;
#32966 = CARTESIAN_POINT ( 'NONE',  ( -64.08758708074093136, 38.00013147421745430, 4.165003120435059714 ) ) ;
#32967 = VECTOR ( 'NONE', #8690, 1000.000000000000000 ) ;
#32968 = EDGE_CURVE ( 'NONE', #5208, #40141, #665, .T. ) ;
#32969 = FACE_OUTER_BOUND ( 'NONE', #20860, .T. ) ;
#32970 = DIRECTION ( 'NONE',  ( 1.000000000000000000, 0.000000000000000000, 0.000000000000000000 ) ) ;
#32971 = CARTESIAN_POINT ( 'NONE',  ( 0.3454438073157775624, -0.5999999999999994227, -3.946157045896701021 ) ) ;
#32972 = CARTESIAN_POINT ( 'NONE',  ( -11.07867591359219794, -26.64985754041175525, 6.700000000000000178 ) ) ;
#32973 = CARTESIAN_POINT ( 'NONE',  ( 78.68849923766543952, 66.05725436416432217, 1.045986116561638202 ) ) ;
#32974 = CARTESIAN_POINT ( 'NONE',  ( 88.37152744968734908, -0.9053694005015545665, 0.1944390934057901588 ) ) ;
#32975 = CARTESIAN_POINT ( 'NONE',  ( 28.89923929355584065, 0.07307017450661948410, 5.719397691353443669 ) ) ;
#32976 = DIRECTION ( 'NONE',  ( -1.000000000000000000, 0.000000000000000000, 0.000000000000000000 ) ) ;
#32977 = CARTESIAN_POINT ( 'NONE',  ( 3.516368447621620597, -26.69550461626186078, 6.865312560952602894 ) ) ;
#32978 = CARTESIAN_POINT ( 'NONE',  ( -77.35749566552371448, -4.820597592931324726, -9.230088820010045936 ) ) ;
#32979 = CARTESIAN_POINT ( 'NONE',  ( -0.5281487064042170720, -32.13773368415257892, 6.887041543973312585 ) ) ;
#32980 = CARTESIAN_POINT ( 'NONE',  ( 0.1039781302203472563, -26.45521208309125427, 7.006908160621415860 ) ) ;
#32981 = AXIS2_PLACEMENT_3D ( 'NONE', #29862, #1079, #14207 ) ;
#32982 = EDGE_CURVE ( 'NONE', #39757, #31915, #38911, .T. ) ;
#32983 = CARTESIAN_POINT ( 'NONE',  ( 32.84225399592710914, -0.7495783096613907182, -5.332226047615563402 ) ) ;
#32984 = EDGE_CURVE ( 'NONE', #29208, #699, #20379, .T. ) ;
#32985 = DIRECTION ( 'NONE',  ( 1.000000000000000000, 1.273455763949465563E-16, 0.000000000000000000 ) ) ;
#32986 = CARTESIAN_POINT ( 'NONE',  ( -57.16504416091206053, 33.41445838748276742, -4.000000000000000000 ) ) ;
#32987 = CARTESIAN_POINT ( 'NONE',  ( -63.45304970008103140, 43.00143306355779771, -3.444018727593662899 ) ) ;
#32988 = CYLINDRICAL_SURFACE ( 'NONE', #40150, 0.1000000000000028644 ) ;
#32989 = ORIENTED_EDGE ( 'NONE', *, *, #1837, .F. ) ;
#32990 = CARTESIAN_POINT ( 'NONE',  ( 34.51602972922534462, -1.013642683923393184, 5.504862190214542927 ) ) ;
#32991 = CARTESIAN_POINT ( 'NONE',  ( -62.92837670882106238, -42.37473357531882812, -6.000000000000000000 ) ) ;
#32992 = CARTESIAN_POINT ( 'NONE',  ( 67.13660786288076565, 58.10023080654656980, -3.998533043703386802 ) ) ;
#32993 = EDGE_CURVE ( 'NONE', #12399, #21663, #16665, .T. ) ;
#32994 = CARTESIAN_POINT ( 'NONE',  ( 3.024292301338818323, -26.32996603374844824, 6.870724624169665340 ) ) ;
#32995 = ORIENTED_EDGE ( 'NONE', *, *, #30893, .T. ) ;
#32996 = LINE ( 'NONE', #14037, #6839 ) ;
#32997 = EDGE_CURVE ( 'NONE', #25861, #31660, #9313, .T. ) ;
#32998 = CARTESIAN_POINT ( 'NONE',  ( 3.791157483716739218, -32.25110375459131973, 7.754798119455333705 ) ) ;
#32999 = CARTESIAN_POINT ( 'NONE',  ( 84.97506497612948806, 1.907738733390036856, -4.849904034997914337 ) ) ;
#33000 = CARTESIAN_POINT ( 'NONE',  ( 0.9076429196643266417, -32.87621993457957359, 6.929923840112063971 ) ) ;
#33001 = CARTESIAN_POINT ( 'NONE',  ( 3.613844859187792746, -26.63928332947567057, 6.941203072598477242 ) ) ;
#33002 = CARTESIAN_POINT ( 'NONE',  ( -1.699609515697033890, -29.56803366691413970, 7.768698451128750904 ) ) ;
#33003 = EDGE_LOOP ( 'NONE', ( #38447, #21362, #9756, #11934 ) ) ;
#33004 = CARTESIAN_POINT ( 'NONE',  ( 22.61565167955079758, 4.617847287593741079, 3.051803804880747872 ) ) ;
#33005 = CARTESIAN_POINT ( 'NONE',  ( 80.99721608130789718, 62.45573281339171956, 3.163072811751561186 ) ) ;
#33006 = AXIS2_PLACEMENT_3D ( 'NONE', #39674, #8168, #2450 ) ;
#33007 = CARTESIAN_POINT ( 'NONE',  ( -63.61790918070564516, 43.90188359253805572, 2.582768616493209990 ) ) ;
#33008 = ORIENTED_EDGE ( 'NONE', *, *, #40270, .F. ) ;
#33009 = CARTESIAN_POINT ( 'NONE',  ( 77.57568143946795658, 64.97578145858240362, -2.643019404356976576 ) ) ;
#33011 = CARTESIAN_POINT ( 'NONE',  ( 14.74217871668694890, -5.108457001575695600, -2.500000000000635936 ) ) ;
#33010 = CARTESIAN_POINT ( 'NONE',  ( 22.28556628514242988, 0.2471207394018046788, 7.129339672946321649 ) ) ;
#33012 = EDGE_CURVE ( 'NONE', #39035, #2944, #20575, .T. ) ;
#33013 = EDGE_CURVE ( 'NONE', #13756, #39610, #24564, .T. ) ;
#33014 = CARTESIAN_POINT ( 'NONE',  ( 81.59170830166485189, 62.44397035145045294, -2.684801069570277310 ) ) ;
#33015 = CARTESIAN_POINT ( 'NONE',  ( 78.78025785238997969, 63.39248666165328672, 3.791687334209851379 ) ) ;
#33016 = ORIENTED_EDGE ( 'NONE', *, *, #14164, .F. ) ;
#33017 = EDGE_CURVE ( 'NONE', #35820, #38408, #25974, .T. ) ;
#33018 = LINE ( 'NONE', #33220, #39177 ) ;
#33019 = CARTESIAN_POINT ( 'NONE',  ( 82.17153865661313716, 64.85009419791106211, 1.775718711109096404 ) ) ;
#33020 = CARTESIAN_POINT ( 'NONE',  ( 37.83867290611771494, -6.084034091406928191, -6.000000000000000000 ) ) ;
#33021 = CARTESIAN_POINT ( 'NONE',  ( 27.87470673840761037, 2.608020033772324275, -0.5247038454205935620 ) ) ;
#33022 = CARTESIAN_POINT ( 'NONE',  ( -1.323924960262854666, -31.33161076090960151, 7.635761828346577573 ) ) ;
#33023 = ORIENTED_EDGE ( 'NONE', *, *, #35267, .T. ) ;
#33024 = CARTESIAN_POINT ( 'NONE',  ( -80.83093704390071821, -5.699917940215170731, 1.450021397597311301 ) ) ;
#33025 = CARTESIAN_POINT ( 'NONE',  ( 23.59548752951696571, 0.4310456963235400618, -5.519663247815086216 ) ) ;
#33026 = DIRECTION ( 'NONE',  ( 1.000000000000000000, 0.000000000000000000, 0.000000000000000000 ) ) ;
#33027 = FACE_OUTER_BOUND ( 'NONE', #16398, .T. ) ;
#33028 = CARTESIAN_POINT ( 'NONE',  ( 37.21106504267930148, -2.744214598291488727, -6.000909659284667796 ) ) ;
#33029 = LINE ( 'NONE', #38374, #35188 ) ;
#33030 = FACE_OUTER_BOUND ( 'NONE', #33003, .T. ) ;
#33031 = CARTESIAN_POINT ( 'NONE',  ( -72.95330471031414277, 33.71485196875532608, -12.49999999999999645 ) ) ;
#33032 = CARTESIAN_POINT ( 'NONE',  ( -72.38866088156714795, -47.51164815211338066, 5.820093912444312956 ) ) ;
#33033 = DIRECTION ( 'NONE',  ( 1.682730792515357087E-16, -1.000000000000000000, 0.000000000000000000 ) ) ;
#33034 = CARTESIAN_POINT ( 'NONE',  ( 2.187796539937281182, -33.03559314236433408, 7.754798119455333705 ) ) ;
#33035 = CARTESIAN_POINT ( 'NONE',  ( 1.815759002417408396, -26.07183212662117455, 6.865482280155368322 ) ) ;
#33036 = CARTESIAN_POINT ( 'NONE',  ( 23.51788449541176007, 1.295866407298160716, -5.129232269930078303 ) ) ;
#33037 = CARTESIAN_POINT ( 'NONE',  ( 2.155604402987680857, -33.04021322912456782, 6.880828092187096345 ) ) ;
#33038 = ORIENTED_EDGE ( 'NONE', *, *, #6530, .F. ) ;
#33039 = CARTESIAN_POINT ( 'NONE',  ( 66.27376694608996388, 57.73522568913447373, 4.000000000000000000 ) ) ;
#33040 = CARTESIAN_POINT ( 'NONE',  ( 71.62240613637702324, 61.07494268190701092, -3.699617110277040766 ) ) ;
#33041 = AXIS2_PLACEMENT_3D ( 'NONE', #36085, #17115, #29887 ) ;
#33042 = ORIENTED_EDGE ( 'NONE', *, *, #13156, .T. ) ;
#33043 = CARTESIAN_POINT ( 'NONE',  ( 84.21289197705223728, 3.045783863710543660, -0.4930364517660317802 ) ) ;
#33044 = CARTESIAN_POINT ( 'NONE',  ( -0.6943239642360979902, -27.00805212371037456, 7.139344958878412584 ) ) ;
#33045 = DIRECTION ( 'NONE',  ( -0.8888117386314180468, -0.4582725098355734938, 0.000000000000000000 ) ) ;
#33046 = CARTESIAN_POINT ( 'NONE',  ( -0.9190822194230292563, -27.24862244995199845, 6.863805608295730387 ) ) ;
#33047 =( NAMED_UNIT ( * ) PLANE_ANGLE_UNIT ( ) SI_UNIT ( $, .RADIAN. ) );
#33048 = EDGE_CURVE ( 'NONE', #37911, #20726, #3574, .T. ) ;
#33049 = DIRECTION ( 'NONE',  ( 0.1303762246624279586, -0.7394003126383905666, -0.6605219282605403475 ) ) ;
#33050 = FACE_OUTER_BOUND ( 'NONE', #12577, .T. ) ;
#33051 = DIRECTION ( 'NONE',  ( -1.000000000000000000, 9.435707606059839439E-16, 0.000000000000000000 ) ) ;
#33052 = CARTESIAN_POINT ( 'NONE',  ( 30.67349724481533002, -3.593355625737403525, 4.777428303402127874 ) ) ;
#33053 = ORIENTED_EDGE ( 'NONE', *, *, #22059, .F. ) ;
#33054 = EDGE_CURVE ( 'NONE', #2740, #1123, #20104, .T. ) ;
#33055 = VERTEX_POINT ( 'NONE', #7828 ) ;
#33056 = CARTESIAN_POINT ( 'NONE',  ( 80.10726245975679660, 62.76215410473258771, -3.584461231902855705 ) ) ;
#33057 = CARTESIAN_POINT ( 'NONE',  ( 33.81811101054934454, -4.997128391572976724, 3.084473742510627670 ) ) ;
#33058 = CARTESIAN_POINT ( 'NONE',  ( 79.50676573472792086, 64.15826028415024496, 3.676305632669318424 ) ) ;
#33059 = AXIS2_PLACEMENT_3D ( 'NONE', #1569, #14101, #36150 ) ;
#33060 = CARTESIAN_POINT ( 'NONE',  ( 0.6310675123731709357, -26.34244895293124600, 7.774064877406527962 ) ) ;
#33061 = EDGE_CURVE ( 'NONE', #5866, #28854, #29952, .T. ) ;
#33062 = CARTESIAN_POINT ( 'NONE',  ( -6.248748702180631831, -26.64985754041175525, 6.700000000000000178 ) ) ;
#33063 = B_SPLINE_CURVE_WITH_KNOTS ( 'NONE', 3,
 ( #17704, #8439, #2922, #30706, #33598, #30283, #5371, #5575, #5782, #27795, #31110, #34218, #17911, #18320, #30491, #40347, #28003, #24717, #2301, #5987, #18115, #24509, #40545, #2513, #15036, #27597, #6801, #32140, #19354, #10279, #31926 ),
 .UNSPECIFIED., .F., .F.,
 ( 4, 3, 3, 3, 3, 3, 3, 3, 3, 3, 4 ),
 ( 9.697399036122160616E-19, 3.077658087705627201E-05, 6.152638666999302836E-05, 9.267501192706609496E-05, 0.0001241882240135191171, 0.0001556618703051675860, 0.0001866161554452220326, 0.0002167966385860974152, 0.0002463805737537785195, 0.0002758761370306537369, 0.0002847094172290068922 ),
 .UNSPECIFIED. ) ;
#33064 = CARTESIAN_POINT ( 'NONE',  ( 16.15319511113404261, 10.47632875577966338, -2.684738856704420584 ) ) ;
#33065 = DIRECTION ( 'NONE',  ( 1.000000000000000000, 0.000000000000000000, 0.000000000000000000 ) ) ;
#33066 = CARTESIAN_POINT ( 'NONE',  ( 21.85643539959774273, 10.29907807357824723, -3.463423532579224418 ) ) ;
#33067 = EDGE_LOOP ( 'NONE', ( #15223, #34904, #12137, #23626 ) ) ;
#33068 = CARTESIAN_POINT ( 'NONE',  ( -76.77456831373793023, 10.78129903716225790, 8.115337217677211612 ) ) ;
#33069 = VECTOR ( 'NONE', #33475, 1000.000000000000000 ) ;
#33070 = CARTESIAN_POINT ( 'NONE',  ( 14.75304912753043496, -4.607437571476275195, 2.508639535167287882 ) ) ;
#33071 = CARTESIAN_POINT ( 'NONE',  ( -73.03883085241794504, 7.296995364254068583, -9.776882264804946487 ) ) ;
#33072 = CARTESIAN_POINT ( 'NONE',  ( 1.259933197038312302, -26.09775540055275656, 7.013842709614101167 ) ) ;
#33073 = CARTESIAN_POINT ( 'NONE',  ( 37.18716061172991516, -2.963873844666090829, -6.000015731507488681 ) ) ;
#33074 = CARTESIAN_POINT ( 'NONE',  ( 81.14908696703564317, 61.29647948322620010, 1.137963815189210193 ) ) ;
#33075 = DIRECTION ( 'NONE',  ( -0.4999999999999918954, -0.8660254037844432595, -0.000000000000000000 ) ) ;
#33076 = CARTESIAN_POINT ( 'NONE',  ( -20.24874870218063805, -26.64985754041175525, 6.800000000000000711 ) ) ;
#33077 = DIRECTION ( 'NONE',  ( 0.000000000000000000, 0.000000000000000000, 1.000000000000000000 ) ) ;
#33078 = CARTESIAN_POINT ( 'NONE',  ( -70.79792407645882690, 0.2170085631122713188, 9.999999999999980460 ) ) ;
#33079 = CARTESIAN_POINT ( 'NONE',  ( 3.021324086407803478, -26.64985754041175525, 6.800000000000000711 ) ) ;
#33080 = CARTESIAN_POINT ( 'NONE',  ( 1.119761070567095285, -33.02143436011441935, 7.655937882338900380 ) ) ;
#33081 = DIRECTION ( 'NONE',  ( 0.000000000000000000, 1.000000000000000000, 0.000000000000000000 ) ) ;
#33082 = CARTESIAN_POINT ( 'NONE',  ( 67.95937142815736820, 58.56762263466062279, 3.988335407916665520 ) ) ;
#33083 = CARTESIAN_POINT ( 'NONE',  ( 22.92221885755501631, 2.655821486554086786, 3.783964647315853469 ) ) ;
#33084 = B_SPLINE_CURVE_WITH_KNOTS ( 'NONE', 3,
 ( #31162, #3785, #6854, #15908, #12612, #28676, #9312, #3585, #28258, #27847 ),
 .UNSPECIFIED., .F., .F.,
 ( 4, 3, 3, 4 ),
 ( 0.0005050348086185285981, 0.0005143352185143270630, 0.0005445898203825176153, 0.0005634294782181690055 ),
 .UNSPECIFIED. ) ;
#33085 = VERTEX_POINT ( 'NONE', #1274 ) ;
#33086 = DIRECTION ( 'NONE',  ( 0.000000000000000000, 0.000000000000000000, 1.000000000000000000 ) ) ;
#33087 = CARTESIAN_POINT ( 'NONE',  ( 88.25986434197210428, -0.7799440980648532085, -3.332403339731401015 ) ) ;
#33089 = CARTESIAN_POINT ( 'NONE',  ( 33.61655304153408252, -1.223667153998024171, -5.453074140175755424 ) ) ;
#33088 = CARTESIAN_POINT ( 'NONE',  ( 81.04779914310620370, 62.47515088512101755, -3.146509185145923038 ) ) ;
#33090 = LINE ( 'NONE', #39040, #30041 ) ;
#33091 = CARTESIAN_POINT ( 'NONE',  ( -1.619634369087763481, -28.83682884688450798, 6.868387053540521592 ) ) ;
#33092 = AXIS2_PLACEMENT_3D ( 'NONE', #3963, #20177, #36437 ) ;
#33093 = CARTESIAN_POINT ( 'NONE',  ( -58.97431419818040155, 27.59684639285647378, 7.041158924856742551 ) ) ;
#33094 = ORIENTED_EDGE ( 'NONE', *, *, #10508, .T. ) ;
#33095 = CARTESIAN_POINT ( 'NONE',  ( -14.97867591359219119, -26.64985754041175525, 6.800000000000000711 ) ) ;
#33096 = ORIENTED_EDGE ( 'NONE', *, *, #34724, .F. ) ;
#33097 = DIRECTION ( 'NONE',  ( 0.6427876096865425826, -0.7660444431189752379, 0.000000000000000000 ) ) ;
#33098 = EDGE_LOOP ( 'NONE', ( #2145, #3327, #15828, #29794 ) ) ;
#33099 = ORIENTED_EDGE ( 'NONE', *, *, #628, .T. ) ;
#33100 = CARTESIAN_POINT ( 'NONE',  ( 79.37669412903225918, 65.14038507876428241, -3.220356845322064565 ) ) ;
#33101 = CARTESIAN_POINT ( 'NONE',  ( -1.531156124662372608, -28.22562180236089802, 6.883550009118464708 ) ) ;
#33102 = CARTESIAN_POINT ( 'NONE',  ( 79.64490966524790849, 64.60885719387560755, 3.518158556798112180 ) ) ;
#33103 = CARTESIAN_POINT ( 'NONE',  ( 22.83213583935611624, 0.9805358558969262672, 5.835874598331055374 ) ) ;
#33105 = EDGE_LOOP ( 'NONE', ( #3930, #37482, #12557, #10695 ) ) ;
#33104 = CARTESIAN_POINT ( 'NONE',  ( 4.787207249339009429, -27.92198779192843716, 7.761113333117551250 ) ) ;
#33106 = ADVANCED_FACE ( 'NONE', ( #29858 ), #10507, .F. ) ;
#33107 = ADVANCED_FACE ( 'NONE', ( #26379 ), #7228, .F. ) ;
#33108 = VECTOR ( 'NONE', #19057, 1000.000000000000000 ) ;
#33110 = EDGE_CURVE ( 'NONE', #38572, #33366, #23676, .T. ) ;
#33109 = FACE_OUTER_BOUND ( 'NONE', #12218, .T. ) ;
#33112 = DIRECTION ( 'NONE',  ( 1.000000000000000000, 1.776143608908745286E-15, 0.000000000000000000 ) ) ;
#33111 = FACE_OUTER_BOUND ( 'NONE', #32139, .T. ) ;
#33113 = CARTESIAN_POINT ( 'NONE',  ( -16.44874870218064089, -26.64985754041175525, 6.700000000000000178 ) ) ;
#33114 = CARTESIAN_POINT ( 'NONE',  ( 1.021324086407808585, -24.55319635012989110, 6.700000000000000178 ) ) ;
#33115 = DIRECTION ( 'NONE',  ( -0.000000000000000000, -0.000000000000000000, 1.000000000000000000 ) ) ;
#33116 = CARTESIAN_POINT ( 'NONE',  ( 22.27850866888861958, 4.871699234913689835, -3.307860320298297019 ) ) ;
#33117 = VERTEX_POINT ( 'NONE', #33160 ) ;
#33118 = CARTESIAN_POINT ( 'NONE',  ( 2.343486897573773486, -33.01034098890863078, 7.698786668945011513 ) ) ;
#33119 = VECTOR ( 'NONE', #9541, 1000.000000000000000 ) ;
#33120 = CARTESIAN_POINT ( 'NONE',  ( 22.79820677575384380, -6.119817767430131283, -4.702819652331462486 ) ) ;
#33121 = CARTESIAN_POINT ( 'NONE',  ( 21.88097534391988219, 3.372061099782372562, 3.393279653752791614 ) ) ;
#33122 = CARTESIAN_POINT ( 'NONE',  ( 2.896448246037522267, -32.75260910491768840, 7.680992449362118002 ) ) ;
#33123 = CARTESIAN_POINT ( 'NONE',  ( 5.100040579096636328, -29.61868030101130245, 6.894806418505348589 ) ) ;
#33124 = CARTESIAN_POINT ( 'NONE',  ( 80.41462361966681271, 65.06645272473066655, 3.228380831072425572 ) ) ;
#33125 = CARTESIAN_POINT ( 'NONE',  ( 84.70654116317179216, 2.970325471579660981, -2.062712134826208299 ) ) ;
#33126 = CARTESIAN_POINT ( 'NONE',  ( 2.779598305578060646, -32.89939134339510929, 7.751599049952173637 ) ) ;
#33127 = VERTEX_POINT ( 'NONE', #30475 ) ;
#33128 = CYLINDRICAL_SURFACE ( 'NONE', #20742, 3.399999999999999911 ) ;
#33129 = ORIENTED_EDGE ( 'NONE', *, *, #10557, .F. ) ;
#33130 = PLANE ( 'NONE',  #13157 ) ;
#33131 = CARTESIAN_POINT ( 'NONE',  ( 17.02371012435539299, -3.136981811050143953, -2.862043499008697811 ) ) ;
#33132 = CARTESIAN_POINT ( 'NONE',  ( 34.33178807571479751, -1.489136665238962154, -5.564703865284172934 ) ) ;
#33133 = DIRECTION ( 'NONE',  ( 1.000000000000000000, 0.000000000000000000, 0.000000000000000000 ) ) ;
#33134 = CARTESIAN_POINT ( 'NONE',  ( 22.39197674124670456, 0.3416523442181764736, -6.896521180731577161 ) ) ;
#33135 = CARTESIAN_POINT ( 'NONE',  ( -12.24874870218063627, -26.64985754041175525, 6.700000000000000178 ) ) ;
#33136 = VERTEX_POINT ( 'NONE', #30688 ) ;
#33137 = CARTESIAN_POINT ( 'NONE',  ( 2.813604351667470027, -32.87737832280624417, 7.780491323090170219 ) ) ;
#33138 = CARTESIAN_POINT ( 'NONE',  ( -1.654684078475540998, -30.12090371034253167, 7.784838882742139532 ) ) ;
#33139 = AXIS2_PLACEMENT_3D ( 'NONE', #15922, #3207, #22530 ) ;
#33140 = CARTESIAN_POINT ( 'NONE',  ( 31.83665345065898222, -2.965757740674789922, -5.175277761985421776 ) ) ;
#33141 = ORIENTED_EDGE ( 'NONE', *, *, #4450, .F. ) ;
#33142 = VERTEX_POINT ( 'NONE', #36847 ) ;
#33143 = CARTESIAN_POINT ( 'NONE',  ( 35.36852012591459982, -3.795115921518204871, 5.508735250874407186 ) ) ;
#33144 = CARTESIAN_POINT ( 'NONE',  ( -1.648565780277510218, -30.58703805132190467, 6.931070083220555844 ) ) ;
#33145 = CARTESIAN_POINT ( 'NONE',  ( 14.74516149780720475, 13.12656125137930196, -2.500000000000006217 ) ) ;
#33146 = DIRECTION ( 'NONE',  ( 0.000000000000000000, 1.000000000000000000, 0.000000000000000000 ) ) ;
#33147 = CARTESIAN_POINT ( 'NONE',  ( -1.743696608120477221, -30.19304425262081182, 7.638132480492517473 ) ) ;
#33148 = ORIENTED_EDGE ( 'NONE', *, *, #10188, .T. ) ;
#33150 = ORIENTED_EDGE ( 'NONE', *, *, #34163, .T. ) ;
#33149 = ORIENTED_EDGE ( 'NONE', *, *, #12233, .T. ) ;
#33151 = LINE ( 'NONE', #17466, #24646 ) ;
#33152 = AXIS2_PLACEMENT_3D ( 'NONE', #5453, #10994, #17574 ) ;
#33153 = VERTEX_POINT ( 'NONE', #18097 ) ;
#33154 = CARTESIAN_POINT ( 'NONE',  ( -57.41832745699786500, 33.02173582530747353, -4.020356607641593527 ) ) ;
#33155 = VERTEX_POINT ( 'NONE', #21415 ) ;
#33156 = DIRECTION ( 'NONE',  ( 0.4987820251299136531, 0.06975647374412531632, 0.8639158094271034427 ) ) ;
#33157 = ORIENTED_EDGE ( 'NONE', *, *, #6520, .F. ) ;
#33158 = CARTESIAN_POINT ( 'NONE',  ( 23.41639419491407637, 3.441844816758488967, 3.597223659465575984 ) ) ;
#33159 = CARTESIAN_POINT ( 'NONE',  ( 79.23414132050092462, 66.25012704882064440, -1.421876342974255802 ) ) ;
#33161 = EDGE_CURVE ( 'NONE', #15928, #18006, #5356, .T. ) ;
#33160 = CARTESIAN_POINT ( 'NONE',  ( -62.81463675898083210, 36.67811266762162603, -4.600311178732273021 ) ) ;
#33162 = ORIENTED_EDGE ( 'NONE', *, *, #7658, .T. ) ;
#33164 = DIRECTION ( 'NONE',  ( -0.000000000000000000, -0.000000000000000000, -1.000000000000000000 ) ) ;
#33163 = LINE ( 'NONE', #30069, #2936 ) ;
#33165 = DIRECTION ( 'NONE',  ( 0.3420201433256662704, 0.9396926207859093161, -0.000000000000000000 ) ) ;
#33166 = CARTESIAN_POINT ( 'NONE',  ( 73.64914076101801754, 62.55656703988326939, 3.294766324886514663 ) ) ;
#33167 = ORIENTED_EDGE ( 'NONE', *, *, #23470, .T. ) ;
#33168 = CARTESIAN_POINT ( 'NONE',  ( 23.64026257316363555, 2.651593249435279631, -4.149758956619620243 ) ) ;
#33169 = ORIENTED_EDGE ( 'NONE', *, *, #22150, .T. ) ;
#33170 = CARTESIAN_POINT ( 'NONE',  ( -64.08758708074093136, 37.42960919638050399, 3.182465448035748157 ) ) ;
#33171 = CARTESIAN_POINT ( 'NONE',  ( 23.06594672544511582, -8.086844732617873177, 2.500000000000001332 ) ) ;
#33172 = DIRECTION ( 'NONE',  ( 0.06925283225918045515, 0.9903616414705930238, -0.1199494240409457457 ) ) ;
#33173 = CARTESIAN_POINT ( 'NONE',  ( 4.017981887854990219, -32.06726540440380546, 7.139196562012273262 ) ) ;
#33174 = CYLINDRICAL_SURFACE ( 'NONE', #39890, 3.399999999999999911 ) ;
#33175 = CARTESIAN_POINT ( 'NONE',  ( 80.19490802141261554, 65.93291197049445884, 2.397965335136733600 ) ) ;
#33176 = CARTESIAN_POINT ( 'NONE',  ( 87.18327248044521127, 0.4293349789342923994, 4.780712506200352152 ) ) ;
#33177 = CARTESIAN_POINT ( 'NONE',  ( 32.03962978398497796, -5.076534887360421244, -0.9488177176524058565 ) ) ;
#33178 = CARTESIAN_POINT ( 'NONE',  ( 5.401390093233090717, -28.93157757802832819, 6.894806418505347700 ) ) ;
#33179 = LINE ( 'NONE', #1689, #12999 ) ;
#33180 = CIRCLE ( 'NONE', #6879, 0.1000000000000028644 ) ;
#33181 = CARTESIAN_POINT ( 'NONE',  ( -76.43695570392601724, -4.296655540762186476, -9.829794133232820030 ) ) ;
#33182 = CARTESIAN_POINT ( 'NONE',  ( -42.83131703149249603, -32.06993018339340296, 6.000000000000000000 ) ) ;
#33183 = CARTESIAN_POINT ( 'NONE',  ( 5.121324086407808451, -26.64985754041175525, 6.700000000000000178 ) ) ;
#33184 = CARTESIAN_POINT ( 'NONE',  ( 25.38653250821387175, 1.982128556287479304, -4.168580392152317238 ) ) ;
#33185 = DIRECTION ( 'NONE',  ( 0.3420201433256748746, -0.9396926207859060964, 0.000000000000000000 ) ) ;
#33186 = CARTESIAN_POINT ( 'NONE',  ( 5.185801770105404884, -29.63756468397217958, 7.784725160561911217 ) ) ;
#33187 =( BOUNDED_CURVE ( )  B_SPLINE_CURVE ( 3, ( #11502, #29651, #30061, #30469 ),
 .UNSPECIFIED., .F., .T. ) 
 B_SPLINE_CURVE_WITH_KNOTS ( ( 4, 4 ),
 ( 2.498091544796509300, 3.785093762383078708 ),
 .UNSPECIFIED. ) 
 CURVE ( )  GEOMETRIC_REPRESENTATION_ITEM ( )  RATIONAL_B_SPLINE_CURVE ( ( 1.000000000000000000, 0.8666666666666664742, 0.8666666666666664742, 1.000000000000000000 ) ) 
 REPRESENTATION_ITEM ( '' )  );
#33188 = LINE ( 'NONE', #39754, #29616 ) ;
#33189 = EDGE_CURVE ( 'NONE', #11880, #29308, #2703, .T. ) ;
#33190 = CARTESIAN_POINT ( 'NONE',  ( 4.371603794565618095, -31.82287587566080944, 7.773839561854630986 ) ) ;
#33191 = CARTESIAN_POINT ( 'NONE',  ( -18.34874870218063947, -26.64985754041175525, 6.700000000000000178 ) ) ;
#33192 = ORIENTED_EDGE ( 'NONE', *, *, #7014, .T. ) ;
#33193 = CARTESIAN_POINT ( 'NONE',  ( 37.07822424304627162, -3.092072612053704539, 5.980643640684182749 ) ) ;
#33194 = CARTESIAN_POINT ( 'NONE',  ( 67.51854282697247811, 57.96351248157043301, -3.990882853436549027 ) ) ;
#33195 = LINE ( 'NONE', #23903, #14805 ) ;
#33196 = EDGE_CURVE ( 'NONE', #7083, #16289, #3959, .T. ) ;
#33197 = AXIS2_PLACEMENT_3D ( 'NONE', #40611, #27851, #37324 ) ;
#33198 = ORIENTED_EDGE ( 'NONE', *, *, #14885, .F. ) ;
#33199 = CARTESIAN_POINT ( 'NONE',  ( -0.5530902551810904511, -32.11587329338448882, 7.778050822775636419 ) ) ;
#33200 = CARTESIAN_POINT ( 'NONE',  ( 2.474049714983522108, -26.25912200567108457, 7.013842709614101167 ) ) ;
#33201 = CARTESIAN_POINT ( 'NONE',  ( 85.31284572182654813, 1.429488415003690838, -5.464460692432248301 ) ) ;
#33202 = CARTESIAN_POINT ( 'NONE',  ( -70.92837670882107659, -27.85319909218681644, -6.138794830819693793 ) ) ;
#33203 = CARTESIAN_POINT ( 'NONE',  ( -1.474761067717296203, -28.35402923960093347, 6.887041543973313473 ) ) ;
#33204 = AXIS2_PLACEMENT_3D ( 'NONE', #21496, #3196, #14887 ) ;
#33205 = FACE_OUTER_BOUND ( 'NONE', #25228, .T. ) ;
#33206 = DIRECTION ( 'NONE',  ( 0.000000000000000000, 0.000000000000000000, 1.000000000000000000 ) ) ;
#33207 = ORIENTED_EDGE ( 'NONE', *, *, #12820, .F. ) ;
#33208 = CARTESIAN_POINT ( 'NONE',  ( 21.99446821316316303, 5.584237617783551322, 3.108634153913448994 ) ) ;
#33209 = CARTESIAN_POINT ( 'NONE',  ( 78.69038500580381879, 66.05859403932473128, -1.002944004955704349 ) ) ;
#33210 = AXIS2_PLACEMENT_3D ( 'NONE', #35645, #20174, #23662 ) ;
#33211 = CARTESIAN_POINT ( 'NONE',  ( 79.92454992231405697, 64.78853304740056274, 3.443978770203976136 ) ) ;
#33213 = ADVANCED_FACE ( 'NONE', ( #30892 ), #11709, .F. ) ;
#33212 = CARTESIAN_POINT ( 'NONE',  ( 16.75050750990541104, 0.9041099969468745501, -4.803821987783263303 ) ) ;
#33214 = ORIENTED_EDGE ( 'NONE', *, *, #2921, .F. ) ;
#33215 = CARTESIAN_POINT ( 'NONE',  ( 77.67868059383670243, 64.13990294438298179, -3.401348408886263552 ) ) ;
#33217 = CARTESIAN_POINT ( 'NONE',  ( 2.261828623665968596, -26.21660544866439224, 7.661510568013097711 ) ) ;
#33216 = CARTESIAN_POINT ( 'NONE',  ( 26.76860462860027923, 0.8092645171851360342, 4.384286172079291610 ) ) ;
#33218 = CARTESIAN_POINT ( 'NONE',  ( 81.55137728095425587, 62.42468454963441360, -2.710336141770833596 ) ) ;
#33219 = CARTESIAN_POINT ( 'NONE',  ( 77.74023705119593330, 64.68384637002905890, 3.042889847487493249 ) ) ;
#33220 = CARTESIAN_POINT ( 'NONE',  ( -29.07867591359219617, -26.64985754041175525, 6.700000000000000178 ) ) ;
#33221 = CARTESIAN_POINT ( 'NONE',  ( 82.13789946638789274, 62.20769933019770548, 1.398807481800125485 ) ) ;
#33223 = CARTESIAN_POINT ( 'NONE',  ( 39.57450465021913999, -13.08403409140692553, -6.000000000000000000 ) ) ;
#33222 = CARTESIAN_POINT ( 'NONE',  ( 87.04213330793392345, 0.5878691963682424193, 0.000000000000000000 ) ) ;
#33224 = CARTESIAN_POINT ( 'NONE',  ( 29.14988983353436680, -2.161137664473038900, -5.740130334263455758 ) ) ;
#33225 = CARTESIAN_POINT ( 'NONE',  ( 14.77044403067345257, -5.165496212256374342, -2.499999999999999556 ) ) ;
#33226 = FACE_OUTER_BOUND ( 'NONE', #14381, .T. ) ;
#33227 = VERTEX_POINT ( 'NONE', #27581 ) ;
#33228 = DIRECTION ( 'NONE',  ( -0.7660444431189818992, 0.6427876096865345890, 0.000000000000000000 ) ) ;
#33229 = CARTESIAN_POINT ( 'NONE',  ( 24.74515534416565288, 0.5823800272612684736, -4.777517428576818048 ) ) ;
#33230 = EDGE_CURVE ( 'NONE', #15453, #1114, #15222, .T. ) ;
#33231 = LINE ( 'NONE', #1342, #22865 ) ;
#33232 = CIRCLE ( 'NONE', #11507, 0.1000000000000028644 ) ;
#33233 = CARTESIAN_POINT ( 'NONE',  ( 1.078588498108656424, -33.79778590424514562, 7.754798119455333705 ) ) ;
#33234 = AXIS2_PLACEMENT_3D ( 'NONE', #3664, #34955, #16190 ) ;
#33235 = CARTESIAN_POINT ( 'NONE',  ( 5.151894269954111039, -30.15055920605938766, 7.655937882338901268 ) ) ;
#33236 = CARTESIAN_POINT ( 'NONE',  ( 35.21907562575142947, -1.051044697053814314, -5.414479983419766995 ) ) ;
#33237 = CARTESIAN_POINT ( 'NONE',  ( 30.88512837779606102, -3.430581993324693268, -4.934071252754470116 ) ) ;
#33238 = CARTESIAN_POINT ( 'NONE',  ( 3.331358690166323910, -32.66670692436608192, 6.870724624169665340 ) ) ;
#33239 = CARTESIAN_POINT ( 'NONE',  ( -65.15514661499977933, 34.97220226750606997, -6.888442104241536690 ) ) ;
#33240 = FACE_OUTER_BOUND ( 'NONE', #27433, .T. ) ;
#33241 = CARTESIAN_POINT ( 'NONE',  ( 2.815008375265338536, -32.78203729893284901, 6.892063359921933419 ) ) ;
#33242 = LINE ( 'NONE', #4437, #19106 ) ;
#33243 = VECTOR ( 'NONE', #343, 1000.000000000000000 ) ;
#33244 = CARTESIAN_POINT ( 'NONE',  ( 1.836318226000623666, -26.07255855739565575, 6.870724624169667116 ) ) ;
#33245 = ORIENTED_EDGE ( 'NONE', *, *, #10183, .T. ) ;
#33246 = ADVANCED_FACE ( 'NONE', ( #24701 ), #17893, .T. ) ;
#33247 = CARTESIAN_POINT ( 'NONE',  ( -69.61816732119611117, -47.87313727245317097, 5.855707401755813279 ) ) ;
#33249 = EDGE_CURVE ( 'NONE', #40258, #13756, #21618, .T. ) ;
#33248 = CARTESIAN_POINT ( 'NONE',  ( 66.59136238364995108, 57.77385624644436746, 3.999229419681933351 ) ) ;
#33250 = CARTESIAN_POINT ( 'NONE',  ( 72.33948634203015615, 59.36795819651598549, -3.882941974771884297 ) ) ;
#33251 = EDGE_CURVE ( 'NONE', #35439, #27554, #22634, .T. ) ;
#33252 = VERTEX_POINT ( 'NONE', #24490 ) ;
#33253 = CARTESIAN_POINT ( 'NONE',  ( 86.84125380892929513, -1.134812445414097981, 5.244953511127716794 ) ) ;
#33254 = CARTESIAN_POINT ( 'NONE',  ( 0.1710129748054547427, -26.53331930453025933, 6.903372536218457256 ) ) ;
#33255 = PRODUCT_DEFINITION_SHAPE ( 'NONE', 'NONE',  #8438 ) ;
#33256 = CARTESIAN_POINT ( 'NONE',  ( -0.8529892338943324548, -27.17613526092917198, 6.961115707816235343 ) ) ;
#33257 = CARTESIAN_POINT ( 'NONE',  ( 5.551251297819359110, -26.64985754041175525, 6.700000000000000178 ) ) ;
#33258 = PLANE ( 'NONE',  #12831 ) ;
#33259 = LINE ( 'NONE', #13708, #18163 ) ;
#33260 = CARTESIAN_POINT ( 'NONE',  ( 24.59436848130510356, -3.190661413691112447, 3.914729585663517142 ) ) ;
#33261 = AXIS2_PLACEMENT_3D ( 'NONE', #996, #23209, #19718 ) ;
#33262 = CIRCLE ( 'NONE', #20103, 4.500000000000003553 ) ;
#33263 = EDGE_CURVE ( 'NONE', #9354, #9750, #33382, .T. ) ;
#33264 = VERTEX_POINT ( 'NONE', #27372 ) ;
#33265 = CARTESIAN_POINT ( 'NONE',  ( 78.63268743221328805, 65.61080103085718918, -2.414331286641655527 ) ) ;
#33266 = CARTESIAN_POINT ( 'NONE',  ( 15.27436600411698997, 8.240067691444819431, -3.484044305282195442 ) ) ;
#33267 = CARTESIAN_POINT ( 'NONE',  ( 80.89410497084998042, 61.37834026963080447, 2.095806625473841223 ) ) ;
#33269 = ORIENTED_EDGE ( 'NONE', *, *, #11848, .F. ) ;
#33268 = DIRECTION ( 'NONE',  ( 0.1736481776669273336, 0.9848077530122085754, -0.000000000000000000 ) ) ;
#33270 = VECTOR ( 'NONE', #9299, 1000.000000000000000 ) ;
#33271 = CARTESIAN_POINT ( 'NONE',  ( 4.421194222029321885, -27.53100279559231112, 7.013842709614101167 ) ) ;
#33272 = CARTESIAN_POINT ( 'NONE',  ( 3.987918417508891089, -27.05451493134790653, 6.865312560952604670 ) ) ;
#33274 = ORIENTED_EDGE ( 'NONE', *, *, #28941, .F. ) ;
#33273 = CARTESIAN_POINT ( 'NONE',  ( 16.65948297789018895, 14.84918060193631995, 2.499999999999999556 ) ) ;
#33275 = CARTESIAN_POINT ( 'NONE',  ( 21.85643539959775339, 7.579478879252558698, 11.98046644763472024 ) ) ;
#33276 = ORIENTED_EDGE ( 'NONE', *, *, #20266, .F. ) ;
#33277 = CARTESIAN_POINT ( 'NONE',  ( -75.45330471031414277, 33.71485196875532608, -9.800414904976365804 ) ) ;
#33278 = EDGE_CURVE ( 'NONE', #11497, #23165, #4855, .T. ) ;
#33279 = CARTESIAN_POINT ( 'NONE',  ( 14.76777200802055212, -5.161570699583752919, 2.499999999979765963 ) ) ;
#33280 = CARTESIAN_POINT ( 'NONE',  ( -79.69001610741072739, 10.46859553514188867, -4.835689715862597993 ) ) ;
#33281 = DIRECTION ( 'NONE',  ( -1.000000000000000000, 0.000000000000000000, 0.000000000000000000 ) ) ;
#33282 = CARTESIAN_POINT ( 'NONE',  ( 2.480715098600875468, -26.26068663146227067, 6.903372536218457256 ) ) ;
#33283 = CARTESIAN_POINT ( 'NONE',  ( 81.16399599188275715, 62.84525499041613017, 3.248659383495554831 ) ) ;
#33284 = CARTESIAN_POINT ( 'NONE',  ( -1.532116777668663499, -30.62392227519150723, 7.761597726988851420 ) ) ;
#33285 = CYLINDRICAL_SURFACE ( 'NONE', #24638, 3.784187430299790211 ) ;
#33286 = CYLINDRICAL_SURFACE ( 'NONE', #8933, 4.500000000000003553 ) ;
#33287 = CARTESIAN_POINT ( 'NONE',  ( 0.6859961916748535948, -26.22015330552546075, 6.961115707816238007 ) ) ;
#33288 = EDGE_CURVE ( 'NONE', #16748, #38621, #10761, .T. ) ;
#33289 = AXIS2_PLACEMENT_3D ( 'NONE', #40663, #33907, #37170 ) ;
#33290 = CARTESIAN_POINT ( 'NONE',  ( 4.460641277711257402, -27.41792629019667160, 6.867199677474203234 ) ) ;
#33291 = ADVANCED_FACE ( 'NONE', ( #11300 ), #23865, .T. ) ;
#33292 = CARTESIAN_POINT ( 'NONE',  ( 1.105923466014343548, -33.01907637181788147, 7.635761828346575797 ) ) ;
#33293 = DIRECTION ( 'NONE',  ( 1.000000000000000000, 0.000000000000000000, 0.000000000000000000 ) ) ;
#33294 = EDGE_LOOP ( 'NONE', ( #27866, #40331, #8532, #26187 ) ) ;
#33295 = CARTESIAN_POINT ( 'NONE',  ( 67.35228065126028696, 58.41716755899589941, 3.985038673850037849 ) ) ;
#33296 = CARTESIAN_POINT ( 'NONE',  ( 37.01034345348816856, -2.703823390587133169, 5.982757213092503079 ) ) ;
#33297 = AXIS2_PLACEMENT_3D ( 'NONE', #19097, #5572, #27596 ) ;
#33298 = EDGE_CURVE ( 'NONE', #21194, #26672, #27169, .T. ) ;
#33299 = EDGE_LOOP ( 'NONE', ( #10628, #3859 ) ) ;
#33300 = DIRECTION ( 'NONE',  ( -0.3420201433256726542, 0.9396926207859070956, -0.000000000000000000 ) ) ;
#33301 = CARTESIAN_POINT ( 'NONE',  ( 85.21894181876761820, 2.635764410888131959, 2.550537924818469637 ) ) ;
#33303 = CARTESIAN_POINT ( 'NONE',  ( 31.21770016481918475, -0.3792164351781658338, -5.078675132288333671 ) ) ;
#33302 = CARTESIAN_POINT ( 'NONE',  ( 78.74533340381492508, 66.05753824468469304, -1.508787936435524113 ) ) ;
#33304 = CARTESIAN_POINT ( 'NONE',  ( -1.608853458698036976, -28.78960517802560304, 6.903372536218457256 ) ) ;
#33305 = EDGE_CURVE ( 'NONE', #16334, #2658, #27481, .T. ) ;
#33306 = CARTESIAN_POINT ( 'NONE',  ( 2.340695417320536986, -26.14220864269441691, 7.783750581861600182 ) ) ;
#33307 = CARTESIAN_POINT ( 'NONE',  ( -0.4954141421830357550, -26.97407892422453202, 7.635761828346577573 ) ) ;
#33308 = ORIENTED_EDGE ( 'NONE', *, *, #34584, .T. ) ;
#33309 = DIRECTION ( 'NONE',  ( -0.000000000000000000, -1.000000000000000000, -0.000000000000000000 ) ) ;
#33310 = ORIENTED_EDGE ( 'NONE', *, *, #40244, .F. ) ;
#33311 = ORIENTED_EDGE ( 'NONE', *, *, #32245, .T. ) ;
#33312 = CARTESIAN_POINT ( 'NONE',  ( 78.57229106431512378, 65.97474043420317003, -1.364493914842173306 ) ) ;
#33313 = CARTESIAN_POINT ( 'NONE',  ( -30.44874870218064089, -26.64985754041175525, 6.700000000000000178 ) ) ;
#33314 = CARTESIAN_POINT ( 'NONE',  ( 80.44862750795415707, 63.21300062201468251, 3.624000857162004152 ) ) ;
#33315 = CARTESIAN_POINT ( 'NONE',  ( 21.94773631808104497, 0.8018986738919260393, 7.249714582973164845 ) ) ;
#33317 = ORIENTED_EDGE ( 'NONE', *, *, #37374, .F. ) ;
#33316 = CARTESIAN_POINT ( 'NONE',  ( -0.8082847640681127821, -27.27503357126796857, 6.868387053540521592 ) ) ;
#33318 = CARTESIAN_POINT ( 'NONE',  ( 75.02040913282911561, 59.50525224047964201, -3.395557233589185486 ) ) ;
#33319 = CARTESIAN_POINT ( 'NONE',  ( -40.34874870218063592, -25.49307895267003587, 6.700000000000000178 ) ) ;
#33321 = LINE ( 'NONE', #20328, #39362 ) ;
#33320 = CARTESIAN_POINT ( 'NONE',  ( -56.90710715293131017, 30.56612162020725165, -3.329579881309527423 ) ) ;
#33322 = CARTESIAN_POINT ( 'NONE',  ( 5.200364047366366371, -29.55642757665872722, 7.635761828346577573 ) ) ;
#33323 = AXIS2_PLACEMENT_3D ( 'NONE', #13246, #19033, #9957 ) ;
#33324 = FACE_OUTER_BOUND ( 'NONE', #8452, .T. ) ;
#33325 = CARTESIAN_POINT ( 'NONE',  ( -41.07867591359219972, -24.55319635012989110, 6.800000000000000711 ) ) ;
#33326 = VECTOR ( 'NONE', #19505, 1000.000000000000000 ) ;
#33327 = CARTESIAN_POINT ( 'NONE',  ( 22.50262521106708746, 4.464923929019867010, -3.378628388999005860 ) ) ;
#33328 = ORIENTED_EDGE ( 'NONE', *, *, #6398, .F. ) ;
#33329 = CARTESIAN_POINT ( 'NONE',  ( 2.261116115764334022, -26.10824616355668937, 7.255881584735162981 ) ) ;
#33330 = AXIS2_PLACEMENT_3D ( 'NONE', #33389, #23494, #26581 ) ;
#33331 = EDGE_LOOP ( 'NONE', ( #13187, #15918, #19790, #24138 ) ) ;
#33332 = EDGE_CURVE ( 'NONE', #4500, #31748, #38382, .T. ) ;
#33333 = CARTESIAN_POINT ( 'NONE',  ( 22.33594428049882197, 5.124660873843202680, 5.347558210918236909 ) ) ;
#33334 = CARTESIAN_POINT ( 'NONE',  ( 2.896981936218417708, -32.75240845689362601, 7.693875151218753317 ) ) ;
#33335 = EDGE_LOOP ( 'NONE', ( #6409, #247, #12778, #10874 ) ) ;
#33336 = LINE ( 'NONE', #14764, #37973 ) ;
#33337 = VECTOR ( 'NONE', #28866, 1000.000000000000000 ) ;
#33338 = CARTESIAN_POINT ( 'NONE',  ( 81.60109106391716693, 62.17032169345860382, 2.476693319890299616 ) ) ;
#33339 = CYLINDRICAL_SURFACE ( 'NONE', #14772, 3.399999999999999911 ) ;
#33340 = ORIENTED_EDGE ( 'NONE', *, *, #5052, .T. ) ;
#33341 = CARTESIAN_POINT ( 'NONE',  ( -42.83131703149249603, -29.56993018339339940, 6.000000000000000000 ) ) ;
#33342 = EDGE_CURVE ( 'NONE', #21312, #25213, #13409, .T. ) ;
#33343 = ORIENTED_EDGE ( 'NONE', *, *, #12433, .F. ) ;
#33344 = CYLINDRICAL_SURFACE ( 'NONE', #37445, 3.399999999999999911 ) ;
#33345 = EDGE_CURVE ( 'NONE', #31581, #22494, #10058, .T. ) ;
#33346 = CARTESIAN_POINT ( 'NONE',  ( 28.88852978429638796, -3.262707939826073655, -4.666690105132320632 ) ) ;
#33347 = CARTESIAN_POINT ( 'NONE',  ( 35.86815174039828946, -2.088852906378757091, -5.804490572253821590 ) ) ;
#33348 = LINE ( 'NONE', #33748, #37152 ) ;
#33349 = CARTESIAN_POINT ( 'NONE',  ( 21.74205696664383680, 0.4458481429987432576, -8.549212226879914667 ) ) ;
#33350 = DIRECTION ( 'NONE',  ( 1.000000000000000000, 0.000000000000000000, 0.000000000000000000 ) ) ;
#33351 = ORIENTED_EDGE ( 'NONE', *, *, #407, .T. ) ;
#33352 = CARTESIAN_POINT ( 'NONE',  ( 35.33522112941847837, -3.167697025310678871, 5.721313861434861536 ) ) ;
#33353 = EDGE_CURVE ( 'NONE', #9639, #5985, #11260, .T. ) ;
#33354 = CIRCLE ( 'NONE', #9679, 0.1000000000000028644 ) ;
#33355 = ADVANCED_FACE ( 'NONE', ( #9244 ), #3321, .F. ) ;
#33356 = CARTESIAN_POINT ( 'NONE',  ( -1.149480952756954055, -27.71566481673633220, 6.887945620086120435 ) ) ;
#33357 = VERTEX_POINT ( 'NONE', #15635 ) ;
#33358 = ORIENTED_EDGE ( 'NONE', *, *, #10132, .T. ) ;
#33359 = CARTESIAN_POINT ( 'NONE',  ( 35.73193773234398662, -1.301360303042222721, 5.535510931126363054 ) ) ;
#33360 = CARTESIAN_POINT ( 'NONE',  ( -1.626205328355836199, -30.65793886950926961, 6.865482280155368322 ) ) ;
#33361 = AXIS2_PLACEMENT_3D ( 'NONE', #21348, #40268, #8563 ) ;
#33362 = CARTESIAN_POINT ( 'NONE',  ( 14.77500326541903952, -5.175625724643098557, -2.499997102511863911 ) ) ;
#33363 = VECTOR ( 'NONE', #34925, 999.9999999999998863 ) ;
#33364 = DIRECTION ( 'NONE',  ( -0.000000000000000000, -0.000000000000000000, 1.000000000000000000 ) ) ;
#33365 = AXIS2_PLACEMENT_3D ( 'NONE', #391, #12929, #9633 ) ;
#33366 = VERTEX_POINT ( 'NONE', #9 ) ;
#33367 = DIRECTION ( 'NONE',  ( 1.000000000000000000, 0.000000000000000000, -0.000000000000000000 ) ) ;
#33368 = VERTEX_POINT ( 'NONE', #12542 ) ;
#33370 = ORIENTED_EDGE ( 'NONE', *, *, #40675, .T. ) ;
#33369 = VERTEX_POINT ( 'NONE', #25113 ) ;
#33371 = CARTESIAN_POINT ( 'NONE',  ( 5.123750824668761972, -30.29724448404768111, 7.754798119455333705 ) ) ;
#33372 = CARTESIAN_POINT ( 'NONE',  ( 81.17225696364401699, 61.44517649410261129, -1.881209715725437270 ) ) ;
#33373 = ORIENTED_EDGE ( 'NONE', *, *, #17981, .T. ) ;
#33374 = CARTESIAN_POINT ( 'NONE',  ( 14.73967931769175621, -5.056389090928278485, 2.500286496908393552 ) ) ;
#33375 = VERTEX_POINT ( 'NONE', #12954 ) ;
#33377 = DIRECTION ( 'NONE',  ( 0.000000000000000000, 0.000000000000000000, 1.000000000000000000 ) ) ;
#33376 = CARTESIAN_POINT ( 'NONE',  ( 4.812762731218999335, -27.96895030771830548, 6.895394898881667345 ) ) ;
#33378 = ORIENTED_EDGE ( 'NONE', *, *, #4709, .T. ) ;
#33379 = CARTESIAN_POINT ( 'NONE',  ( 23.19659671777491283, 3.528833225524024897, 3.648563265218450091 ) ) ;
#33380 = CARTESIAN_POINT ( 'NONE',  ( 82.15586074033932107, 62.44414535927726462, -1.848245342697680593 ) ) ;
#33381 = LINE ( 'NONE', #39314, #16295 ) ;
#33382 = LINE ( 'NONE', #33580, #32499 ) ;
#33383 = VERTEX_POINT ( 'NONE', #22030 ) ;
#33385 = CARTESIAN_POINT ( 'NONE',  ( 17.95405594424124018, -2.878999424384995898, -3.008562669219466024 ) ) ;
#33384 = CARTESIAN_POINT ( 'NONE',  ( -0.004313233346292664333, -26.62815260315269228, 7.763628509615283946 ) ) ;
#33386 = LINE ( 'NONE', #18307, #31691 ) ;
#33387 = CARTESIAN_POINT ( 'NONE',  ( 74.17630236427460488, 61.40657735673663353, 3.883841728571264973 ) ) ;
#33388 = CARTESIAN_POINT ( 'NONE',  ( 24.07252604127487672, 2.729050162928195356, -3.962914714437188124 ) ) ;
#33389 = CARTESIAN_POINT ( 'NONE',  ( 1.700390093233090871, -29.56993018339339940, 7.800000000000000711 ) ) ;
#33390 = PLANE ( 'NONE',  #33521 ) ;
#33391 = CARTESIAN_POINT ( 'NONE',  ( 4.173564143869515242, -31.91328782742822767, 7.386948897581451234 ) ) ;
#33392 = CARTESIAN_POINT ( 'NONE',  ( 6.136079629878683050, -27.96984039756584295, 7.635761828346577573 ) ) ;
#33393 = CARTESIAN_POINT ( 'NONE',  ( 81.52783586777056257, 64.51439989829020760, 2.952528780688829624 ) ) ;
#33394 = CARTESIAN_POINT ( 'NONE',  ( 85.24855023725586989, 2.602506829941634514, 1.762177041774413588 ) ) ;
#33395 = CARTESIAN_POINT ( 'NONE',  ( 33.19459970134796123, -3.309813850278316760, -5.543304389637502716 ) ) ;
#33396 = PRODUCT_DEFINITION_FORMATION_WITH_SPECIFIED_SOURCE ( 'ANY', '', #22464, .NOT_KNOWN. ) ;
#33397 = VECTOR ( 'NONE', #534, 1000.000000000000000 ) ;
#33398 = VECTOR ( 'NONE', #16028, 1000.000000000000000 ) ;
#33399 = CARTESIAN_POINT ( 'NONE',  ( -72.84815947045237294, 2.027470820963650056, -10.96147798754374669 ) ) ;
#33400 = VERTEX_POINT ( 'NONE', #34607 ) ;
#33401 = CARTESIAN_POINT ( 'NONE',  ( 19.71787932340214411, -3.013412653616829751, 3.231043527512243330 ) ) ;
#33402 = CARTESIAN_POINT ( 'NONE',  ( -38.87867591359218977, -24.55319635012989110, 6.800000000000000711 ) ) ;
#33403 = CARTESIAN_POINT ( 'NONE',  ( 36.14926277598984683, -3.245532955201251291, -5.848364748053938023 ) ) ;
#33404 = LINE ( 'NONE', #5177, #24666 ) ;
#33405 = CARTESIAN_POINT ( 'NONE',  ( 5.187261144941242463, -29.64526969736682815, 7.782861076432734393 ) ) ;
#33406 = DIRECTION ( 'NONE',  ( 1.000000000000000000, 0.000000000000000000, 0.000000000000000000 ) ) ;
#33407 = DIRECTION ( 'NONE',  ( -0.000000000000000000, -0.000000000000000000, 1.000000000000000000 ) ) ;
#33408 = EDGE_CURVE ( 'NONE', #10861, #24982, #6384, .T. ) ;
#33409 = CARTESIAN_POINT ( 'NONE',  ( 0.1214003938371286395, -25.12656084334626172, 7.695279973900954751 ) ) ;
#33410 = EDGE_CURVE ( 'NONE', #33969, #39661, #28397, .T. ) ;
#33411 = ORIENTED_EDGE ( 'NONE', *, *, #27200, .F. ) ;
#33412 = CARTESIAN_POINT ( 'NONE',  ( 20.88448788323691119, 4.552395270423596152, 2.802001917821514532 ) ) ;
#33413 = CARTESIAN_POINT ( 'NONE',  ( -64.08758708074093136, 38.13199975834722721, -3.043809435734133650 ) ) ;
#33414 = CARTESIAN_POINT ( 'NONE',  ( 66.72933079118084265, 57.85140187965895819, -3.999416444359401357 ) ) ;
#33415 = B_SPLINE_CURVE_WITH_KNOTS ( 'NONE', 3,
 ( #13926, #14522, #36366, #26498, #1395, #17603, #11223, #20298, #29981, #10826, #33290, #7750, #26302, #23991, #4670, #8135, #38834, #36562, #1589, #1795, #8342, #5074, #35774, #10629, #30182, #39028, #39433, #20918, #32882, #23206, #7548 ),
 .UNSPECIFIED., .F., .F.,
 ( 4, 3, 3, 3, 3, 3, 3, 3, 3, 3, 4 ),
 ( 0.000000000000000000, 3.077658087705820324E-05, 6.152638666999296060E-05, 9.267501192706854797E-05, 0.0001241882240135193068, 0.0001556618703051694563, 0.0001866161554452238757, 0.0002167966385860975508, 0.0002463805737537784653, 0.0002758761370306542790, 0.0002847094172289964297 ),
 .UNSPECIFIED. ) ;
#33416 = PLANE ( 'NONE',  #6278 ) ;
#33417 = VECTOR ( 'NONE', #11667, 1000.000000000000000 ) ;
#33418 = ORIENTED_EDGE ( 'NONE', *, *, #9827, .F. ) ;
#33419 = CARTESIAN_POINT ( 'NONE',  ( -0.5385815272626705008, -32.12866175765496024, 7.784476445165074310 ) ) ;
#33420 = CARTESIAN_POINT ( 'NONE',  ( 3.895694199539312841, -32.16621117463044044, 7.756377446753167426 ) ) ;
#33421 = CARTESIAN_POINT ( 'NONE',  ( 84.97662400644560421, 1.905623477933771737, -4.853294916085792998 ) ) ;
#33422 = CARTESIAN_POINT ( 'NONE',  ( -76.23695949607322575, 10.51077996663807035, 8.482526175063888729 ) ) ;
#33423 = DIRECTION ( 'NONE',  ( 0.000000000000000000, 1.000000000000000000, 0.000000000000000000 ) ) ;
#33424 = CIRCLE ( 'NONE', #38647, 2.000000000000000000 ) ;
#33425 = CARTESIAN_POINT ( 'NONE',  ( -1.699609906766908596, -29.56993018339339940, 7.767301406074262893 ) ) ;
#33426 = ORIENTED_EDGE ( 'NONE', *, *, #12329, .F. ) ;
#33427 = CARTESIAN_POINT ( 'NONE',  ( 24.05810555315960642, 3.342710263256114089, 3.230529690456637404 ) ) ;
#33428 = CARTESIAN_POINT ( 'NONE',  ( 82.41652906543019697, 64.58603266165640377, -1.328060019258380242 ) ) ;
#33429 = CARTESIAN_POINT ( 'NONE',  ( 79.07783777134646641, 65.79916784333097723, 2.450942308261427893 ) ) ;
#33430 = PLANE ( 'NONE',  #35765 ) ;
#33431 = ORIENTED_EDGE ( 'NONE', *, *, #17403, .T. ) ;
#33432 = CARTESIAN_POINT ( 'NONE',  ( 79.63092111360349179, 60.86998874196336828, -2.418543376929292332 ) ) ;
#33434 = CYLINDRICAL_SURFACE ( 'NONE', #28270, 0.1000000000000028644 ) ;
#33433 = CARTESIAN_POINT ( 'NONE',  ( 21.77774817454276146, 0.1996980602981901221, 8.433676550975363284 ) ) ;
#33435 = CARTESIAN_POINT ( 'NONE',  ( 80.61314501155287360, 64.81116531652870094, -3.343039074468324046 ) ) ;
#33436 = CARTESIAN_POINT ( 'NONE',  ( 79.26553226962346343, 61.67928659302138783, 3.361664161258347772 ) ) ;
#33437 = ORIENTED_EDGE ( 'NONE', *, *, #6663, .T. ) ;
#33438 = ORIENTED_EDGE ( 'NONE', *, *, #20574, .F. ) ;
#33439 = CARTESIAN_POINT ( 'NONE',  ( -0.8286472691028512472, -27.29749316118379454, 7.761597726988854973 ) ) ;
#33440 = CARTESIAN_POINT ( 'NONE',  ( 79.63539728012720786, 66.30663591242944221, 1.358135763685230923 ) ) ;
#33441 =( BOUNDED_CURVE ( )  B_SPLINE_CURVE ( 3, ( #3765, #32171, #13004, #38112 ),
 .UNSPECIFIED., .F., .T. ) 
 B_SPLINE_CURVE_WITH_KNOTS ( ( 4, 4 ),
 ( 4.748221474220559735, 4.941946782021394036 ),
 .UNSPECIFIED. ) 
 CURVE ( )  GEOMETRIC_REPRESENTATION_ITEM ( )  RATIONAL_B_SPLINE_CURVE ( ( 1.000000000000000000, 0.9968749865767494445, 0.9968749865767494445, 1.000000000000000000 ) ) 
 REPRESENTATION_ITEM ( '' )  );
#33443 = DIRECTION ( 'NONE',  ( -0.000000000000000000, -1.000000000000000000, -0.000000000000000000 ) ) ;
#33442 = CARTESIAN_POINT ( 'NONE',  ( 4.345741007283959512, -31.86168028790528695, 6.875671892026063325 ) ) ;
#33444 = VECTOR ( 'NONE', #10967, 1000.000000000000000 ) ;
#33445 = CARTESIAN_POINT ( 'NONE',  ( 26.56136967304951213, 3.021295450130037530, 0.006841891102512360698 ) ) ;
#33446 = DIRECTION ( 'NONE',  ( 0.000000000000000000, 1.000000000000000000, 0.000000000000000000 ) ) ;
#33447 = PLANE ( 'NONE',  #35824 ) ;
#33448 = VERTEX_POINT ( 'NONE', #22244 ) ;
#33449 = DIRECTION ( 'NONE',  ( -1.000000000000000000, 0.000000000000000000, 0.000000000000000000 ) ) ;
#33450 = CARTESIAN_POINT ( 'NONE',  ( 21.97292779079860026, 0.2231725819405185052, -7.728249543608548322 ) ) ;
#33451 = EDGE_CURVE ( 'NONE', #15988, #2006, #3509, .T. ) ;
#33452 = FACE_OUTER_BOUND ( 'NONE', #18866, .T. ) ;
#33453 = CARTESIAN_POINT ( 'NONE',  ( -1.699609906766908818, -29.56993018339339940, 7.620413589471895399 ) ) ;
#33454 = CARTESIAN_POINT ( 'NONE',  ( 5.154949517232994438, -29.00770241687787276, 6.880608371227950215 ) ) ;
#33455 = CARTESIAN_POINT ( 'NONE',  ( 3.751251297819363728, -26.64985754041175525, 6.800000000000000711 ) ) ;
#33456 = CARTESIAN_POINT ( 'NONE',  ( 35.36775907828450016, -3.789722492740957183, -5.512854138522889968 ) ) ;
#33457 = CARTESIAN_POINT ( 'NONE',  ( 3.369652234211440334, -26.60790990542409773, 7.680992449362126884 ) ) ;
#33458 = CARTESIAN_POINT ( 'NONE',  ( 1.145429890469515932, -32.92433313672930240, 7.695279973900954751 ) ) ;
#33459 = LINE ( 'NONE', #34278, #305 ) ;
#33460 = CARTESIAN_POINT ( 'NONE',  ( -24.24874870218063450, -26.64985754041175525, 6.700000000000000178 ) ) ;
#33461 = FACE_OUTER_BOUND ( 'NONE', #35406, .T. ) ;
#33462 = CIRCLE ( 'NONE', #29499, 2.500000000000002220 ) ;
#33463 = CARTESIAN_POINT ( 'NONE',  ( 14.75718030968480932, -4.580811787944012003, -2.509406477144433545 ) ) ;
#33464 = EDGE_CURVE ( 'NONE', #12271, #28306, #39273, .T. ) ;
#33465 = APPLICATION_CONTEXT ( 'automotive_design' ) ;
#33466 = ORIENTED_EDGE ( 'NONE', *, *, #3117, .F. ) ;
#33467 = CARTESIAN_POINT ( 'NONE',  ( 66.27376694608996388, 57.73522568913447373, 4.000000000000000000 ) ) ;
#33468 = CARTESIAN_POINT ( 'NONE',  ( 72.96153509227066536, 61.08495594734687018, -3.864208391313482149 ) ) ;
#33469 = VERTEX_POINT ( 'NONE', #17030 ) ;
#33470 = CARTESIAN_POINT ( 'NONE',  ( 87.51701825761838904, -2.015745416966476800, -3.511549023785576651 ) ) ;
#33471 = CIRCLE ( 'NONE', #16332, 3.000000000000002665 ) ;
#33472 = DIRECTION ( 'NONE',  ( 1.000000000000000000, 0.000000000000000000, 0.000000000000000000 ) ) ;
#33473 = CARTESIAN_POINT ( 'NONE',  ( 3.038230656040339372, -26.44419577647722264, 6.895222827070024429 ) ) ;
#33474 = CARTESIAN_POINT ( 'NONE',  ( -0.8638866058868895914, -27.18780260212992061, 6.903112506833886997 ) ) ;
#33475 = DIRECTION ( 'NONE',  ( 0.3420201433256662704, 0.9396926207859093161, -0.000000000000000000 ) ) ;
#33476 = ORIENTED_EDGE ( 'NONE', *, *, #31706, .T. ) ;
#33477 = DIRECTION ( 'NONE',  ( 1.000000000000000000, 0.000000000000000000, 0.000000000000000000 ) ) ;
#33478 = ORIENTED_EDGE ( 'NONE', *, *, #29022, .F. ) ;
#33479 = CARTESIAN_POINT ( 'NONE',  ( 80.34542504610527658, 62.25824679691979924, -3.331801170923413213 ) ) ;
#33480 = CARTESIAN_POINT ( 'NONE',  ( 22.53035224700295913, 7.500703693485321288, -2.500000000000001776 ) ) ;
#33481 = CARTESIAN_POINT ( 'NONE',  ( 81.83449460947085186, 63.17368474096252129, -2.819252638153957768 ) ) ;
#33482 = EDGE_CURVE ( 'NONE', #18814, #22060, #28946, .T. ) ;
#33483 = CARTESIAN_POINT ( 'NONE',  ( 80.37564778476929916, 62.54931541869399325, 3.458772244351172809 ) ) ;
#33484 = CYLINDRICAL_SURFACE ( 'NONE', #10699, 0.09010775117052870209 ) ;
#33485 = CARTESIAN_POINT ( 'NONE',  ( 0.9179867665364390694, -32.98135877481576728, 7.002103980607166989 ) ) ;
#33487 = EDGE_LOOP ( 'NONE', ( #7695, #18136, #1545, #34851 ) ) ;
#33486 = CARTESIAN_POINT ( 'NONE',  ( 19.16552509909860902, 12.52704827632410556, 2.500000000000000444 ) ) ;
#33488 = ADVANCED_FACE ( 'NONE', ( #19546 ), #19933, .F. ) ;
#33489 = CARTESIAN_POINT ( 'NONE',  ( 21.85643539959779957, -12.42149291456256499, -5.642648835571736576 ) ) ;
#33490 = ORIENTED_EDGE ( 'NONE', *, *, #4301, .T. ) ;
#33491 = CARTESIAN_POINT ( 'NONE',  ( -78.35305259910721531, 10.09532361400513523, 8.407576680341714237 ) ) ;
#33492 = ADVANCED_FACE ( 'NONE', ( #38456 ), #39263, .T. ) ;
#33493 = CARTESIAN_POINT ( 'NONE',  ( 14.71719540082058764, -5.067275742575013453, 2.500000000000000444 ) ) ;
#33494 = CARTESIAN_POINT ( 'NONE',  ( -74.22183281877552474, 6.953451750990062408, -9.495966342939334837 ) ) ;
#33495 = VECTOR ( 'NONE', #23817, 1000.000000000000000 ) ;
#33496 = CYLINDRICAL_SURFACE ( 'NONE', #20160, 0.09010775117052914618 ) ;
#33497 = CARTESIAN_POINT ( 'NONE',  ( -36.34874870218064302, -25.49307895267003587, 6.700000000000000178 ) ) ;
#33498 = CARTESIAN_POINT ( 'NONE',  ( 4.907274956385933251, -30.69948305815673351, 7.680992449362120666 ) ) ;
#33499 = CARTESIAN_POINT ( 'NONE',  ( 3.960809538620813974, -27.03012904829729024, 7.774064877406531515 ) ) ;
#33500 = CARTESIAN_POINT ( 'NONE',  ( -34.87867591359218977, -26.64985754041175525, 6.700000000000000178 ) ) ;
#33501 = DIRECTION ( 'NONE',  ( 0.000000000000000000, 0.000000000000000000, 1.000000000000000000 ) ) ;
#33502 = CARTESIAN_POINT ( 'NONE',  ( -17.27251170661583402, 3.729367930467589076, 6.000000000000000000 ) ) ;
#33503 = FACE_OUTER_BOUND ( 'NONE', #29452, .T. ) ;
#33504 = CARTESIAN_POINT ( 'NONE',  ( 4.263026732192791712, -31.80442242921652252, 6.880147297696977304 ) ) ;
#33505 = ADVANCED_FACE ( 'NONE', ( #26130 ), #38660, .T. ) ;
#33506 = VERTEX_POINT ( 'NONE', #32511 ) ;
#33507 = CARTESIAN_POINT ( 'NONE',  ( 68.16305384742138074, 58.02271910793402299, 3.969942683317755350 ) ) ;
#33508 = CARTESIAN_POINT ( 'NONE',  ( 35.78619758286966857, -3.165684574248104344, 5.791699643902712857 ) ) ;
#33509 = AXIS2_PLACEMENT_3D ( 'NONE', #21891, #34469, #12613 ) ;
#33510 = ORIENTED_EDGE ( 'NONE', *, *, #32614, .T. ) ;
#33511 = CARTESIAN_POINT ( 'NONE',  ( 0.5248424762351729944, -26.37961863118246697, 7.635761828346577573 ) ) ;
#33512 = CARTESIAN_POINT ( 'NONE',  ( 88.92600529607371129, -1.724176122391732680, 0.2146816905789898644 ) ) ;
#33514 = CARTESIAN_POINT ( 'NONE',  ( 2.106121278015897325, -33.05321266051473117, 7.387053503561885393 ) ) ;
#33513 = CARTESIAN_POINT ( 'NONE',  ( -0.2903816339205422259, -32.33492270865357199, 7.505001789837626447 ) ) ;
#33515 = CYLINDRICAL_SURFACE ( 'NONE', #20196, 0.1000000000000028644 ) ;
#33516 = DIRECTION ( 'NONE',  ( -0.000000000000000000, -0.000000000000000000, 1.000000000000000000 ) ) ;
#33517 = CARTESIAN_POINT ( 'NONE',  ( 0.04278369059588756074, -26.60137143983851615, 6.894806418505345924 ) ) ;
#33518 = EDGE_CURVE ( 'NONE', #23544, #28626, #3602, .T. ) ;
#33519 = ORIENTED_EDGE ( 'NONE', *, *, #32111, .T. ) ;
#33520 = DIRECTION ( 'NONE',  ( 0.000000000000000000, 0.000000000000000000, -1.000000000000000000 ) ) ;
#33521 = AXIS2_PLACEMENT_3D ( 'NONE', #29867, #30699, #5365 ) ;
#33522 = ORIENTED_EDGE ( 'NONE', *, *, #27696, .T. ) ;
#33523 = CARTESIAN_POINT ( 'NONE',  ( 80.69037048981478222, 62.35571368504050582, -3.252077313700841188 ) ) ;
#33524 = CARTESIAN_POINT ( 'NONE',  ( -1.545690014252844247, -28.26108608583131954, 6.865706122441729065 ) ) ;
#33525 = CARTESIAN_POINT ( 'NONE',  ( 78.81125837042770854, 65.77339625846090598, 2.277920705665355872 ) ) ;
#33526 = CARTESIAN_POINT ( 'NONE',  ( 21.73992701349164491, 0.3979915806805984779, 8.655561263121205329 ) ) ;
#33528 = EDGE_LOOP ( 'NONE', ( #6754, #26878, #41, #34639 ) ) ;
#33527 = CARTESIAN_POINT ( 'NONE',  ( 4.728949138686682652, -27.82203914373970832, 7.767720160662275219 ) ) ;
#33529 = CARTESIAN_POINT ( 'NONE',  ( 74.68367562674023930, 60.27297886100710400, -3.815996826674382447 ) ) ;
#33530 = CARTESIAN_POINT ( 'NONE',  ( 3.309654742251315618, -32.56498916126437138, 6.864651958020304257 ) ) ;
#33532 = CARTESIAN_POINT ( 'NONE',  ( -1.102808333278741504, -27.46281054005859446, 7.139344958878411695 ) ) ;
#33531 = CARTESIAN_POINT ( 'NONE',  ( 0.000000000000000000, 0.5999999999999995337, -3.730072921939604047 ) ) ;
#33533 = DIRECTION ( 'NONE',  ( -0.000000000000000000, -0.000000000000000000, 1.000000000000000000 ) ) ;
#33534 = EDGE_CURVE ( 'NONE', #826, #6003, #21159, .T. ) ;
#33535 = EDGE_CURVE ( 'NONE', #6329, #21217, #34880, .T. ) ;
#33536 = CARTESIAN_POINT ( 'NONE',  ( 21.75127074489211410, 5.956360602679930949, -3.331638318609325911 ) ) ;
#33537 = ORIENTED_EDGE ( 'NONE', *, *, #5109, .T. ) ;
#33538 = ADVANCED_FACE ( 'NONE', ( #33109 ), #4892, .F. ) ;
#33539 = AXIS2_PLACEMENT_3D ( 'NONE', #24882, #21383, #9415 ) ;
#33540 = CARTESIAN_POINT ( 'NONE',  ( 22.31758782591801094, 6.227955964823622459, -0.6941013191108784675 ) ) ;
#33541 = DIRECTION ( 'NONE',  ( -1.000000000000000000, 0.000000000000000000, 0.000000000000000000 ) ) ;
#33542 = LINE ( 'NONE', #23636, #1158 ) ;
#33543 = CARTESIAN_POINT ( 'NONE',  ( 80.90131254178920983, 64.57540998625900386, 3.341858160559718183 ) ) ;
#33544 = CARTESIAN_POINT ( 'NONE',  ( 88.77375424906220758, -2.037038645060464503, 1.247452244799444276 ) ) ;
#33545 = DIRECTION ( 'NONE',  ( 0.8660254037844393737, 0.000000000000000000, 0.4999999999999985567 ) ) ;
#33546 = VERTEX_POINT ( 'NONE', #24439 ) ;
#33547 = CARTESIAN_POINT ( 'NONE',  ( 0.1825688514436868137, -0.5999999999999994227, -3.931742364907163001 ) ) ;
#33548 = DIRECTION ( 'NONE',  ( 0.000000000000000000, 0.000000000000000000, -1.000000000000000000 ) ) ;
#33549 = CIRCLE ( 'NONE', #8534, 0.1000000000000028644 ) ;
#33550 = CARTESIAN_POINT ( 'NONE',  ( 14.78586781214834822, -4.455391028847350832, -2.513676416125953939 ) ) ;
#33551 = CARTESIAN_POINT ( 'NONE',  ( -67.16566696070617581, 37.18524951245925081, -8.491446490664150915 ) ) ;
#33552 = DIRECTION ( 'NONE',  ( 0.000000000000000000, 0.000000000000000000, 1.000000000000000000 ) ) ;
#33553 = CARTESIAN_POINT ( 'NONE',  ( 26.61193938308475992, 1.046481346643641341, -4.377103786515438522 ) ) ;
#33554 = CARTESIAN_POINT ( 'NONE',  ( 1.909697446979260471, -26.17637777632732821, 6.939395833800439561 ) ) ;
#33555 = VERTEX_POINT ( 'NONE', #21364 ) ;
#33556 = CARTESIAN_POINT ( 'NONE',  ( 34.92821691692935104, -1.713421868941626958, 5.657791010641918916 ) ) ;
#33557 = CARTESIAN_POINT ( 'NONE',  ( 87.36631219772915813, 0.2237360808920199895, 4.554730944530843040 ) ) ;
#33558 = VERTEX_POINT ( 'NONE', #18254 ) ;
#33559 = ORIENTED_EDGE ( 'NONE', *, *, #9339, .T. ) ;
#33561 = CARTESIAN_POINT ( 'NONE',  ( 34.63773063272169850, -0.7807602160518050116, 5.273885112211214476 ) ) ;
#33560 = CARTESIAN_POINT ( 'NONE',  ( 81.23287006775859709, 61.35999619221078660, -1.467306180864046183 ) ) ;
#33562 = CARTESIAN_POINT ( 'NONE',  ( 14.75437388269761385, -4.625874150431743104, -2.499999999999999556 ) ) ;
#33563 = CARTESIAN_POINT ( 'NONE',  ( 14.77315594796471387, 13.19392823276521298, -2.499999999999998668 ) ) ;
#33564 = ORIENTED_EDGE ( 'NONE', *, *, #15201, .T. ) ;
#33565 = DIRECTION ( 'NONE',  ( -0.000000000000000000, -0.000000000000000000, -1.000000000000000000 ) ) ;
#33566 = ORIENTED_EDGE ( 'NONE', *, *, #40605, .T. ) ;
#33567 = EDGE_LOOP ( 'NONE', ( #3454, #12391, #3647, #21835 ) ) ;
#33568 = CARTESIAN_POINT ( 'NONE',  ( -34.24874870218063450, -26.64985754041175525, 6.800000000000000711 ) ) ;
#33569 = CARTESIAN_POINT ( 'NONE',  ( 78.82816376705464734, 65.99584493362826265, -1.862141363775770220 ) ) ;
#33570 = CARTESIAN_POINT ( 'NONE',  ( -58.91620474891573167, 27.52990360452328389, -4.138963871842760156 ) ) ;
#33571 = ORIENTED_EDGE ( 'NONE', *, *, #13773, .T. ) ;
#33573 = DIRECTION ( 'NONE',  ( 0.000000000000000000, 0.000000000000000000, 1.000000000000000000 ) ) ;
#33572 = PRESENTATION_STYLE_ASSIGNMENT (( #20994 ) ) ;
#33574 = ORIENTED_EDGE ( 'NONE', *, *, #11187, .T. ) ;
#33575 = EDGE_CURVE ( 'NONE', #8273, #33127, #19357, .T. ) ;
#33576 = CARTESIAN_POINT ( 'NONE',  ( 24.34634393679970898, 2.915314615346324967, 3.758318930332451124 ) ) ;
#33577 = CARTESIAN_POINT ( 'NONE',  ( 81.69611827519042890, 64.99316753419185488, -2.512558077908312537 ) ) ;
#33578 = EDGE_CURVE ( 'NONE', #9702, #38572, #2934, .T. ) ;
#33579 = AXIS2_PLACEMENT_3D ( 'NONE', #29039, #29442, #1255 ) ;
#33580 = CARTESIAN_POINT ( 'NONE',  ( 3.551251297819357777, -26.64985754041175525, 6.700000000000000178 ) ) ;
#33582 = CARTESIAN_POINT ( 'NONE',  ( 1.074705601983324099, -26.22799677331331125, 7.691066658568948000 ) ) ;
#33581 = CARTESIAN_POINT ( 'NONE',  ( 0.07872181157995387923, -26.58158750152437477, 7.778050822775634643 ) ) ;
#33583 = CARTESIAN_POINT ( 'NONE',  ( -1.795493615143840982, -29.40023310768274456, 6.895394898881668233 ) ) ;
#33584 = CARTESIAN_POINT ( 'NONE',  ( 74.27115401224453706, 62.67359094190466351, 3.404024988867591084 ) ) ;
#33585 = ORIENTED_EDGE ( 'NONE', *, *, #40629, .F. ) ;
#33586 = CARTESIAN_POINT ( 'NONE',  ( 22.24257640610459674, 3.226614291024176406, -4.542278202119804043 ) ) ;
#33587 = ORIENTED_EDGE ( 'NONE', *, *, #26107, .F. ) ;
#33588 = ADVANCED_FACE ( 'NONE', ( #36391 ), #20946, .F. ) ;
#33589 = CARTESIAN_POINT ( 'NONE',  ( -0.3926246584570329823, -26.75618466204053192, 7.387053503561885393 ) ) ;
#33590 = LINE ( 'NONE', #30078, #10480 ) ;
#33591 = ORIENTED_EDGE ( 'NONE', *, *, #39262, .T. ) ;
#33592 = CARTESIAN_POINT ( 'NONE',  ( -16.24874870218063450, -26.64985754041175525, 6.700000000000000178 ) ) ;
#33593 = CARTESIAN_POINT ( 'NONE',  ( 81.83803008603292994, 64.28563725689731712, 2.776691787112188337 ) ) ;
#33594 = B_SPLINE_CURVE_WITH_KNOTS ( 'NONE', 3,
 ( #25338, #37872, #3532, #16056, #38680, #10675, #29822, #20544, #7397, #26147, #29626, #32529, #32731, #4909, #26937, #4330, #16850, #23256, #1440, #26541, #25135, #3538, #7005, #16651, #22863, #436, #646, #19763, #25545, #38483, #25746, #34834, #38286, #6809, #28632, #10085 ),
 .UNSPECIFIED., .F., .F.,
 ( 4, 2, 2, 2, 2, 2, 2, 2, 2, 2, 2, 2, 2, 2, 2, 2, 2, 4 ),
 ( 0.03938660120963451833, 0.04068090286293612329, 0.04197520451623773519, 0.04326950616953934015, 0.04456380782284094511, 0.04585810947614255700, 0.04715241112944416196, 0.04844671278274577386, 0.04974101443604737882, 0.05103531608934898378, 0.05232961774265058874, 0.05362391939595220064, 0.05491822104925381254, 0.05621252270255541750, 0.05750682435585702246, 0.05880112600915864129, 0.05944827683580943684, 0.06009542766246023932 ),
 .UNSPECIFIED. ) ;
#33595 = CARTESIAN_POINT ( 'NONE',  ( 85.06303677129686491, 2.810884359907178442, 0.2996589496366894867 ) ) ;
#33596 = FACE_OUTER_BOUND ( 'NONE', #25674, .T. ) ;
#33597 = CIRCLE ( 'NONE', #39460, 0.1000000000000028644 ) ;
#33598 = CARTESIAN_POINT ( 'NONE',  ( 2.836962395230103073, -32.88026010553018352, 6.870737987065012042 ) ) ;
#33599 = FACE_OUTER_BOUND ( 'NONE', #27617, .T. ) ;
#33600 = CARTESIAN_POINT ( 'NONE',  ( 0.02383944398482668731, -26.49760566920138061, 6.865554069792296765 ) ) ;
#33601 = CARTESIAN_POINT ( 'NONE',  ( 37.02724721148364040, -2.689435811069947224, -5.985395453346618488 ) ) ;
#33602 = CARTESIAN_POINT ( 'NONE',  ( 5.514668135701366936, -33.12250938555327906, 6.894806418505347700 ) ) ;
#33603 = CARTESIAN_POINT ( 'NONE',  ( 4.643350526641022213, -31.46439155470594073, 7.013842709614101167 ) ) ;
#33604 = CARTESIAN_POINT ( 'NONE',  ( -28.44874870218064444, -25.49307895267003587, 6.800000000000000711 ) ) ;
#33605 =( BOUNDED_SURFACE ( )  B_SPLINE_SURFACE ( 3, 3, ( 
 ( #30334, #33020, #36504, #5416 ),
 ( #29914, #5009, #36702, #14263 ),
 ( #17954, #23932, #4614, #17540 ),
 ( #7889, #30539, #8485, #39580 ),
 ( #11365, #23734, #39373, #29716 ),
 ( #17749, #33223, #30128, #17144 ),
 ( #33641, #1943, #11164, #14659 ) ),
 .UNSPECIFIED., .T., .F., .T. ) 
 B_SPLINE_SURFACE_WITH_KNOTS ( ( 4, 3, 4 ),
 ( 4, 4 ),
 ( 0.000000000000000000, 0.5000000000000000000, 1.000000000000000000 ),
 ( 0.000000000000000000, 1.000000000000000000 ),
 .UNSPECIFIED. ) 
 GEOMETRIC_REPRESENTATION_ITEM ( )  RATIONAL_B_SPLINE_SURFACE ( (
 ( 1.000000000000000000, 0.9563893749471424899, 0.9563893749471424899, 1.000000000000000000),
 ( 0.3333333333333333703, 0.3187964583157141818, 0.3187964583157141818, 0.3333333333333333703),
 ( 0.3333333333333333703, 0.3187964583157141818, 0.3187964583157141818, 0.3333333333333333703),
 ( 1.000000000000000000, 0.9563893749471424899, 0.9563893749471424899, 1.000000000000000000),
 ( 0.3333333333333333703, 0.3187964583157141818, 0.3187964583157141818, 0.3333333333333333703),
 ( 0.3333333333333333703, 0.3187964583157141818, 0.3187964583157141818, 0.3333333333333333703),
 ( 1.000000000000000000, 0.9563893749471424899, 0.9563893749471424899, 1.000000000000000000) ) ) 
 REPRESENTATION_ITEM ( '' )  SURFACE ( )  );
#33606 = LINE ( 'NONE', #8858, #34822 ) ;
#33607 = CARTESIAN_POINT ( 'NONE',  ( 3.301837905240542881, -32.68206207414233688, 7.013842709614101167 ) ) ;
#33608 = VECTOR ( 'NONE', #39589, 1000.000000000000000 ) ;
#33609 = EDGE_LOOP ( 'NONE', ( #14067, #28171, #30899, #37032 ) ) ;
#33610 = CARTESIAN_POINT ( 'NONE',  ( 34.79207415533190328, -3.831289137303656389, 5.380522550652695024 ) ) ;
#33611 = CARTESIAN_POINT ( 'NONE',  ( -71.90801809991052096, -0.5528860982213333886, 3.919500413570160990 ) ) ;
#33612 = CARTESIAN_POINT ( 'NONE',  ( 67.04731915158012612, 57.88926793091046363, -3.996990690923978296 ) ) ;
#33613 = FACE_OUTER_BOUND ( 'NONE', #19071, .T. ) ;
#33614 = VERTEX_POINT ( 'NONE', #30214 ) ;
#33615 = CARTESIAN_POINT ( 'NONE',  ( -0.5461542787101242302, -32.12201250624161730, 7.782034975670479859 ) ) ;
#33616 = FACE_OUTER_BOUND ( 'NONE', #4790, .T. ) ;
#33617 = CARTESIAN_POINT ( 'NONE',  ( 67.64868974113205979, 58.60604628695281804, 3.975234571633589731 ) ) ;
#33618 = DIRECTION ( 'NONE',  ( -0.000000000000000000, -0.000000000000000000, 1.000000000000000000 ) ) ;
#33619 = ORIENTED_EDGE ( 'NONE', *, *, #2622, .F. ) ;
#33620 = CARTESIAN_POINT ( 'NONE',  ( 5.121324086407808451, -26.64985754041175525, 6.800000000000000711 ) ) ;
#33621 = CARTESIAN_POINT ( 'NONE',  ( 1.259933197038312302, -26.09775540055275656, 7.013842709614101167 ) ) ;
#33622 = ORIENTED_EDGE ( 'NONE', *, *, #11418, .T. ) ;
#33623 = CARTESIAN_POINT ( 'NONE',  ( 24.66975522534114162, 2.992800531127576047, 3.487905392549471628 ) ) ;
#33624 = AXIS2_PLACEMENT_3D ( 'NONE', #12193, #28248, #18368 ) ;
#33625 = CARTESIAN_POINT ( 'NONE',  ( 81.87444285025600266, 65.47866087958055914, -1.319711737400975915 ) ) ;
#33626 = CARTESIAN_POINT ( 'NONE',  ( 79.58225024864498209, 65.28851876552752742, 3.146509185145913712 ) ) ;
#33627 = DIRECTION ( 'NONE',  ( 1.000000000000000000, -0.000000000000000000, 0.000000000000000000 ) ) ;
#33628 = VERTEX_POINT ( 'NONE', #2030 ) ;
#33629 = CARTESIAN_POINT ( 'NONE',  ( 79.04999676712192525, 61.38304106620122980, -3.266768353517003565 ) ) ;
#33631 = CARTESIAN_POINT ( 'NONE',  ( 14.70299449326277141, -4.943839671930780000, -2.500000000006339818 ) ) ;
#33630 = CARTESIAN_POINT ( 'NONE',  ( 26.76516748616653629, 0.8542131806872658162, 4.383548290790947100 ) ) ;
#33632 = CARTESIAN_POINT ( 'NONE',  ( 81.15569957775159082, 61.29889919928260156, -1.113695828830626455 ) ) ;
#33633 = CARTESIAN_POINT ( 'NONE',  ( 78.61725963159938146, 63.00713372587872385, 3.804514705604319591 ) ) ;
#33634 = ADVANCED_FACE ( 'NONE', ( #14547 ), #38013, .F. ) ;
#33635 = EDGE_CURVE ( 'NONE', #13175, #9154, #40231, .T. ) ;
#33636 = CARTESIAN_POINT ( 'NONE',  ( 36.51841587071722017, -3.542906066142682775, -5.805451938871582840 ) ) ;
#33637 = AXIS2_PLACEMENT_3D ( 'NONE', #30251, #33146, #5749 ) ;
#33638 = ADVANCED_FACE ( 'NONE', ( #16196 ), #366, .F. ) ;
#33639 = CARTESIAN_POINT ( 'NONE',  ( 81.30214557805317099, 65.90511036421355584, 1.555014038482367633 ) ) ;
#33641 = CARTESIAN_POINT ( 'NONE',  ( 14.69558838330753758, 3.996311804371543985, -6.000000000000000000 ) ) ;
#33640 = DIRECTION ( 'NONE',  ( 0.8660254037844452579, -0.4999999999999886202, 0.000000000000000000 ) ) ;
#33642 = CARTESIAN_POINT ( 'NONE',  ( 32.02118327030063227, -4.941963151977918578, 1.942379491845174444 ) ) ;
#33643 = CARTESIAN_POINT ( 'NONE',  ( -1.774482262040463665, -29.98858372608404110, 6.971170733404101760 ) ) ;
#33644 = DIRECTION ( 'NONE',  ( -0.000000000000000000, -1.000000000000000000, -0.000000000000000000 ) ) ;
#33645 = DIRECTION ( 'NONE',  ( 0.7660444431189857850, -0.6427876096865299260, -0.000000000000000000 ) ) ;
#33646 = CARTESIAN_POINT ( 'NONE',  ( 27.38334305430047166, 1.066451547753710871, -4.479821203429939835 ) ) ;
#33647 = CARTESIAN_POINT ( 'NONE',  ( -4.978675913592189417, -24.55319635012989110, 6.700000000000000178 ) ) ;
#33648 = FACE_OUTER_BOUND ( 'NONE', #18919, .T. ) ;
#33649 = CARTESIAN_POINT ( 'NONE',  ( 5.173272756311751763, -29.13508997310039206, 7.006908160621414972 ) ) ;
#33650 = DIRECTION ( 'NONE',  ( 0.000000000000000000, 0.000000000000000000, 1.000000000000000000 ) ) ;
#33651 = CARTESIAN_POINT ( 'NONE',  ( 29.48746289019463518, 1.218344962496953565, -4.224834120391865788 ) ) ;
#33652 = CARTESIAN_POINT ( 'NONE',  ( -68.92837670882107659, -42.87473357531881391, 0.000000000000000000 ) ) ;
#33653 = CARTESIAN_POINT ( 'NONE',  ( 27.42865362376633698, 1.027713267802376818, -4.487302781120154016 ) ) ;
#33654 = CARTESIAN_POINT ( 'NONE',  ( -11.81496944966682960, -21.25669541281728669, 4.000000000000000000 ) ) ;
#33655 = CYLINDRICAL_SURFACE ( 'NONE', #18631, 0.09010775117052972905 ) ;
#33656 = CYLINDRICAL_SURFACE ( 'NONE', #12139, 0.09010775117052798044 ) ;
#33657 = CARTESIAN_POINT ( 'NONE',  ( -72.87830298647827476, 3.234560164695657214, 10.95879046326537676 ) ) ;
#33658 = CARTESIAN_POINT ( 'NONE',  ( 4.908817600565330785, -28.44472466649483877, 7.784838882742139532 ) ) ;
#33659 = CARTESIAN_POINT ( 'NONE',  ( 4.921324086407802056, -26.64985754041175525, 6.700000000000000178 ) ) ;
#33660 = VERTEX_POINT ( 'NONE', #25272 ) ;
#33661 = CARTESIAN_POINT ( 'NONE',  ( -70.53757485429949270, -48.56857388652895224, 5.988040939572852217 ) ) ;
#33662 = CARTESIAN_POINT ( 'NONE',  ( 66.58549141467136678, 57.79032289594774596, 3.999530551061463157 ) ) ;
#33663 = CARTESIAN_POINT ( 'NONE',  ( 68.99357861020946814, 59.34113723602050783, -3.933428174212677320 ) ) ;
#33664 = CARTESIAN_POINT ( 'NONE',  ( -24.24874870218063450, -25.49307895267003587, 6.700000000000000178 ) ) ;
#33665 = ORIENTED_EDGE ( 'NONE', *, *, #3882, .F. ) ;
#33666 = CARTESIAN_POINT ( 'NONE',  ( 85.28844081106248609, 1.468752784057639094, 5.439171570854275828 ) ) ;
#33667 = VECTOR ( 'NONE', #33165, 1000.000000000000000 ) ;
#33668 = CARTESIAN_POINT ( 'NONE',  ( 0.1279077100727408489, -26.55541543726089060, 6.868387053540520704 ) ) ;
#33669 = CARTESIAN_POINT ( 'NONE',  ( 3.007898519841142981, -26.43137683128037452, 6.871394612369935651 ) ) ;
#33671 = CARTESIAN_POINT ( 'NONE',  ( 4.894364063540053600, -30.73549025348913588, 7.769368695748489095 ) ) ;
#33670 = CARTESIAN_POINT ( 'NONE',  ( -0.9606818258635283492, -27.29645349747919170, 6.894806418505347700 ) ) ;
#33672 = CARTESIAN_POINT ( 'NONE',  ( -60.92837670882106238, -37.87473357531881391, 0.000000000000000000 ) ) ;
#33673 = ORIENTED_EDGE ( 'NONE', *, *, #5841, .F. ) ;
#33674 = DIRECTION ( 'NONE',  ( 0.000000000000000000, 0.000000000000000000, 1.000000000000000000 ) ) ;
#33675 = DIRECTION ( 'NONE',  ( 0.4826092789263594640, 0.5751513419797960047, 0.6605219282605379050 ) ) ;
#33676 = ORIENTED_EDGE ( 'NONE', *, *, #24975, .F. ) ;
#33677 = CARTESIAN_POINT ( 'NONE',  ( 79.18319737856853635, 64.63648950223996792, -3.475409704257727217 ) ) ;
#33678 =( BOUNDED_CURVE ( )  B_SPLINE_CURVE ( 3, ( #18008, #8740, #5673, #30597 ),
 .UNSPECIFIED., .F., .T. ) 
 B_SPLINE_CURVE_WITH_KNOTS ( ( 4, 4 ),
 ( 1.347909859412852907, 1.534781240595297414 ),
 .UNSPECIFIED. ) 
 CURVE ( )  GEOMETRIC_REPRESENTATION_ITEM ( )  RATIONAL_B_SPLINE_CURVE ( ( 1.000000000000000000, 0.9970920404276226723, 0.9970920404276226723, 1.000000000000000000 ) ) 
 REPRESENTATION_ITEM ( '' )  );
#33679 = CARTESIAN_POINT ( 'NONE',  ( 15.85384049071795332, 7.981620597509389015, -3.484773916741112476 ) ) ;
#33680 = CARTESIAN_POINT ( 'NONE',  ( 80.40506551886717546, 65.76252680069852374, -2.626729253126910191 ) ) ;
#33681 = CARTESIAN_POINT ( 'NONE',  ( 80.48897389181450990, 62.29924170813984574, 3.301258712451522026 ) ) ;
#33682 = CARTESIAN_POINT ( 'NONE',  ( -2.749201978999709084, -28.00803730016500737, 7.695279973900954751 ) ) ;
#33683 = EDGE_CURVE ( 'NONE', #744, #26853, #34962, .T. ) ;
#33685 = VERTEX_POINT ( 'NONE', #19085 ) ;
#33684 = CARTESIAN_POINT ( 'NONE',  ( 2.704349939082798304, -26.31416920314327612, 7.139196562012273262 ) ) ;
#33686 = CARTESIAN_POINT ( 'NONE',  ( 21.85643539959775694, 0.3794388012242833064, 14.22155525766799045 ) ) ;
#33687 = VERTEX_POINT ( 'NONE', #18662 ) ;
#33688 = CARTESIAN_POINT ( 'NONE',  ( -80.90861860399087391, 11.45717611192839591, 0.6283086135788882309 ) ) ;
#33689 = CARTESIAN_POINT ( 'NONE',  ( 14.69558838330748785, -4.461849342347332659, 2.499999999999996891 ) ) ;
#33690 = CARTESIAN_POINT ( 'NONE',  ( -74.89083676646993126, 9.557107727799328600, -9.187685426891615492 ) ) ;
#33691 = LINE ( 'NONE', #11420, #21505 ) ;
#33692 = CARTESIAN_POINT ( 'NONE',  ( 35.83269171260823782, -3.732037575501295112, -5.621802225981361367 ) ) ;
#33693 = CARTESIAN_POINT ( 'NONE',  ( -1.765272865745179498, -30.05733663009887024, 7.754798119455333705 ) ) ;
#33694 = CARTESIAN_POINT ( 'NONE',  ( 14.77286119241257722, 13.14530852789250304, 2.499563476182618427 ) ) ;
#33695 = FACE_OUTER_BOUND ( 'NONE', #29414, .T. ) ;
#33696 = CARTESIAN_POINT ( 'NONE',  ( 31.24733724172370586, -0.3895753884219697039, 5.083300714914697593 ) ) ;
#33697 = CARTESIAN_POINT ( 'NONE',  ( 5.049232725593039817, -28.98234782857963410, 7.769368695748486431 ) ) ;
#33698 = VECTOR ( 'NONE', #16518, 1000.000000000000114 ) ;
#33699 = CARTESIAN_POINT ( 'NONE',  ( -10.44874870218064089, -26.64985754041175525, 6.800000000000000711 ) ) ;
#33700 = CARTESIAN_POINT ( 'NONE',  ( 87.30211668890848387, 0.2958435233019774402, 4.630501607711047463 ) ) ;
#33701 = CARTESIAN_POINT ( 'NONE',  ( 26.36036888033374126, 1.773289138066936665, -4.282619303848153258 ) ) ;
#33702 = ORIENTED_EDGE ( 'NONE', *, *, #30995, .F. ) ;
#33703 = CARTESIAN_POINT ( 'NONE',  ( 67.82906190410768943, 58.02404379074640417, 3.985511447369935123 ) ) ;
#33704 = CARTESIAN_POINT ( 'NONE',  ( 36.64688567981695400, -2.460106794591897295, 5.926030837251451189 ) ) ;
#33705 = EDGE_CURVE ( 'NONE', #2062, #16748, #31432, .T. ) ;
#33706 = CARTESIAN_POINT ( 'NONE',  ( 86.43196921298398649, 0.8512835087624049946, 5.909244108978848331 ) ) ;
#33708 = CARTESIAN_POINT ( 'NONE',  ( 21.78047190118184773, 5.616103730238553027, 3.473245441588607374 ) ) ;
#33707 = DIRECTION ( 'NONE',  ( -1.000000000000000000, 0.000000000000000000, 0.000000000000000000 ) ) ;
#33709 = CYLINDRICAL_SURFACE ( 'NONE', #16232, 0.1000000000000028644 ) ;
#33710 = CARTESIAN_POINT ( 'NONE',  ( 8.290806648384990041, -10.90558813203967148, -6.000000000000000000 ) ) ;
#33711 = CARTESIAN_POINT ( 'NONE',  ( 32.90365724210374765, -3.811969404918499560, 4.977804649287965510 ) ) ;
#33712 = CARTESIAN_POINT ( 'NONE',  ( -0.6777970675445941229, -32.13785343440231657, 7.011627023500182965 ) ) ;
#33713 = ORIENTED_EDGE ( 'NONE', *, *, #12792, .T. ) ;
#33714 = CARTESIAN_POINT ( 'NONE',  ( -70.93014222716664108, -21.78919581838237463, 6.013069300985384835 ) ) ;
#33715 = ADVANCED_FACE ( 'NONE', ( #28350 ), #31655, .F. ) ;
#33716 = EDGE_LOOP ( 'NONE', ( #18762, #26961, #40189, #3953, #1029, #16949 ) ) ;
#33717 = CARTESIAN_POINT ( 'NONE',  ( 78.81125837042770854, 65.77339625846090598, -2.277920705665355428 ) ) ;
#33718 = CARTESIAN_POINT ( 'NONE',  ( -1.557283979289156184, -28.29021886912457617, 6.864368109219936009 ) ) ;
#33719 = CARTESIAN_POINT ( 'NONE',  ( 79.23506694815802121, 65.34107492257680860, 3.003915454719612743 ) ) ;
#33720 = CARTESIAN_POINT ( 'NONE',  ( 26.54063429493796278, 1.105409551691596270, 4.373481918376509014 ) ) ;
#33723 = VERTEX_POINT ( 'NONE', #12286 ) ;
#33722 = DIRECTION ( 'NONE',  ( 1.000000000000000000, 0.000000000000000000, 0.000000000000000000 ) ) ;
#33721 = AXIS2_PLACEMENT_3D ( 'NONE', #21050, #6216, #15265 ) ;
#33724 = CARTESIAN_POINT ( 'NONE',  ( 73.98866219012947454, 61.81968298976576648, -3.762445401688966573 ) ) ;
#33725 = CARTESIAN_POINT ( 'NONE',  ( 3.291145163220645209, -32.57486068939992663, 6.863904403958576594 ) ) ;
#33726 = ADVANCED_FACE ( 'NONE', ( #26478 ), #39006, .T. ) ;
#33728 = DIRECTION ( 'NONE',  ( 1.165409145176969993E-16, -1.000000000000000000, 0.000000000000000000 ) ) ;
#33727 = CARTESIAN_POINT ( 'NONE',  ( 4.936849669449925315, -30.90234506304400952, 6.875780273367530171 ) ) ;
#33729 = PLANE ( 'NONE',  #27728 ) ;
#33730 = CARTESIAN_POINT ( 'NONE',  ( 81.35706873939174955, 65.93413826765582542, 1.000000000000000000 ) ) ;
#33731 = CARTESIAN_POINT ( 'NONE',  ( 24.66025866237015762, 2.990908695463429634, -3.498935737220656872 ) ) ;
#33732 = VERTEX_POINT ( 'NONE', #22992 ) ;
#33733 = CARTESIAN_POINT ( 'NONE',  ( -1.797364064287140906, -29.44672032744571055, 7.753200566781576875 ) ) ;
#33734 = CARTESIAN_POINT ( 'NONE',  ( 23.91855504425362255, 4.211737807167565961, 0.007810489111244203406 ) ) ;
#33735 = FACE_OUTER_BOUND ( 'NONE', #35066, .T. ) ;
#33736 = CARTESIAN_POINT ( 'NONE',  ( 1.076318136774142564, -33.00497882164555108, 7.778495531946297170 ) ) ;
#33737 = CARTESIAN_POINT ( 'NONE',  ( 81.53538963104975323, 62.13961868399318433, 2.518708746844631197 ) ) ;
#33738 = CARTESIAN_POINT ( 'NONE',  ( 84.25787434187677150, 2.991901652185509075, -1.300773176381055940 ) ) ;
#33739 = DIRECTION ( 'NONE',  ( 0.000000000000000000, 1.000000000000000000, 0.000000000000000000 ) ) ;
#33740 = ORIENTED_EDGE ( 'NONE', *, *, #27271, .T. ) ;
#33741 = FACE_OUTER_BOUND ( 'NONE', #8878, .T. ) ;
#33742 = VECTOR ( 'NONE', #35753, 1000.000000000000000 ) ;
#33744 = EDGE_CURVE ( 'NONE', #19079, #10898, #972, .T. ) ;
#33743 = VERTEX_POINT ( 'NONE', #29362 ) ;
#33745 = CARTESIAN_POINT ( 'NONE',  ( 4.078577254010792075, -27.00200693238450000, 7.011627023500183853 ) ) ;
#33746 = CARTESIAN_POINT ( 'NONE',  ( 18.22228433872105313, -2.944577058405784875, -3.048495850186285772 ) ) ;
#33747 = CARTESIAN_POINT ( 'NONE',  ( 30.51370498771255768, -0.1447642529027365621, -4.968799658713162870 ) ) ;
#33748 = CARTESIAN_POINT ( 'NONE',  ( 1.300000000000000044, 0.5999999999999995337, 4.250000000000000000 ) ) ;
#33749 = CARTESIAN_POINT ( 'NONE',  ( 1.904238495577618151, -26.17604549525697522, 6.920489980334476599 ) ) ;
#33750 = ORIENTED_EDGE ( 'NONE', *, *, #15565, .F. ) ;
#33751 = CYLINDRICAL_SURFACE ( 'NONE', #25718, 0.09010775117052914618 ) ;
#33752 = DIRECTION ( 'NONE',  ( 0.000000000000000000, 0.000000000000000000, 1.000000000000000000 ) ) ;
#33753 = AXIS2_PLACEMENT_3D ( 'NONE', #8714, #6469, #12626 ) ;
#33754 = PLANE ( 'NONE',  #10876 ) ;
#33755 = B_SPLINE_CURVE_WITH_KNOTS ( 'NONE', 3,
 ( #30569, #24375, #38590, #10396, #35535, #7309, #19866, #8508, #17977, #10984, #1964, #2162, #13891, #33037, #5030, #7708, #20458, #14481, #29935, #34121, #39095, #30047, #751, #12679, #346, #24567, #30551, #37118, #34274, #6043, #31165 ),
 .UNSPECIFIED., .F., .F.,
 ( 4, 3, 3, 3, 3, 3, 3, 3, 3, 3, 4 ),
 ( 4.336808689942017736E-19, 3.077658087705710549E-05, 6.152638666999027720E-05, 9.267501192706690811E-05, 0.0001241882240135190087, 0.0001556618703051683178, 0.0001866161554452223036, 0.0002167966385860985808, 0.0002463805737537785737, 0.0002758761370306538996, 0.0002847094172290079222 ),
 .UNSPECIFIED. ) ;
#33756 = CARTESIAN_POINT ( 'NONE',  ( 5.651251297819362307, -25.49307895267003587, 6.700000000000000178 ) ) ;
#33757 = ORIENTED_EDGE ( 'NONE', *, *, #5170, .F. ) ;
#33758 = ORIENTED_EDGE ( 'NONE', *, *, #34522, .T. ) ;
#33760 = CARTESIAN_POINT ( 'NONE',  ( 36.44569688397662333, -1.731580701890905072, 5.730255527505096147 ) ) ;
#33759 = CARTESIAN_POINT ( 'NONE',  ( 81.32346312764153140, 61.65804850752792987, -2.069468987430089779 ) ) ;
#33761 = CARTESIAN_POINT ( 'NONE',  ( 26.05544091025929276, -2.756875503939111294, 4.272979725902397163 ) ) ;
#33762 = ADVANCED_FACE ( 'NONE', ( #35559 ), #4652, .T. ) ;
#33763 = EDGE_CURVE ( 'NONE', #27958, #32955, #19885, .T. ) ;
#33764 = CARTESIAN_POINT ( 'NONE',  ( 21.93632313734164185, -3.072674611199754491, -3.536223897022242824 ) ) ;
#33765 = DIRECTION ( 'NONE',  ( -0.000000000000000000, -0.000000000000000000, -1.000000000000000000 ) ) ;
#33766 = VERTEX_POINT ( 'NONE', #13298 ) ;
#33767 = ADVANCED_FACE ( 'NONE', ( #13109 ), #25669, .F. ) ;
#33768 = CARTESIAN_POINT ( 'NONE',  ( -80.92837670882107659, 2.429809908903242555, -12.50000000000000000 ) ) ;
#33769 = ORIENTED_EDGE ( 'NONE', *, *, #34903, .F. ) ;
#33770 = VECTOR ( 'NONE', #37420, 1000.000000000000000 ) ;
#33771 = ORIENTED_EDGE ( 'NONE', *, *, #22982, .T. ) ;
#33772 = DIRECTION ( 'NONE',  ( -0.9848077530122069101, -0.1736481776669374644, -0.000000000000000000 ) ) ;
#33773 = CARTESIAN_POINT ( 'NONE',  ( 78.81037980241194418, 65.98117473861063331, -1.881209715725460141 ) ) ;
#33774 = CARTESIAN_POINT ( 'NONE',  ( 14.75265942311007983, -4.610020690361468887, 2.508566039384218627 ) ) ;
#33775 = EDGE_LOOP ( 'NONE', ( #9643, #29143, #17022, #5248 ) ) ;
#33777 = CARTESIAN_POINT ( 'NONE',  ( 21.42989180576616803, 8.003656144025150354, -2.742373372379655283 ) ) ;
#33776 = CARTESIAN_POINT ( 'NONE',  ( 23.08977137947836056, 2.997041596059222268, 4.148509914069672178 ) ) ;
#33778 = CARTESIAN_POINT ( 'NONE',  ( 80.99701317011651724, 65.74337749817941301, -2.326649614738085514 ) ) ;
#33779 = CARTESIAN_POINT ( 'NONE',  ( -71.80203242198795976, -21.28647353953329358, 3.936269516591345052 ) ) ;
#33780 = ADVANCED_FACE ( 'NONE', ( #29755, #38612 ), #23383, .T. ) ;
#33782 = CARTESIAN_POINT ( 'NONE',  ( 22.07382372493323786, -2.652280543961057724, -3.651552068356747061 ) ) ;
#33781 = CARTESIAN_POINT ( 'NONE',  ( 0.1825688514436868137, -0.5999999999999994227, -3.931742364907163001 ) ) ;
#33783 = CARTESIAN_POINT ( 'NONE',  ( -1.799033128594637931, -29.50575927414515576, 6.870737987065012042 ) ) ;
#33784 = CARTESIAN_POINT ( 'NONE',  ( 73.85752424338471656, 60.59307193704751882, 3.935025356177997757 ) ) ;
#33785 = CARTESIAN_POINT ( 'NONE',  ( 22.44967802737946272, 3.154736390076984698, -4.439590424646853606 ) ) ;
#33786 = CARTESIAN_POINT ( 'NONE',  ( 21.85643539959774273, 10.50077279934518160, -1.805501455388072385 ) ) ;
#33787 = PLANE ( 'NONE',  #19694 ) ;
#33788 = ORIENTED_EDGE ( 'NONE', *, *, #5011, .T. ) ;
#33789 = CARTESIAN_POINT ( 'NONE',  ( -63.99293516169444729, 35.89893413629672381, 7.506047544094568202 ) ) ;
#33790 = CARTESIAN_POINT ( 'NONE',  ( 79.66325760479746521, 66.16013226748967213, 2.011780557866075458 ) ) ;
#33791 = CARTESIAN_POINT ( 'NONE',  ( 87.26180097699096905, 0.3411280444268214862, 4.951700522085849876 ) ) ;
#33792 = CARTESIAN_POINT ( 'NONE',  ( -0.9786759135921931918, -24.55319635012989110, 6.700000000000000178 ) ) ;
#33793 = LINE ( 'NONE', #1899, #9596 ) ;
#33794 = CARTESIAN_POINT ( 'NONE',  ( -64.08758708074093136, 38.76906266698303227, 3.000000000000000000 ) ) ;
#33796 = ADVANCED_FACE ( 'NONE', ( #16390 ), #20087, .F. ) ;
#33795 = VERTEX_POINT ( 'NONE', #32863 ) ;
#33797 = CARTESIAN_POINT ( 'NONE',  ( 15.61919507633180615, -3.751113255642578359, 2.631306685128067091 ) ) ;
#33798 = CARTESIAN_POINT ( 'NONE',  ( -70.92837670882107659, -60.53509472482660669, 0.000000000000000000 ) ) ;
#33799 = CARTESIAN_POINT ( 'NONE',  ( 35.45425782886216837, -1.912984739101698750, -5.739892417296534433 ) ) ;
#33800 = CARTESIAN_POINT ( 'NONE',  ( 5.189116403693322610, -29.65506484607316651, 7.780491323090178213 ) ) ;
#33801 = CARTESIAN_POINT ( 'NONE',  ( -24.97867591359219475, -26.64985754041175525, 6.800000000000000711 ) ) ;
#33802 = EDGE_CURVE ( 'NONE', #1190, #40382, #13717, .T. ) ;
#33803 = CARTESIAN_POINT ( 'NONE',  ( 4.389428757393228686, -31.81026445011082870, 7.756742906098587298 ) ) ;
#33804 = VECTOR ( 'NONE', #4685, 1000.000000000000000 ) ;
#33805 = CARTESIAN_POINT ( 'NONE',  ( -75.45330471031414277, 33.71485196875532608, -12.49999999999999645 ) ) ;
#33806 = EDGE_CURVE ( 'NONE', #16613, #14683, #4813, .T. ) ;
#33807 = CIRCLE ( 'NONE', #16698, 0.1000000000000028644 ) ;
#33808 = VERTEX_POINT ( 'NONE', #7529 ) ;
#33809 = CARTESIAN_POINT ( 'NONE',  ( 23.31574270449137387, 3.489135525515108416, 3.362528818731710167 ) ) ;
#33810 = CARTESIAN_POINT ( 'NONE',  ( -2.954197855305039422, -12.43481156997016157, 1.000000000000000000 ) ) ;
#33811 = PLANE ( 'NONE',  #37546 ) ;
#33812 = EDGE_CURVE ( 'NONE', #12703, #9079, #29163, .T. ) ;
#33813 = DIRECTION ( 'NONE',  ( 0.8660254037844449249, -0.4999999999999888423, -0.000000000000000000 ) ) ;
#33814 = ORIENTED_EDGE ( 'NONE', *, *, #22427, .T. ) ;
#33815 = CARTESIAN_POINT ( 'NONE',  ( -0.4603391584254019064, -32.19504905708794951, 7.721096864323896192 ) ) ;
#33816 = CARTESIAN_POINT ( 'NONE',  ( -73.80328626875311215, 8.420059221808692485, -9.582109240214750301 ) ) ;
#33817 = CARTESIAN_POINT ( 'NONE',  ( 67.37456247186543123, 58.43133532855971879, 3.984420468527628767 ) ) ;
#33818 = CARTESIAN_POINT ( 'NONE',  ( -18.44874870218064089, -26.64985754041175525, 6.800000000000000711 ) ) ;
#33819 = B_SPLINE_SURFACE_WITH_KNOTS ( 'NONE', 5, 3, ( 
 ( #15202, #39911, #12520, #28165, #24677, #21392, #11685, #18282, #12099, #8607, #34379, #36619, #36825, #21599, #15402, #27962, #17867, #34179, #8405, #21185, #6154, #18483, #2257, #2881, #33966, #2474, #40505, #2679, #12315, #5333, #33557, #30451, #24890, #27352, #14997, #27557, #40114, #37022, #8806, #5740, #1004, #19315, #9422, #9844, #19522, #22822, #32297, #18910 ),
 ( #25094, #795, #3497, #6963, #16608, #35392, #396, #16221, #7162, #25496, #22419, #38241, #34586, #38438, #19724, #34989, #37623, #3700, #28587, #4095, #31478, #32102, #25698, #6763, #10243, #31889, #10042, #29192, #28795, #13326, #22011, #6361, #599, #13139, #22622, #35191, #16420, #3908, #3301, #28993, #25902, #15822, #28377, #187, #12724, #25300, #37835, #9638 ),
 ( #22220, #34790, #6566, #31679, #19113, #16020, #12934, #4679, #29989, #17407, #4871, #26310, #23798, #13936, #23609, #23020, #20715, #36173, #33301, #35780, #14329, #29393, #38643, #7359, #7759, #1804, #13538, #23216, #32891, #32488, #10441, #7955, #20503, #5081, #4491, #39442, #17613, #35978, #20306, #17012, #30192, #33087, #8144, #26900, #1599, #16815, #29783, #26507 ),
 ( #17213, #26112, #11232, #36373, #35588, #4288, #11031, #1212, #14130, #26707, #38844, #19917, #13747, #10639, #39241, #7558, #20113, #32692, #29588, #1404, #39037, #10838, #23414, #8352, #33919, #27515, #14730, #2633, #24424, #36980, #11435, #15358, #27102, #8761, #39652, #24840, #37387, #33512, #15153, #27913, #2210, #18643, #21344, #24000, #40067, #37181, #40459, #9181 ),
 ( #27303, #39867, #2011, #36572, #12268, #14949, #5283, #14530, #21753, #11638, #5696, #12049, #17821, #34336, #24628, #30403, #18236, #6107, #36776, #24216, #8558, #27710, #21140, #40264, #11846, #30826, #33706, #8968, #5903, #21555, #34132, #5487, #18029, #30621, #18440, #31029, #2835, #2428, #6916, #31633, #37994, #25650, #25050, #28330, #3857, #25452, #146, #31838 ),
 ( #9379, #7115, #13283, #38392, #25253, #749, #31228, #3049, #22378, #38194, #32051, #22174, #28744, #31433, #34537, #22576, #16176, #37784, #9796, #15776, #9995, #12677, #15569, #19476, #9591, #13089, #22778, #28947, #6522, #34942, #25855, #3457, #28535, #3650, #12480, #16373, #10194, #344, #28122, #6721, #34743, #35345, #37583, #35144, #553, #12888, #21966, #19272 ),
 ( #6311, #18860, #3255, #19069, #15971, #4449, #20464, #29346, #36135, #20072, #26463, #14084, #13489, #16765, #33043, #13897, #1168, #20265, #23169, #35934, #38597, #36331, #1757, #26857, #13698, #29940, #19679, #32252, #10789, #26662, #4833, #10594, #35738, #17365, #39400, #1363, #38991, #7511, #4051, #1553, #14289, #23569, #7715, #22976, #4638, #32648, #11189, #38797 ),
 ( #7915, #39196, #23760, #10400, #17169, #7312, #23366, #29738, #32443, #16566, #29148, #19871, #10990, #954, #26063, #4240, #26265, #16973, #29545, #21507, #5652, #14490, #40023, #33666, #20882, #8718, #30571, #2379, #17568, #34085, #33253, #14900, #5036, #30984, #2788, #27063, #21297, #5860, #8306, #33872, #18396, #33470, #24797, #27468, #30152, #5444, #2585, #15315 ) ),
 .UNSPECIFIED., .F., .T., .F.,
 ( 6, 2, 6 ),
 ( 4, 1, 1, 1, 1, 1, 1, 1, 1, 1, 1, 1, 1, 1, 1, 1, 1, 1, 1, 1, 1, 1, 1, 1, 1, 1, 1, 1, 1, 1, 1, 1, 1, 1, 1, 1, 1, 1, 1, 1, 1, 1, 1, 1, 1, 4 ),
 ( 0.000000000000000000, 0.5000000000000000000, 1.000000000000000000 ),
 ( 0.02319993227479018663, 0.02338707809474536645, 0.02357422391470053238, 0.02376136973465571220, 0.02401089749459594039, 0.02432280719452123083, 0.02469709883443158005, 0.02507139047434192580, 0.02557044599422238565, 0.02619426539407297347, 0.02694284867389366844, 0.02769143195371436342, 0.02844001523353506186, 0.02918859851335575684, 0.02993718179317645181, 0.03068576507299715025, 0.03143434835281785217, 0.03218293163263854367, 0.03293151491245924212, 0.03355533431230981606, 0.03405438983219027937, 0.03442868147210063207, 0.03480297311201098476, 0.03511488281193627520, 0.03536441057187650339, 0.03555155639183167626, 0.03573870221178684914, 0.03598822997172709121, 0.03630013967165238165, 0.03667443131156272740, 0.03704872295147307315, 0.03754777847135353647, 0.03817159787120411735, 0.03892018115102481579, 0.03966876443084551424, 0.04041734771066620574, 0.04141545875042713931, 0.04241356979018806594, 0.04341168082994899952, 0.04416026410976969102, 0.04490884738959038947, 0.04553266678944096341, 0.04603172230932142672, 0.04640601394923177248, 0.04678030558914212517, 0.04715459722905247786 ),
 .UNSPECIFIED. ) ;
#33820 = ORIENTED_EDGE ( 'NONE', *, *, #16501, .T. ) ;
#33821 = DIRECTION ( 'NONE',  ( -0.000000000000000000, -0.000000000000000000, 1.000000000000000000 ) ) ;
#33822 = CARTESIAN_POINT ( 'NONE',  ( -58.99872204295123623, 28.54795728317104064, -6.891578894883706674 ) ) ;
#33823 = VERTEX_POINT ( 'NONE', #767 ) ;
#33824 = CARTESIAN_POINT ( 'NONE',  ( 23.42497383391232191, 3.742411600671747607, 3.213303063791231207 ) ) ;
#33825 = CARTESIAN_POINT ( 'NONE',  ( 80.70729934198669753, 66.20774049649585891, -1.233992409460997086 ) ) ;
#33827 = AXIS2_PLACEMENT_3D ( 'NONE', #25804, #29691, #17120 ) ;
#33826 = CARTESIAN_POINT ( 'NONE',  ( 78.79648636889820068, 65.96905942459900984, 1.896863055073862103 ) ) ;
#33828 = AXIS2_PLACEMENT_3D ( 'NONE', #35714, #20050, #27643 ) ;
#33829 = DIRECTION ( 'NONE',  ( 1.000000000000000000, 0.000000000000000000, -0.000000000000000000 ) ) ;
#33830 = ORIENTED_EDGE ( 'NONE', *, *, #36561, .T. ) ;
#33831 = CARTESIAN_POINT ( 'NONE',  ( 77.57912958173203322, 64.32824690378613752, -3.266768353516996903 ) ) ;
#33833 = CARTESIAN_POINT ( 'NONE',  ( 14.74692632493244027, -5.123162004414108850, -2.499999999977825738 ) ) ;
#33832 = CARTESIAN_POINT ( 'NONE',  ( 23.05082101514768667, 0.3401240180440390226, 5.963255066552523687 ) ) ;
#33834 = CARTESIAN_POINT ( 'NONE',  ( 78.83208086995163910, 66.11806168415770912, -1.392093260604380545 ) ) ;
#33835 = DIRECTION ( 'NONE',  ( 1.000000000000000000, 0.000000000000000000, 0.000000000000000000 ) ) ;
#33836 = CARTESIAN_POINT ( 'NONE',  ( 77.86640729734749300, 62.36914183036536485, 3.839379600940521442 ) ) ;
#33837 = ORIENTED_EDGE ( 'NONE', *, *, #21102, .F. ) ;
#33838 = AXIS2_PLACEMENT_3D ( 'NONE', #19617, #32191, #38934 ) ;
#33839 = CARTESIAN_POINT ( 'NONE',  ( 36.77396871613090923, -3.421702227977501565, -5.878726859251444559 ) ) ;
#33840 = AXIS2_PLACEMENT_3D ( 'NONE', #23766, #36540, #32854 ) ;
#33841 = CARTESIAN_POINT ( 'NONE',  ( 80.64785791202346843, 66.17610879001711055, 1.553473047276234587 ) ) ;
#33843 = CARTESIAN_POINT ( 'NONE',  ( -1.694407884520888752, -29.38183540858682363, 6.895222827070020877 ) ) ;
#33842 = CARTESIAN_POINT ( 'NONE',  ( -0.2487487021806331078, -26.64985754041175525, 6.700000000000000178 ) ) ;
#33844 = CARTESIAN_POINT ( 'NONE',  ( 28.07449379822080004, 1.807001228253011016, 3.913063849393144888 ) ) ;
#33845 = CARTESIAN_POINT ( 'NONE',  ( -1.774643799394317156, -29.98723051182367882, 6.961115707816238896 ) ) ;
#33846 = CARTESIAN_POINT ( 'NONE',  ( -1.267148935398236143, -27.71435023938598619, 7.753200566781576875 ) ) ;
#33847 = CARTESIAN_POINT ( 'NONE',  ( 1.546080347881852335, -33.06653896731305764, 6.880828092187097234 ) ) ;
#33848 = B_SPLINE_CURVE_WITH_KNOTS ( 'NONE', 3,
 ( #37195, #34555, #31447, #22188, #3269, #8985, #28345, #21361 ),
 .UNSPECIFIED., .F., .F.,
 ( 4, 2, 2, 4 ),
 ( 0.000000000000000000, 0.0004377122104129928964, 0.0006565683156194867696, 0.0008754244208259806970 ),
 .UNSPECIFIED. ) ;
#33849 = CARTESIAN_POINT ( 'NONE',  ( -32.97867591359219119, -24.55319635012989110, 6.700000000000000178 ) ) ;
#33850 = EDGE_CURVE ( 'NONE', #16288, #25100, #9837, .T. ) ;
#33851 = CARTESIAN_POINT ( 'NONE',  ( 2.474049714983546089, -33.27093018339341057, 7.013842709614101167 ) ) ;
#33852 = CARTESIAN_POINT ( 'NONE',  ( 81.14431910071698439, 61.29472151471745178, 1.169926324511519455 ) ) ;
#33853 = CARTESIAN_POINT ( 'NONE',  ( 5.153279172109080264, -30.14225614731511982, 7.685194954629195330 ) ) ;
#33854 = CARTESIAN_POINT ( 'NONE',  ( 37.15950049230122687, -2.950588481368993321, -5.999614729618140352 ) ) ;
#33855 = DIRECTION ( 'NONE',  ( -0.000000000000000000, -0.000000000000000000, 1.000000000000000000 ) ) ;
#33856 = CARTESIAN_POINT ( 'NONE',  ( 5.200390093233090205, -29.56993018339339940, 6.929570838012950595 ) ) ;
#33857 = LINE ( 'NONE', #15093, #23302 ) ;
#33858 = DIRECTION ( 'NONE',  ( -0.000000000000000000, -0.000000000000000000, 1.000000000000000000 ) ) ;
#33859 = DIRECTION ( 'NONE',  ( 0.000000000000000000, 0.000000000000000000, -1.000000000000000000 ) ) ;
#33860 = B_SPLINE_CURVE_WITH_KNOTS ( 'NONE', 3,
 ( #5638, #30769, #21494, #24363, #8293, #37122, #8910, #2571, #18178, #40208 ),
 .UNSPECIFIED., .F., .F.,
 ( 4, 3, 3, 4 ),
 ( 0.0001585009270395693266, 0.0001815657551981851700, 0.0002118214035944126139, 0.0002170292169044741302 ),
 .UNSPECIFIED. ) ;
#33861 = FACE_OUTER_BOUND ( 'NONE', #9134, .T. ) ;
#33862 = VECTOR ( 'NONE', #18783, 1000.000000000000000 ) ;
#33863 = CARTESIAN_POINT ( 'NONE',  ( 24.87654660328950129, 1.883990792660638069, -4.293584299149880934 ) ) ;
#33864 = CARTESIAN_POINT ( 'NONE',  ( -32.24874870218063450, -26.64985754041175525, 6.700000000000000178 ) ) ;
#33865 = ORIENTED_EDGE ( 'NONE', *, *, #36733, .T. ) ;
#33866 = ORIENTED_EDGE ( 'NONE', *, *, #24110, .F. ) ;
#33867 = DIRECTION ( 'NONE',  ( 1.165409145176969993E-16, -1.000000000000000000, 0.000000000000000000 ) ) ;
#33868 = CARTESIAN_POINT ( 'NONE',  ( 69.33847993643759366, 58.44820081139205570, -3.962610901733986335 ) ) ;
#33869 = ADVANCED_FACE ( 'NONE', ( #11207 ), #24397, .F. ) ;
#33870 = AXIS2_PLACEMENT_3D ( 'NONE', #38603, #34948, #38806 ) ;
#33871 = ORIENTED_EDGE ( 'NONE', *, *, #11795, .F. ) ;
#33872 = CARTESIAN_POINT ( 'NONE',  ( 87.82658540711466344, -2.392274210255118216, -1.851534029869310816 ) ) ;
#33873 = EDGE_CURVE ( 'NONE', #34747, #37237, #28476, .T. ) ;
#33874 = LINE ( 'NONE', #40418, #20634 ) ;
#33875 = CARTESIAN_POINT ( 'NONE',  ( 69.89919258653301881, 58.73135405362895511, 3.965028736237032891 ) ) ;
#33876 = CARTESIAN_POINT ( 'NONE',  ( -32.87867591359218977, -26.64985754041175525, 6.800000000000000711 ) ) ;
#33878 = CARTESIAN_POINT ( 'NONE',  ( 1.243865080918407529, -26.20070406487326764, 6.865312560952602894 ) ) ;
#33877 = CARTESIAN_POINT ( 'NONE',  ( -0.8600751803131411188, -27.18371306214347527, 6.912143950357343414 ) ) ;
#33879 = SHAPE_DEFINITION_REPRESENTATION ( #17689, #131 ) ;
#33880 = CARTESIAN_POINT ( 'NONE',  ( -1.799566460562916470, -29.58736926422850999, 7.749999999999998224 ) ) ;
#33881 = EDGE_LOOP ( 'NONE', ( #34090, #8314, #37428, #9853 ) ) ;
#33882 = CARTESIAN_POINT ( 'NONE',  ( 23.14331707321704457, 4.052454345113581269, 3.066645182171226836 ) ) ;
#33883 = DIRECTION ( 'NONE',  ( -0.000000000000000000, -1.000000000000000000, -0.000000000000000000 ) ) ;
#33884 = EDGE_LOOP ( 'NONE', ( #30032, #16057, #21968, #34227, #19577 ) ) ;
#33885 = CARTESIAN_POINT ( 'NONE',  ( 79.50676573472793507, 64.15826028415024496, -3.676305632669317536 ) ) ;
#33886 = LINE ( 'NONE', #30377, #13811 ) ;
#33887 = CARTESIAN_POINT ( 'NONE',  ( 80.14906791408208164, 65.90796394341647613, -2.445541897054225977 ) ) ;
#33888 = CARTESIAN_POINT ( 'NONE',  ( 78.87241222613832292, 65.34207468649373141, 2.902290250791179194 ) ) ;
#33889 = CIRCLE ( 'NONE', #6923, 2.500000000000000444 ) ;
#33890 = AXIS2_PLACEMENT_3D ( 'NONE', #17880, #33367, #30253 ) ;
#33891 = CARTESIAN_POINT ( 'NONE',  ( 22.01622206693788897, 4.835086392017111656, 3.641232820207879417 ) ) ;
#33892 = B_SPLINE_CURVE_WITH_KNOTS ( 'NONE', 3,
 ( #18682, #23009, #7150, #22811, #13127, #29181, #1199, #16599, #990, #588 ),
 .UNSPECIFIED., .F., .F.,
 ( 4, 3, 3, 4 ),
 ( 0.0001585009270395721455, 0.0001815657551981848447, 0.0002118214035944132373, 0.0002170292169044773015 ),
 .UNSPECIFIED. ) ;
#33894 = ORIENTED_EDGE ( 'NONE', *, *, #40384, .F. ) ;
#33893 = CYLINDRICAL_SURFACE ( 'NONE', #9108, 2.500000000000002220 ) ;
#33895 = CARTESIAN_POINT ( 'NONE',  ( 22.56491764776242803, -2.112007571549842755, -8.936849366082922685 ) ) ;
#33896 = ORIENTED_EDGE ( 'NONE', *, *, #9542, .F. ) ;
#33897 = CARTESIAN_POINT ( 'NONE',  ( -2.978675913592195190, -24.55319635012989110, 6.700000000000000178 ) ) ;
#33898 = FACE_OUTER_BOUND ( 'NONE', #8392, .T. ) ;
#33899 = AXIS2_PLACEMENT_3D ( 'NONE', #14091, #13902, #8107 ) ;
#33900 = CARTESIAN_POINT ( 'NONE',  ( -1.426118936618665067, -27.98159272051555035, 7.139344958878413472 ) ) ;
#33901 = CARTESIAN_POINT ( 'NONE',  ( -78.34784942564689914, 10.09360306622668446, -8.412543785568951549 ) ) ;
#33902 = CARTESIAN_POINT ( 'NONE',  ( 1.700390093233090871, -29.56993018339339940, -2.499999999999998668 ) ) ;
#33903 = CARTESIAN_POINT ( 'NONE',  ( 36.88828627238819280, -3.352251944545559414, -5.910322522570560899 ) ) ;
#33904 = DIRECTION ( 'NONE',  ( -0.000000000000000000, -0.000000000000000000, 1.000000000000000000 ) ) ;
#33905 = CARTESIAN_POINT ( 'NONE',  ( 15.30733144061336581, 11.48784145168144732, 2.585939450232884962 ) ) ;
#33906 = CARTESIAN_POINT ( 'NONE',  ( 2.304086713256504382, -32.91590543598751850, 7.635761828346577573 ) ) ;
#33907 = DIRECTION ( 'NONE',  ( -0.6502177225477870914, -0.3754033771448342938, -0.6605219282605403475 ) ) ;
#33908 = CARTESIAN_POINT ( 'NONE',  ( 17.85923178500418373, 13.84674244481094085, -2.499999999999999556 ) ) ;
#33909 = LINE ( 'NONE', #22163, #25385 ) ;
#33910 = CARTESIAN_POINT ( 'NONE',  ( 24.42208616128406362, 2.821435771912959023, -3.829602786363869971 ) ) ;
#33911 = ORIENTED_EDGE ( 'NONE', *, *, #39641, .T. ) ;
#33912 = CARTESIAN_POINT ( 'NONE',  ( 67.51064039993573829, 57.98508837280776618, 3.992553130659727056 ) ) ;
#33913 = CARTESIAN_POINT ( 'NONE',  ( 31.78478551401448016, -0.3652337162497744649, 5.167182516041234130 ) ) ;
#33914 = CYLINDRICAL_SURFACE ( 'NONE', #36894, 3.399999999999999911 ) ;
#33915 = EDGE_CURVE ( 'NONE', #11496, #1708, #31946, .T. ) ;
#33916 = AXIS2_PLACEMENT_3D ( 'NONE', #3487, #40709, #12510 ) ;
#33917 = CARTESIAN_POINT ( 'NONE',  ( -22.24874870218063450, -26.64985754041175525, 6.700000000000000178 ) ) ;
#33918 = AXIS2_PLACEMENT_3D ( 'NONE', #19736, #32310, #4107 ) ;
#33919 = CARTESIAN_POINT ( 'NONE',  ( 86.17769677085827595, 1.483769024673816661, 5.380928644057212828 ) ) ;
#33920 = ADVANCED_FACE ( 'NONE', ( #2185 ), #18003, .T. ) ;
#33922 = CARTESIAN_POINT ( 'NONE',  ( 4.838943445346131966, -30.87743861000141621, 6.871394612369933874 ) ) ;
#33921 = LINE ( 'NONE', #27304, #40593 ) ;
#33923 = CARTESIAN_POINT ( 'NONE',  ( -10.97867591359219475, -26.64985754041175525, 6.700000000000000178 ) ) ;
#33924 =( BOUNDED_CURVE ( )  B_SPLINE_CURVE ( 3, ( #18043, #39458, #39666, #2444 ),
 .UNSPECIFIED., .F., .T. ) 
 B_SPLINE_CURVE_WITH_KNOTS ( ( 4, 4 ),
 ( 0.6656944266037789770, 1.570796326794896558 ),
 .UNSPECIFIED. ) 
 CURVE ( )  GEOMETRIC_REPRESENTATION_ITEM ( )  RATIONAL_B_SPLINE_CURVE ( ( 1.000000000000000000, 0.9328897322841716022, 0.9328897322841716022, 1.000000000000000000 ) ) 
 REPRESENTATION_ITEM ( '' )  );
#33925 = ORIENTED_EDGE ( 'NONE', *, *, #28157, .F. ) ;
#33926 = LINE ( 'NONE', #5700, #1163 ) ;
#33927 = CIRCLE ( 'NONE', #20721, 0.1000000000000028644 ) ;
#33928 = CARTESIAN_POINT ( 'NONE',  ( 5.150202707224498688, -30.16051711886163744, 7.750000000000001776 ) ) ;
#33929 = VERTEX_POINT ( 'NONE', #14505 ) ;
#33930 = PLANE ( 'NONE',  #23437 ) ;
#33931 = ORIENTED_EDGE ( 'NONE', *, *, #31284, .F. ) ;
#33932 = CARTESIAN_POINT ( 'NONE',  ( 79.58170130377179419, 64.56493525204570005, -3.531602295408449610 ) ) ;
#33933 = CARTESIAN_POINT ( 'NONE',  ( -1.743365991543899485, -30.19486540288534826, 7.750000000000001776 ) ) ;
#33934 = CARTESIAN_POINT ( 'NONE',  ( 80.06960825067233145, 63.75365790317244574, 3.697630003121160414 ) ) ;
#33936 = ORIENTED_EDGE ( 'NONE', *, *, #10757, .T. ) ;
#33935 = LINE ( 'NONE', #12065, #39406 ) ;
#33937 = CARTESIAN_POINT ( 'NONE',  ( 74.11268706641025972, 61.54722250361106717, -3.856662941142631418 ) ) ;
#33938 = CARTESIAN_POINT ( 'NONE',  ( 2.921324086407800280, -24.55319635012989110, 6.700000000000000178 ) ) ;
#33940 = CARTESIAN_POINT ( 'NONE',  ( -17.69482985384421880, -29.56993018339339940, 6.000000000000000000 ) ) ;
#33939 = CARTESIAN_POINT ( 'NONE',  ( 4.918507887475499274, -30.94605444427887520, 6.961115707816230902 ) ) ;
#33941 = CARTESIAN_POINT ( 'NONE',  ( -17.27251170661583402, 3.729367930467589076, 6.000000000000000000 ) ) ;
#33942 = CARTESIAN_POINT ( 'NONE',  ( 14.77222811005485603, -4.461988841550141416, 2.511961482897715481 ) ) ;
#33943 = EDGE_CURVE ( 'NONE', #25803, #6772, #11407, .T. ) ;
#33944 = CARTESIAN_POINT ( 'NONE',  ( 24.32052479808152157, 3.131090298592408949, -3.427421788660176105 ) ) ;
#33945 = ORIENTED_EDGE ( 'NONE', *, *, #2148, .F. ) ;
#33946 = CARTESIAN_POINT ( 'NONE',  ( 5.018308223201096041, -30.31257054894095049, 6.871394612369936539 ) ) ;
#33947 = VECTOR ( 'NONE', #1584, 1000.000000000000000 ) ;
#33948 = CARTESIAN_POINT ( 'NONE',  ( 23.94338804316802438, 3.829326634665836782, 2.990621344434266415 ) ) ;
#33949 = VECTOR ( 'NONE', #33821, 1000.000000000000000 ) ;
#33950 = CARTESIAN_POINT ( 'NONE',  ( 2.887291949543890457, -32.75603725470723759, 7.652160403243384756 ) ) ;
#33951 = CARTESIAN_POINT ( 'NONE',  ( 0.9852593961805760081, -32.99344650311874716, 7.766640943994643109 ) ) ;
#33952 = CARTESIAN_POINT ( 'NONE',  ( 81.01997673013200085, 63.86331202395269457, 3.456914256421384835 ) ) ;
#33953 = CARTESIAN_POINT ( 'NONE',  ( 85.30740962031771346, 1.871039318281703334, 5.038373847784950676 ) ) ;
#33954 = LINE ( 'NONE', #37011, #27273 ) ;
#33955 = ORIENTED_EDGE ( 'NONE', *, *, #27641, .T. ) ;
#33956 = CARTESIAN_POINT ( 'NONE',  ( -24.24874870218063450, -26.64985754041175525, 6.800000000000000711 ) ) ;
#33957 = CARTESIAN_POINT ( 'NONE',  ( 3.463827299026049911, -26.66297573651074160, 6.874555630061442990 ) ) ;
#33958 = EDGE_CURVE ( 'NONE', #17250, #29646, #5670, .T. ) ;
#33959 = DIRECTION ( 'NONE',  ( 0.000000000000000000, 0.000000000000000000, 1.000000000000000000 ) ) ;
#33960 = CARTESIAN_POINT ( 'NONE',  ( 31.37632533542383229, -3.544562347629171661, -4.958508136961243373 ) ) ;
#33961 = CARTESIAN_POINT ( 'NONE',  ( 27.40457795791207829, 0.9565065509615210404, -4.483545191191414148 ) ) ;
#33962 = CARTESIAN_POINT ( 'NONE',  ( 11.29080664838498649, 1.564594260697056104E-15, 2.500000000000000000 ) ) ;
#33963 = CARTESIAN_POINT ( 'NONE',  ( -62.85318495816822093, 36.92099889189239548, 4.451173097142760327 ) ) ;
#33964 = EDGE_LOOP ( 'NONE', ( #2269, #16227, #950, #34080, #2476, #9038, #4526, #13574 ) ) ;
#33965 = CARTESIAN_POINT ( 'NONE',  ( 2.822174244762026607, -32.87228481168282457, 7.782861076432729952 ) ) ;
#33966 = CARTESIAN_POINT ( 'NONE',  ( 86.40868413783579172, 1.299389369533768379, 4.865112849554557251 ) ) ;
#33967 = ADVANCED_FACE ( 'NONE', ( #4847 ), #8533, .T. ) ;
#33968 = ORIENTED_EDGE ( 'NONE', *, *, #4732, .T. ) ;
#33969 = VERTEX_POINT ( 'NONE', #7929 ) ;
#33971 = CARTESIAN_POINT ( 'NONE',  ( 35.83279683802916082, -3.732019870312798027, 5.621828468275774426 ) ) ;
#33970 = CARTESIAN_POINT ( 'NONE',  ( 79.60946285158563285, 65.60230831631015747, -2.836177733672711643 ) ) ;
#33972 = CARTESIAN_POINT ( 'NONE',  ( -1.321941654078521378, -31.33501114731328130, 7.749999999999999112 ) ) ;
#33973 = CARTESIAN_POINT ( 'NONE',  ( 22.05244047626662862, -2.652259403379859215, 3.648214695246499772 ) ) ;
#33974 = CARTESIAN_POINT ( 'NONE',  ( -8.878675913592189772, -26.64985754041175525, 6.800000000000000711 ) ) ;
#33975 = FACE_OUTER_BOUND ( 'NONE', #34949, .T. ) ;
#33976 = ORIENTED_EDGE ( 'NONE', *, *, #19629, .F. ) ;
#33977 = CARTESIAN_POINT ( 'NONE',  ( -1.741975392120745258, -30.20250733242332331, 7.651421919295148477 ) ) ;
#33978 = ORIENTED_EDGE ( 'NONE', *, *, #2237, .F. ) ;
#33979 = VERTEX_POINT ( 'NONE', #27080 ) ;
#33980 = LINE ( 'NONE', #30678, #35832 ) ;
#33981 = CARTESIAN_POINT ( 'NONE',  ( 80.36137575039693104, 63.90592395025429795, -3.640670270625565585 ) ) ;
#33982 = COLOUR_RGB ( '',0.7921568627450980005, 0.8196078431372548767, 0.9333333333333333481 ) ;
#33983 = CARTESIAN_POINT ( 'NONE',  ( 14.77209256136291238, -5.161470997039804054, 2.500001702421898564 ) ) ;
#33984 = ORIENTED_EDGE ( 'NONE', *, *, #12366, .T. ) ;
#33986 = CARTESIAN_POINT ( 'NONE',  ( 31.35344415347196545, 0.5184038160239171633, 4.590894038415813228 ) ) ;
#33985 = CARTESIAN_POINT ( 'NONE',  ( 21.85013245281674799, 2.795871195627560368, 5.288339663639888499 ) ) ;
#33987 = ORIENTED_EDGE ( 'NONE', *, *, #5582, .F. ) ;
#33988 = AXIS2_PLACEMENT_3D ( 'NONE', #1084, #19604, #34868 ) ;
#33989 = CARTESIAN_POINT ( 'NONE',  ( 81.48599817137666435, 65.27445208842044622, -2.474249079299299048 ) ) ;
#33990 = CARTESIAN_POINT ( 'NONE',  ( -71.19182660343213342, -21.78270726315146888, 4.000000000152813762 ) ) ;
#33991 = ORIENTED_EDGE ( 'NONE', *, *, #32681, .F. ) ;
#33992 = LINE ( 'NONE', #18305, #24561 ) ;
#33993 = DIRECTION ( 'NONE',  ( -0.9848077530122067991, -0.1736481776669374644, -0.000000000000000000 ) ) ;
#33994 = CARTESIAN_POINT ( 'NONE',  ( 72.66268786488812736, 61.76016136843576021, 3.552420216958366517 ) ) ;
#33995 = ADVANCED_FACE ( 'NONE', ( #26679 ), #20479, .F. ) ;
#33996 = CARTESIAN_POINT ( 'NONE',  ( 23.68553352910465648, 3.075504613652856989, -3.816384475219152694 ) ) ;
#33997 = ORIENTED_EDGE ( 'NONE', *, *, #26909, .F. ) ;
#33998 = CARTESIAN_POINT ( 'NONE',  ( 2.896981936218417264, -32.75240845689362601, 7.695279973900954751 ) ) ;
#33999 = CARTESIAN_POINT ( 'NONE',  ( 21.85643539959779957, 4.362886173974390935, 14.46802226367788791 ) ) ;
#34000 = CARTESIAN_POINT ( 'NONE',  ( -62.92837670882109080, -52.49535338866469658, 6.000000000000000000 ) ) ;
#34001 = ORIENTED_EDGE ( 'NONE', *, *, #21184, .T. ) ;
#34002 = CARTESIAN_POINT ( 'NONE',  ( -4.890026461918814071, -8.228598103685714525E-16, 6.000000000000000000 ) ) ;
#34003 = ORIENTED_EDGE ( 'NONE', *, *, #19158, .F. ) ;
#34004 = CARTESIAN_POINT ( 'NONE',  ( 79.11601629524611212, 66.18432715369991115, 1.588372325568262688 ) ) ;
#34005 = CARTESIAN_POINT ( 'NONE',  ( 88.39837738899358044, -0.9355285267052176890, 2.786041992172542336 ) ) ;
#34006 = DIRECTION ( 'NONE',  ( 0.000000000000000000, -1.000000000000000000, 0.000000000000000000 ) ) ;
#34007 = EDGE_CURVE ( 'NONE', #33558, #15366, #23973, .T. ) ;
#34008 = ADVANCED_FACE ( 'NONE', ( #2398 ), #33484, .F. ) ;
#34009 = CARTESIAN_POINT ( 'NONE',  ( 3.558396595903837056, -26.60381962644626697, 7.750000000000000888 ) ) ;
#34010 = CARTESIAN_POINT ( 'NONE',  ( 14.89216304183951678, -6.126272768353560494, 2.529875904917741725 ) ) ;
#34011 = CARTESIAN_POINT ( 'NONE',  ( -25.07867591359219617, -26.64985754041175525, 6.800000000000000711 ) ) ;
#34012 = CARTESIAN_POINT ( 'NONE',  ( 31.72030731019543381, -0.5546557356656219850, -5.157119132924021798 ) ) ;
#34013 = CARTESIAN_POINT ( 'NONE',  ( 5.100210461593464473, -29.53486150151830358, 7.711434774245209844 ) ) ;
#34014 = CARTESIAN_POINT ( 'NONE',  ( 4.643065655508351597, -31.46483401609519959, 6.895394898881657575 ) ) ;
#34015 = CIRCLE ( 'NONE', #31359, 10.99999999999998224 ) ;
#34016 = ORIENTED_EDGE ( 'NONE', *, *, #24736, .F. ) ;
#34017 = DIRECTION ( 'NONE',  ( 0.000000000000000000, -1.000000000000000000, 0.000000000000000000 ) ) ;
#34018 = AXIS2_PLACEMENT_3D ( 'NONE', #18936, #5971, #21825 ) ;
#34019 = CARTESIAN_POINT ( 'NONE',  ( 4.314359296880712513, -31.88662353291251605, 7.776484688137386136 ) ) ;
#34020 = LINE ( 'NONE', #40358, #2028 ) ;
#34021 = EDGE_CURVE ( 'NONE', #27835, #15467, #21901, .T. ) ;
#34022 = ORIENTED_EDGE ( 'NONE', *, *, #25634, .T. ) ;
#34023 = CARTESIAN_POINT ( 'NONE',  ( 36.82361487772457309, -2.161144939959093403, 5.895778257769980435 ) ) ;
#34024 = B_SPLINE_CURVE_WITH_KNOTS ( 'NONE', 3,
 ( #24450, #14981, #33950, #11262, #14361, #33122, #36403, #8383, #33334, #21371 ),
 .UNSPECIFIED., .F., .F.,
 ( 4, 3, 3, 4 ),
 ( 0.000000000000000000, 3.025570593003025599E-05, 6.051145698343885989E-05, 6.468151674593503617E-05 ),
 .UNSPECIFIED. ) ;
#34025 = DIRECTION ( 'NONE',  ( 1.000000000000000000, 0.000000000000000000, 0.000000000000000000 ) ) ;
#34026 = CARTESIAN_POINT ( 'NONE',  ( 66.86920591220189181, 57.92326096844472261, -3.999524142429984330 ) ) ;
#34027 = CARTESIAN_POINT ( 'NONE',  ( -1.339436964189177459, -27.83515215944516896, 7.640616322432101981 ) ) ;
#34028 = ORIENTED_EDGE ( 'NONE', *, *, #34393, .T. ) ;
#34029 = CARTESIAN_POINT ( 'NONE',  ( -0.4661178359761078416, -32.19028865001026674, 7.740055089680395461 ) ) ;
#34030 = CARTESIAN_POINT ( 'NONE',  ( -76.57843430598849466, -5.832456142219742290, -8.260218182170147472 ) ) ;
#34031 = LINE ( 'NONE', #18342, #29903 ) ;
#34032 = ORIENTED_EDGE ( 'NONE', *, *, #730, .T. ) ;
#34033 = CARTESIAN_POINT ( 'NONE',  ( -44.23414840393349579, -30.38627270959228710, 6.800000000000000711 ) ) ;
#34034 = DIRECTION ( 'NONE',  ( 1.000000000000000000, 0.000000000000000000, 0.000000000000000000 ) ) ;
#34035 = ORIENTED_EDGE ( 'NONE', *, *, #34324, .F. ) ;
#34036 = CARTESIAN_POINT ( 'NONE',  ( 22.00772085900330666, 5.524290953573272489, 3.138816991787310773 ) ) ;
#34037 = CARTESIAN_POINT ( 'NONE',  ( 82.53033050081239708, 64.25366301186836893, -1.000000000000000000 ) ) ;
#34038 = ADVANCED_FACE ( 'NONE', ( #17794 ), #17380, .F. ) ;
#34039 = CARTESIAN_POINT ( 'NONE',  ( 81.06760980982291187, 61.95377044681377043, 2.747716423863114876 ) ) ;
#34040 = DIRECTION ( 'NONE',  ( -0.4690749385695657803, -0.8831583674551003460, 0.000000000000000000 ) ) ;
#34041 = ORIENTED_EDGE ( 'NONE', *, *, #33332, .F. ) ;
#34042 = CARTESIAN_POINT ( 'NONE',  ( 76.89779646338293162, 61.47851784853094870, -3.801074476324162177 ) ) ;
#34044 = DIRECTION ( 'NONE',  ( 0.000000000000000000, 0.000000000000000000, 1.000000000000000000 ) ) ;
#34043 = CARTESIAN_POINT ( 'NONE',  ( -72.35143257368834213, -46.63264610307073355, 5.828929736913487147 ) ) ;
#34045 = DIRECTION ( 'NONE',  ( 0.5751513419797913418, 0.4826092789263654037, 0.6605219282605377940 ) ) ;
#34046 = VECTOR ( 'NONE', #18240, 1000.000000000000000 ) ;
#34047 = CARTESIAN_POINT ( 'NONE',  ( 79.37811825733845694, 65.99825290327332539, -2.263370276487070232 ) ) ;
#34048 = CARTESIAN_POINT ( 'NONE',  ( 78.55649010480104266, 62.41317512920507937, 3.780406938340867384 ) ) ;
#34049 = CIRCLE ( 'NONE', #20843, 4.250000000000000000 ) ;
#34050 = ORIENTED_EDGE ( 'NONE', *, *, #8105, .T. ) ;
#34051 = AXIS2_PLACEMENT_3D ( 'NONE', #38665, #35416, #29420 ) ;
#34052 = DIRECTION ( 'NONE',  ( -1.000000000000000000, 0.000000000000000000, 0.000000000000000000 ) ) ;
#34053 = CARTESIAN_POINT ( 'NONE',  ( 79.28422506984799156, 66.27750502035060265, 1.322881339814630408 ) ) ;
#34056 = ORIENTED_EDGE ( 'NONE', *, *, #37467, .F. ) ;
#34055 = CARTESIAN_POINT ( 'NONE',  ( -1.576062547484235354, -30.80072589882973944, 7.695279973900954751 ) ) ;
#34054 = CARTESIAN_POINT ( 'NONE',  ( 4.279759429550099803, -31.93571510856349605, 6.880828092187097234 ) ) ;
#34057 = CARTESIAN_POINT ( 'NONE',  ( 31.05604276399450114, -2.500009215535430762, 5.784057531382419626 ) ) ;
#34058 = EDGE_CURVE ( 'NONE', #36741, #35883, #24477, .T. ) ;
#34059 = DIRECTION ( 'NONE',  ( 1.000000000000000000, 0.000000000000000000, 0.000000000000000000 ) ) ;
#34060 = CARTESIAN_POINT ( 'NONE',  ( -64.78745217040227544, 34.77601383833187043, 6.355070236019812135 ) ) ;
#34061 = CARTESIAN_POINT ( 'NONE',  ( 22.31500143320247531, 0.2710179362157456029, -7.066509127937782075 ) ) ;
#34062 = ADVANCED_FACE ( 'NONE', ( #7033 ), #6279, .F. ) ;
#34063 = DIRECTION ( 'NONE',  ( 1.000000000000000000, 0.000000000000000000, 0.000000000000000000 ) ) ;
#34064 = DIRECTION ( 'NONE',  ( -0.000000000000000000, -0.000000000000000000, -1.000000000000000000 ) ) ;
#34065 = CARTESIAN_POINT ( 'NONE',  ( -4.448748702180642667, -25.49307895267003587, 6.700000000000000178 ) ) ;
#34066 = LINE ( 'NONE', #33455, #2586 ) ;
#34067 = CARTESIAN_POINT ( 'NONE',  ( 34.57554517587881548, -0.8971683385966218172, -5.398457213048259540 ) ) ;
#34068 = CARTESIAN_POINT ( 'NONE',  ( 3.439957088343224889, -32.60061551843173078, 7.773839561854630986 ) ) ;
#34069 = LINE ( 'NONE', #30968, #12388 ) ;
#34070 = FACE_OUTER_BOUND ( 'NONE', #26766, .T. ) ;
#34071 = CARTESIAN_POINT ( 'NONE',  ( 8.290806648384990041, -25.50263309590217276, -2.499999999999998668 ) ) ;
#34072 = FACE_OUTER_BOUND ( 'NONE', #1870, .T. ) ;
#34073 = CARTESIAN_POINT ( 'NONE',  ( -73.47413635169593249, 5.573843681890572554, 10.88137847971116123 ) ) ;
#34074 = EDGE_CURVE ( 'NONE', #26564, #30447, #25982, .T. ) ;
#34075 = ADVANCED_FACE ( 'NONE', ( #12240 ), #19603, .F. ) ;
#34076 = FACE_OUTER_BOUND ( 'NONE', #9607, .T. ) ;
#34077 = CARTESIAN_POINT ( 'NONE',  ( 14.74026921260515088, -4.699362955988203083, -2.506077451199989703 ) ) ;
#34078 = CARTESIAN_POINT ( 'NONE',  ( 23.26251525840845957, 2.275869519923719331, -4.593821674871367833 ) ) ;
#34079 = ORIENTED_EDGE ( 'NONE', *, *, #24940, .T. ) ;
#34080 = ORIENTED_EDGE ( 'NONE', *, *, #19261, .T. ) ;
#34081 = CARTESIAN_POINT ( 'NONE',  ( 4.629538257087431496, -31.49813288122227917, 7.387053503561886281 ) ) ;
#34082 = VECTOR ( 'NONE', #16466, 1000.000000000000000 ) ;
#34083 = CARTESIAN_POINT ( 'NONE',  ( 69.57837460818548436, 59.54477471642375974, -3.931953536312648989 ) ) ;
#34084 = ORIENTED_EDGE ( 'NONE', *, *, #18112, .T. ) ;
#34085 = CARTESIAN_POINT ( 'NONE',  ( 86.62140889132389532, -0.8164050916001737157, 5.580443680875508683 ) ) ;
#34086 = DIRECTION ( 'NONE',  ( 0.8660254037844380415, 0.5000000000000011102, 0.000000000000000000 ) ) ;
#34087 = CARTESIAN_POINT ( 'NONE',  ( 2.979782760284078513, -26.41980900443600078, 6.863904403958576594 ) ) ;
#34088 = CARTESIAN_POINT ( 'NONE',  ( 1.182707065140680358, -26.20955829661496850, 6.874555630061442990 ) ) ;
#34089 = CARTESIAN_POINT ( 'NONE',  ( 5.054583831487962975, -30.12615907168387608, 7.712764235869103757 ) ) ;
#34090 = ORIENTED_EDGE ( 'NONE', *, *, #31234, .F. ) ;
#34091 = CARTESIAN_POINT ( 'NONE',  ( 21.70978835544913110, 6.347857807235328664, 3.186345948389122551 ) ) ;
#34092 = CARTESIAN_POINT ( 'NONE',  ( 5.741588806061445283, -32.80189416861090024, 7.754798119455333705 ) ) ;
#34093 = ORIENTED_EDGE ( 'NONE', *, *, #35409, .T. ) ;
#34094 = ORIENTED_EDGE ( 'NONE', *, *, #16842, .F. ) ;
#34095 = CARTESIAN_POINT ( 'NONE',  ( 79.80332398823145468, 63.27387486779120707, -3.741985197832890186 ) ) ;
#34096 = AXIS2_PLACEMENT_3D ( 'NONE', #4260, #10611, #13511 ) ;
#34097 = CARTESIAN_POINT ( 'NONE',  ( 17.47038219521028779, 11.99840016206135118, -2.499999999999995115 ) ) ;
#34098 = CARTESIAN_POINT ( 'NONE',  ( 81.04721337197098308, 65.04274187704037047, -3.019849704269078394 ) ) ;
#34099 = VERTEX_POINT ( 'NONE', #875 ) ;
#34100 = ADVANCED_FACE ( 'NONE', ( #13407, #35463 ), #15126, .T. ) ;
#34101 = VECTOR ( 'NONE', #4668, 1000.000000000000000 ) ;
#34102 = CARTESIAN_POINT ( 'NONE',  ( 6.117106422890660866, -32.35436969967226162, 6.954324564059724878 ) ) ;
#34103 = ADVANCED_FACE ( 'NONE', ( #15329 ), #40238, .T. ) ;
#34104 = CARTESIAN_POINT ( 'NONE',  ( 2.886433127740331894, -32.75636032089741434, 7.740055089680400791 ) ) ;
#34105 = CARTESIAN_POINT ( 'NONE',  ( 22.71767909661236118, -4.608197067329504293, -7.212190040765698917 ) ) ;
#34106 = ORIENTED_EDGE ( 'NONE', *, *, #22375, .F. ) ;
#34107 = CARTESIAN_POINT ( 'NONE',  ( -72.90053700259019820, 3.429967363124852842, 10.95643088971294965 ) ) ;
#34108 = CARTESIAN_POINT ( 'NONE',  ( 37.19556178435423277, -2.859567876585734414, 6.000000005145950333 ) ) ;
#34109 = EDGE_CURVE ( 'NONE', #4930, #38778, #5877, .T. ) ;
#34110 = CIRCLE ( 'NONE', #3874, 6.000000000000005329 ) ;
#34111 = CARTESIAN_POINT ( 'NONE',  ( -1.323924960262854666, -31.33161076090960151, 7.635761828346577573 ) ) ;
#34112 = EDGE_CURVE ( 'NONE', #19965, #11431, #37154, .T. ) ;
#34113 = CARTESIAN_POINT ( 'NONE',  ( -80.35180597995123719, 11.50364652777614971, -3.371254867381904496 ) ) ;
#34114 = CARTESIAN_POINT ( 'NONE',  ( 3.425221786318646267, -26.52444900129300720, 7.730015791551944737 ) ) ;
#34115 = CARTESIAN_POINT ( 'NONE',  ( 37.00845883712383966, -3.246107522403217427, -5.947038319129071660 ) ) ;
#34116 = CARTESIAN_POINT ( 'NONE',  ( -1.740187722448509389, -30.14826187258440626, 7.781480525794718162 ) ) ;
#34117 = CARTESIAN_POINT ( 'NONE',  ( 14.71143272272386326, 12.53673232395533965, 2.502472892362715307 ) ) ;
#34118 = DIRECTION ( 'NONE',  ( -0.000000000000000000, -0.000000000000000000, 1.000000000000000000 ) ) ;
#34119 = CARTESIAN_POINT ( 'NONE',  ( 29.51619774652193229, -3.826605600177332089, 4.386877048897818376 ) ) ;
#34120 = CARTESIAN_POINT ( 'NONE',  ( -6.448748702180637338, -26.64985754041175525, 6.700000000000000178 ) ) ;
#34121 = CARTESIAN_POINT ( 'NONE',  ( 2.120505722696732764, -33.04462681987888573, 6.931070083220556732 ) ) ;
#34122 = CARTESIAN_POINT ( 'NONE',  ( -70.40641634670110705, 0.1089831108692859846, 3.980161455439681806 ) ) ;
#34123 = CARTESIAN_POINT ( 'NONE',  ( 1.062037487868057184, -33.01122440958558002, 6.894806418505347700 ) ) ;
#34124 = CLOSED_SHELL ( 'NONE', ( #809, #29993, #14500, #7085, #21073, #11002 ) ) ;
#34125 = CARTESIAN_POINT ( 'NONE',  ( 24.55513722008589639, 2.975329870594148218, -3.595293232472362988 ) ) ;
#34126 = ORIENTED_EDGE ( 'NONE', *, *, #30499, .F. ) ;
#34127 = VECTOR ( 'NONE', #20239, 1000.000000000000000 ) ;
#34128 = CARTESIAN_POINT ( 'NONE',  ( 67.44728384595320847, 58.15801736331750504, 3.998402061830689025 ) ) ;
#34129 = CARTESIAN_POINT ( 'NONE',  ( 35.33527427362074746, -3.300844520036612995, 5.721322155873344251 ) ) ;
#34130 = CARTESIAN_POINT ( 'NONE',  ( 0.9267304714826125611, -25.86893018339336692, 7.013842709614101167 ) ) ;
#34131 = LINE ( 'NONE', #6720, #35887 ) ;
#34132 = CARTESIAN_POINT ( 'NONE',  ( 87.57592060778061693, -0.6244806207018304134, 5.359096402341661403 ) ) ;
#34134 = CARTESIAN_POINT ( 'NONE',  ( -71.92837670882107659, -23.80776546975053520, 9.949874371066204759 ) ) ;
#34133 = CYLINDRICAL_SURFACE ( 'NONE', #4446, 0.1000000000000028644 ) ;
#34135 = CARTESIAN_POINT ( 'NONE',  ( -1.549552128476125112, -30.56886739641119632, 6.882085323592688653 ) ) ;
#34136 = ORIENTED_EDGE ( 'NONE', *, *, #22706, .F. ) ;
#34137 = CARTESIAN_POINT ( 'NONE',  ( 24.63732103174290700, 2.685245520235881589, 3.901802067749889691 ) ) ;
#34138 = B_SPLINE_CURVE_WITH_KNOTS ( 'NONE', 3,
 ( #11785, #27457, #33657, #30145, #23948, #2369, #34073, #5848, #14888, #24366, #2778, #36929, #27856, #8708, #25188, #10131, #37528, #6662, #6862, #34888, #28475, #31988, #25394, #19214, #25797, #37933, #35086, #22718, #13231, #9742, #22319, #31778 ),
 .UNSPECIFIED., .F., .F.,
 ( 4, 2, 2, 2, 2, 2, 2, 2, 2, 2, 2, 2, 2, 2, 2, 4 ),
 ( 0.06009542766246023932, 0.06130746216911493740, 0.06251949667576962855, 0.06373153118242433357, 0.06494356568907902472, 0.06615560019573371586, 0.06676161744906104756, 0.06736763470238837925, 0.06857966920904304264, 0.06918568646237036046, 0.06979170371569767828, 0.07221577272900697730, 0.07463984174231627633, 0.07585187624897093972, 0.07706391075562560311, 0.07948797976893491601 ),
 .UNSPECIFIED. ) ;
#34139 = CARTESIAN_POINT ( 'NONE',  ( -62.92837670882106238, -23.80776546975053520, -6.000000000000000000 ) ) ;
#34140 = VECTOR ( 'NONE', #17503, 1000.000000000000000 ) ;
#34141 = ORIENTED_EDGE ( 'NONE', *, *, #2780, .F. ) ;
#34142 = PLANE ( 'NONE',  #29348 ) ;
#34143 = UNCERTAINTY_MEASURE_WITH_UNIT (LENGTH_MEASURE( 1.000000000000000082E-05 ), #37895, 'distance_accuracy_value', 'NONE');
#34144 = ORIENTED_EDGE ( 'NONE', *, *, #10304, .T. ) ;
#34145 = ORIENTED_EDGE ( 'NONE', *, *, #13562, .T. ) ;
#34146 = CARTESIAN_POINT ( 'NONE',  ( 79.88758398535436811, 64.02175723273457209, -3.702313260098205383 ) ) ;
#34147 = DIRECTION ( 'NONE',  ( 0.000000000000000000, 0.000000000000000000, -1.000000000000000000 ) ) ;
#34148 = CARTESIAN_POINT ( 'NONE',  ( 80.97211960314545820, 61.55694294823971546, 2.294512580621449693 ) ) ;
#34150 = ORIENTED_EDGE ( 'NONE', *, *, #18659, .F. ) ;
#34149 = CARTESIAN_POINT ( 'NONE',  ( -1.343166177233030556, -31.08544090138337168, 6.939395833800438673 ) ) ;
#34151 = CARTESIAN_POINT ( 'NONE',  ( 73.79885669521775071, 60.72590704978823339, -3.935025356184053802 ) ) ;
#34152 = DIRECTION ( 'NONE',  ( 0.000000000000000000, 0.000000000000000000, 1.000000000000000000 ) ) ;
#34154 = DIRECTION ( 'NONE',  ( -0.000000000000000000, -0.000000000000000000, -1.000000000000000000 ) ) ;
#34153 = DIRECTION ( 'NONE',  ( -0.000000000000000000, -0.000000000000000000, 1.000000000000000000 ) ) ;
#34155 = DIRECTION ( 'NONE',  ( -0.000000000000000000, -0.000000000000000000, 1.000000000000000000 ) ) ;
#34156 = CARTESIAN_POINT ( 'NONE',  ( -4.448748702180642667, -26.64985754041175525, 6.700000000000000178 ) ) ;
#34157 = CARTESIAN_POINT ( 'NONE',  ( 21.88600830960537635, 5.632864204250798146, -3.275930472131208138 ) ) ;
#34158 = EDGE_LOOP ( 'NONE', ( #37454, #11541, #7609, #15372, #26861 ) ) ;
#34159 = DIRECTION ( 'NONE',  ( -1.000000000000000000, 0.000000000000000000, 0.000000000000000000 ) ) ;
#34160 = ADVANCED_FACE ( 'NONE', ( #27884 ), #7683, .T. ) ;
#34161 = EDGE_CURVE ( 'NONE', #35515, #10191, #17483, .T. ) ;
#34162 = CARTESIAN_POINT ( 'NONE',  ( 25.28494853283190125, -3.333630280469910723, 5.108382079771137008 ) ) ;
#34163 = EDGE_CURVE ( 'NONE', #23072, #33660, #39526, .T. ) ;
#34164 = CARTESIAN_POINT ( 'NONE',  ( -77.39670385617056070, -6.181659773469543318, -7.628895083485716988 ) ) ;
#34165 = LINE ( 'NONE', #21994, #503 ) ;
#34166 = CARTESIAN_POINT ( 'NONE',  ( 81.42847900441165621, 61.86412877313431125, 2.316472630215899109 ) ) ;
#34167 = CARTESIAN_POINT ( 'NONE',  ( 88.38642666631945133, -2.374919807968325358, 0.2172961577596721761 ) ) ;
#34168 = CARTESIAN_POINT ( 'NONE',  ( -74.92283640148282586, 18.87330372387140187, -12.49999999999999645 ) ) ;
#34169 = ORIENTED_EDGE ( 'NONE', *, *, #16447, .F. ) ;
#34170 = CARTESIAN_POINT ( 'NONE',  ( -64.08758708074093136, 36.14363715547680300, -3.800414904976364028 ) ) ;
#34171 = CARTESIAN_POINT ( 'NONE',  ( 4.603808887335269162, -31.33918005375042171, 7.782034975670476307 ) ) ;
#34172 = VECTOR ( 'NONE', #26799, 1000.000000000000114 ) ;
#34173 = CARTESIAN_POINT ( 'NONE',  ( 3.998933749712821673, -26.93046473555785170, 6.870737987065013819 ) ) ;
#34174 = LINE ( 'NONE', #18275, #14909 ) ;
#34175 = FACE_OUTER_BOUND ( 'NONE', #14106, .T. ) ;
#34176 = CARTESIAN_POINT ( 'NONE',  ( -0.4083080382643015649, -26.90281974977018109, 7.774064877406530627 ) ) ;
#34177 = CARTESIAN_POINT ( 'NONE',  ( 35.78607896117043197, -3.162280031239083744, 5.791681130117677156 ) ) ;
#34178 = CARTESIAN_POINT ( 'NONE',  ( 4.272324738573828107, -31.79372274477328020, 7.785868773668302545 ) ) ;
#34179 = CARTESIAN_POINT ( 'NONE',  ( 85.24855023725586989, 2.602506829941634514, 1.762177041774413588 ) ) ;
#34180 = VECTOR ( 'NONE', #17289, 1000.000000000000000 ) ;
#34181 = ORIENTED_EDGE ( 'NONE', *, *, #15379, .F. ) ;
#34183 = LINE ( 'NONE', #31481, #27032 ) ;
#34182 = CARTESIAN_POINT ( 'NONE',  ( 80.64987221081615587, 64.05646366546658044, -3.549391953833852753 ) ) ;
#34184 = DIRECTION ( 'NONE',  ( 0.000000000000000000, 1.000000000000000000, 0.000000000000000000 ) ) ;
#34185 = FACE_OUTER_BOUND ( 'NONE', #2217, .T. ) ;
#34186 = ORIENTED_EDGE ( 'NONE', *, *, #24600, .T. ) ;
#34187 = CARTESIAN_POINT ( 'NONE',  ( -1.650167670790918750, -28.99217783630842860, 7.756377446753162097 ) ) ;
#34188 = CARTESIAN_POINT ( 'NONE',  ( -0.4585365243479023190, -26.81617090910717494, 7.761113333117548585 ) ) ;
#34189 = ORIENTED_EDGE ( 'NONE', *, *, #8071, .F. ) ;
#34190 = ORIENTED_EDGE ( 'NONE', *, *, #20828, .F. ) ;
#34191 = CARTESIAN_POINT ( 'NONE',  ( 80.99721608130789718, 62.45573281339171956, -3.163072811751558522 ) ) ;
#34192 = CARTESIAN_POINT ( 'NONE',  ( -58.44033895488188790, 28.22358054771053304, -5.330345403092615619 ) ) ;
#34193 = ORIENTED_EDGE ( 'NONE', *, *, #2836, .T. ) ;
#34195 = CARTESIAN_POINT ( 'NONE',  ( 14.73500979046644233, 12.83520685450635490, 2.502377855999189826 ) ) ;
#34194 = CARTESIAN_POINT ( 'NONE',  ( 21.85329537605191419, 3.009163427712417960, 5.104443796496481944 ) ) ;
#34196 = CARTESIAN_POINT ( 'NONE',  ( 79.78161832376089535, 66.22496747522383487, -1.859759604987000658 ) ) ;
#34197 = AXIS2_PLACEMENT_3D ( 'NONE', #10282, #26150, #37523 ) ;
#34198 = CARTESIAN_POINT ( 'NONE',  ( -71.92837670882107659, -20.78299143688747819, 3.916079783099621014 ) ) ;
#34199 = ORIENTED_EDGE ( 'NONE', *, *, #19594, .F. ) ;
#34201 = CARTESIAN_POINT ( 'NONE',  ( -1.499157785959173594, -28.41975916621540321, 7.635761828346577573 ) ) ;
#34200 = FACE_OUTER_BOUND ( 'NONE', #54, .T. ) ;
#34202 = CARTESIAN_POINT ( 'NONE',  ( 3.751251297819363728, -25.49307895267003587, 6.800000000000000711 ) ) ;
#34203 = CARTESIAN_POINT ( 'NONE',  ( -41.07867591359219972, -26.64985754041175525, 6.700000000000000178 ) ) ;
#34204 = CARTESIAN_POINT ( 'NONE',  ( 73.62310697524999625, 61.12246817794784448, 3.899931323576833808 ) ) ;
#34205 = VERTEX_POINT ( 'NONE', #7638 ) ;
#34206 = CARTESIAN_POINT ( 'NONE',  ( 23.48457729831129726, 3.066923110525566543, -3.897436638742564963 ) ) ;
#34207 = VERTEX_POINT ( 'NONE', #23095 ) ;
#34208 = CARTESIAN_POINT ( 'NONE',  ( 21.85643539959776760, -0.9922589305345951294, -16.01828770219436393 ) ) ;
#34210 = EDGE_CURVE ( 'NONE', #9655, #33400, #8026, .T. ) ;
#34209 = CARTESIAN_POINT ( 'NONE',  ( -6.878675913592188884, -24.55319635012989110, 6.700000000000000178 ) ) ;
#34211 = ORIENTED_EDGE ( 'NONE', *, *, #21442, .T. ) ;
#34212 = CARTESIAN_POINT ( 'NONE',  ( -54.81017820351302561, 31.50178459264590103, -1.053924518346901706 ) ) ;
#34213 = CARTESIAN_POINT ( 'NONE',  ( 79.31479573854763032, 66.13045663638733629, 1.878604182848667037 ) ) ;
#34214 = CARTESIAN_POINT ( 'NONE',  ( 87.87162303905448368, -0.3438530395839958231, 3.959040383187740542 ) ) ;
#34215 = ORIENTED_EDGE ( 'NONE', *, *, #22056, .F. ) ;
#34216 = CARTESIAN_POINT ( 'NONE',  ( -62.14171895907916365, -49.48408358960642062, -4.951123000344130887 ) ) ;
#34217 = B_SPLINE_CURVE_WITH_KNOTS ( 'NONE', 3,
 ( #19439, #34304, #27880, #31193, #21721, #25011, #31395, #37958, #312, #18606 ),
 .UNSPECIFIED., .F., .F.,
 ( 4, 3, 3, 4 ),
 ( 1.748223473168675632E-18, 3.025570593003025938E-05, 6.051145698343942910E-05, 6.468151674593380289E-05 ),
 .UNSPECIFIED. ) ;
#34218 = CARTESIAN_POINT ( 'NONE',  ( 2.768830974701133485, -32.90287465194062833, 6.870724624169667116 ) ) ;
#34219 = CARTESIAN_POINT ( 'NONE',  ( 15.11041258174173407, -4.075176119877783165, 2.561837290471254303 ) ) ;
#34220 = CARTESIAN_POINT ( 'NONE',  ( 24.75830837035764276, 3.019210359990082804, 3.350572556515618583 ) ) ;
#34221 = CARTESIAN_POINT ( 'NONE',  ( 36.63352589858980224, -3.080950350379837666, -5.923945720283577465 ) ) ;
#34222 = CARTESIAN_POINT ( 'NONE',  ( 5.100381899876085257, -29.58108672504286574, 7.775108481317161591 ) ) ;
#34223 = DIRECTION ( 'NONE',  ( 0.4999999999999977240, 0.000000000000000000, -0.8660254037844399289 ) ) ;
#34224 = CARTESIAN_POINT ( 'NONE',  ( -0.9575113486053222767, -31.84711263666175540, 7.695279973900954751 ) ) ;
#34225 = DIRECTION ( 'NONE',  ( 1.000000000000000000, 0.000000000000000000, 0.000000000000000000 ) ) ;
#34226 = CARTESIAN_POINT ( 'NONE',  ( 2.170460981197068762, -32.93727830324805694, 7.754798119455333705 ) ) ;
#34227 = ORIENTED_EDGE ( 'NONE', *, *, #4584, .T. ) ;
#34228 = ORIENTED_EDGE ( 'NONE', *, *, #117, .F. ) ;
#34229 = CARTESIAN_POINT ( 'NONE',  ( 37.08862871230790148, -2.428037328474826229, 5.958176329106160019 ) ) ;
#34230 = DIRECTION ( 'NONE',  ( 1.000000000000000000, 0.000000000000000000, 0.000000000000000000 ) ) ;
#34231 = EDGE_LOOP ( 'NONE', ( #7979, #6027, #21839, #8473 ) ) ;
#34232 = EDGE_CURVE ( 'NONE', #2601, #26604, #32773, .T. ) ;
#34233 = CARTESIAN_POINT ( 'NONE',  ( -0.5003730563773006734, -26.86726130889041286, 7.785344483711591934 ) ) ;
#34234 = ORIENTED_EDGE ( 'NONE', *, *, #14880, .F. ) ;
#34235 = CARTESIAN_POINT ( 'NONE',  ( -88.78960668556791802, 4.298224710795182091, 15.50000000000000000 ) ) ;
#34236 = VECTOR ( 'NONE', #6094, 1000.000000000000000 ) ;
#34237 = CARTESIAN_POINT ( 'NONE',  ( -20.87867591359218977, -26.64985754041175525, 6.700000000000000178 ) ) ;
#34238 = PLANE ( 'NONE',  #8190 ) ;
#34239 = DIRECTION ( 'NONE',  ( -1.000000000000000000, 0.000000000000000000, 0.000000000000000000 ) ) ;
#34240 = CARTESIAN_POINT ( 'NONE',  ( 3.920970191082350453, -32.27530831286587443, 6.887161170156903545 ) ) ;
#34241 = VERTEX_POINT ( 'NONE', #20188 ) ;
#34242 = CARTESIAN_POINT ( 'NONE',  ( 22.00379729694733655, 5.541703127858326638, 3.130312335064352247 ) ) ;
#34243 = CARTESIAN_POINT ( 'NONE',  ( 81.73112818161179405, 61.68666564161350863, -1.174937739208586907 ) ) ;
#34244 = ADVANCED_FACE ( 'NONE', ( #29270 ), #26981, .F. ) ;
#34245 = CARTESIAN_POINT ( 'NONE',  ( 80.72665634072043872, 62.99526239489092205, 3.473545878414587396 ) ) ;
#34246 = CARTESIAN_POINT ( 'NONE',  ( -0.04376389210842144412, -32.48847997939775212, 6.892063359921934307 ) ) ;
#34247 = ORIENTED_EDGE ( 'NONE', *, *, #12160, .T. ) ;
#34248 = CARTESIAN_POINT ( 'NONE',  ( 76.72366484839760403, 61.84716987400894084, -3.872369636032548357 ) ) ;
#34250 = CARTESIAN_POINT ( 'NONE',  ( -70.92837670882107659, -27.85319909218681644, 0.000000000000000000 ) ) ;
#34249 = FACE_OUTER_BOUND ( 'NONE', #40474, .T. ) ;
#34251 = CARTESIAN_POINT ( 'NONE',  ( -1.699609906766908818, -29.56993018339339940, 6.949309202340325342 ) ) ;
#34252 = CARTESIAN_POINT ( 'NONE',  ( 81.46310422712103616, 61.87916883045149063, -2.296576099416859140 ) ) ;
#34253 = CARTESIAN_POINT ( 'NONE',  ( 78.10617727715707304, 63.31486359019603327, 3.780406938340841183 ) ) ;
#34254 = ORIENTED_EDGE ( 'NONE', *, *, #9339, .F. ) ;
#34255 = ORIENTED_EDGE ( 'NONE', *, *, #28267, .F. ) ;
#34256 = AXIS2_PLACEMENT_3D ( 'NONE', #5181, #8450, #14833 ) ;
#34257 = CARTESIAN_POINT ( 'NONE',  ( 4.741120993177593945, -31.30312249647428757, 7.643192810543818716 ) ) ;
#34259 = ADVANCED_FACE ( 'NONE', ( #4369 ), #32370, .F. ) ;
#34258 = CARTESIAN_POINT ( 'NONE',  ( -58.11978350796148618, 31.63118870160872120, 4.423684907992433857 ) ) ;
#34260 = CARTESIAN_POINT ( 'NONE',  ( 82.37993866337130555, 63.11845131094302985, 1.936735430445675421 ) ) ;
#34262 = CARTESIAN_POINT ( 'NONE',  ( -0.8725572984338751947, -27.34733221711291051, 6.894806418505345036 ) ) ;
#34261 = CARTESIAN_POINT ( 'NONE',  ( -64.08758708074093136, 41.64119180419724842, 2.960472586359419900 ) ) ;
#34263 = CARTESIAN_POINT ( 'NONE',  ( 29.24680661740138632, 2.095232292622827508, -1.948189103474716966 ) ) ;
#34264 = CARTESIAN_POINT ( 'NONE',  ( -1.353540684280711393, -31.27978037611249462, 6.880608371227950215 ) ) ;
#34265 = CARTESIAN_POINT ( 'NONE',  ( -62.89138254649398618, 35.56687702170635390, -5.951199099626548694 ) ) ;
#34266 = CARTESIAN_POINT ( 'NONE',  ( -64.35089310738592872, 36.57692748661052207, 5.628006413927832519 ) ) ;
#34267 = CARTESIAN_POINT ( 'NONE',  ( 23.60029590725254778, 0.4360417540011212734, -5.514987849079120430 ) ) ;
#34268 = CYLINDRICAL_SURFACE ( 'NONE', #20878, 0.09010775117053000660 ) ;
#34269 = VERTEX_POINT ( 'NONE', #23492 ) ;
#34270 = CYLINDRICAL_SURFACE ( 'NONE', #14499, 7.999999999999986677 ) ;
#34271 = CARTESIAN_POINT ( 'NONE',  ( -63.58520484588294153, 35.72026407271188475, -6.999999999999999112 ) ) ;
#34272 = VECTOR ( 'NONE', #30097, 1000.000000000000114 ) ;
#34273 = DIRECTION ( 'NONE',  ( -0.000000000000000000, -0.000000000000000000, 1.000000000000000000 ) ) ;
#34274 = CARTESIAN_POINT ( 'NONE',  ( 2.136987090091772235, -33.04259287893679442, 7.009310105710486738 ) ) ;
#34275 = CARTESIAN_POINT ( 'NONE',  ( 36.18514542968358683, -3.553240791427502820, -5.771079380064234599 ) ) ;
#34276 = CARTESIAN_POINT ( 'NONE',  ( 74.75251888580193338, 59.31330218054827697, -3.344918171298342457 ) ) ;
#34277 = DIRECTION ( 'NONE',  ( -0.000000000000000000, -1.000000000000000000, -0.000000000000000000 ) ) ;
#34278 = CARTESIAN_POINT ( 'NONE',  ( -17.27251170661583402, 0.7293679304675921848, 6.000000000000000000 ) ) ;
#34280 = CARTESIAN_POINT ( 'NONE',  ( -77.92837670882107659, 2.429809908903242555, 12.50000000000000000 ) ) ;
#34279 = B_SPLINE_CURVE_WITH_KNOTS ( 'NONE', 3,
 ( #15009, #39714, #352, #15976, #24480, #21198, #9598, #5347, #25262, #36837 ),
 .UNSPECIFIED., .F., .F.,
 ( 4, 3, 3, 4 ),
 ( 1.887418258779916733E-18, 3.025570593003297328E-05, 6.051145698344366427E-05, 6.468151674593822101E-05 ),
 .UNSPECIFIED. ) ;
#34281 = CARTESIAN_POINT ( 'NONE',  ( 4.045228995182856835, -26.97152095390259063, 7.750000000000000888 ) ) ;
#34282 = CARTESIAN_POINT ( 'NONE',  ( -62.99925096543692860, 37.98736139491209940, -4.069933184286554706 ) ) ;
#34283 = ADVANCED_FACE ( 'NONE', ( #29471 ), #36250, .T. ) ;
#34284 = CARTESIAN_POINT ( 'NONE',  ( 14.73982985784992117, -5.057483637003035604, -2.500280250512573854 ) ) ;
#34285 = CARTESIAN_POINT ( 'NONE',  ( -1.525269612006747488, -30.64473977883090328, 6.866852738645441434 ) ) ;
#34286 = ORIENTED_EDGE ( 'NONE', *, *, #11831, .F. ) ;
#34287 = DIRECTION ( 'NONE',  ( 1.000000000000000000, 0.000000000000000000, 0.000000000000000000 ) ) ;
#34288 = CARTESIAN_POINT ( 'NONE',  ( 70.80012018114213390, 59.83342440824694819, -3.954977122261608802 ) ) ;
#34289 = VECTOR ( 'NONE', #19961, 1000.000000000000000 ) ;
#34290 = VERTEX_POINT ( 'NONE', #1282 ) ;
#34291 = CYLINDRICAL_SURFACE ( 'NONE', #17983, 0.09010775117052841066 ) ;
#34292 = CARTESIAN_POINT ( 'NONE',  ( 0.04492882035419289849, -26.60017362597359636, 6.892063359921931642 ) ) ;
#34293 =( BOUNDED_CURVE ( )  B_SPLINE_CURVE ( 3, ( #29596, #15876, #1411, #28433 ),
 .UNSPECIFIED., .F., .T. ) 
 B_SPLINE_CURVE_WITH_KNOTS ( ( 4, 4 ),
 ( 4.708531083176466403, 4.895802057644187855 ),
 .UNSPECIFIED. ) 
 CURVE ( )  GEOMETRIC_REPRESENTATION_ITEM ( )  RATIONAL_B_SPLINE_CURVE ( ( 1.000000000000000000, 0.9970795998553221295, 0.9970795998553221295, 1.000000000000000000 ) ) 
 REPRESENTATION_ITEM ( '' )  );
#34294 = EDGE_CURVE ( 'NONE', #31377, #17770, #1108, .T. ) ;
#34295 = ADVANCED_FACE ( 'NONE', ( #7431 ), #16889, .F. ) ;
#34296 = CARTESIAN_POINT ( 'NONE',  ( 1.202039200222869475, -26.20663676950747600, 6.866852738645443210 ) ) ;
#34297 = CARTESIAN_POINT ( 'NONE',  ( 1.300000000000000044, 0.000000000000000000, 0.000000000000000000 ) ) ;
#34298 = VERTEX_POINT ( 'NONE', #26388 ) ;
#34299 = EDGE_CURVE ( 'NONE', #5793, #17630, #2064, .T. ) ;
#34300 = CARTESIAN_POINT ( 'NONE',  ( 23.75888155827460579, 3.577044823368265458, 3.132426108058699477 ) ) ;
#34301 = AXIS2_PLACEMENT_3D ( 'NONE', #7445, #19613, #20401 ) ;
#34302 = ORIENTED_EDGE ( 'NONE', *, *, #18441, .T. ) ;
#34303 = CARTESIAN_POINT ( 'NONE',  ( 78.85457743492895588, 65.01671056748381261, -3.151254463354985269 ) ) ;
#34304 = CARTESIAN_POINT ( 'NONE',  ( -1.487618233188356065, -30.75172851090044190, 7.643333865083958401 ) ) ;
#34305 = CARTESIAN_POINT ( 'NONE',  ( 81.80968396272736243, 62.04343910699808617, -2.011780557866150509 ) ) ;
#34306 = CARTESIAN_POINT ( 'NONE',  ( 79.89038670178254620, 63.31421865134938542, 3.734652355492745546 ) ) ;
#34307 = CARTESIAN_POINT ( 'NONE',  ( 4.340966779518038443, -27.42811908905094853, 6.887041543973317026 ) ) ;
#34309 = ORIENTED_EDGE ( 'NONE', *, *, #20621, .T. ) ;
#34308 = CARTESIAN_POINT ( 'NONE',  ( 2.787286031397239405, -32.79153584164929214, 7.782034975670476307 ) ) ;
#34310 = CARTESIAN_POINT ( 'NONE',  ( 21.85643539959776049, -10.96491163060450802, -3.419414754301954851 ) ) ;
#34311 = DIRECTION ( 'NONE',  ( 1.000000000000000000, 0.000000000000000000, 0.000000000000000000 ) ) ;
#34312 = ORIENTED_EDGE ( 'NONE', *, *, #16956, .F. ) ;
#34313 = CARTESIAN_POINT ( 'NONE',  ( -75.92086343153737005, 8.774164695908069689, 10.09508035950012506 ) ) ;
#34314 = CARTESIAN_POINT ( 'NONE',  ( -1.799527215904450417, -29.59426670074542898, 7.650127521910076389 ) ) ;
#34315 = CARTESIAN_POINT ( 'NONE',  ( -1.312560436656867724, -31.35097737660188244, 7.686927408461905920 ) ) ;
#34316 = CARTESIAN_POINT ( 'NONE',  ( 1.582902875548440669, -32.96790048997851130, 7.759451378593096749 ) ) ;
#34317 = CARTESIAN_POINT ( 'NONE',  ( 28.62670612262708758, -3.097740522901847093, -4.674287848576377691 ) ) ;
#34318 = CARTESIAN_POINT ( 'NONE',  ( 33.94692901654968153, -0.4865178363018504704, -5.119572993145925288 ) ) ;
#34319 = CARTESIAN_POINT ( 'NONE',  ( 1.700390093233090871, -29.56993018339339940, 7.800000000000000711 ) ) ;
#34320 = FACE_OUTER_BOUND ( 'NONE', #40544, .T. ) ;
#34321 = CARTESIAN_POINT ( 'NONE',  ( -73.07498068578524908, 39.58105274722134226, -46.17089178453873188 ) ) ;
#34322 = CARTESIAN_POINT ( 'NONE',  ( -0.8402781915718714467, -33.89858303842947151, 7.695279973900954751 ) ) ;
#34323 = DIRECTION ( 'NONE',  ( 1.000000000000000000, 0.000000000000000000, 0.000000000000000000 ) ) ;
#34324 = EDGE_CURVE ( 'NONE', #16788, #7910, #17089, .T. ) ;
#34325 = CARTESIAN_POINT ( 'NONE',  ( 17.55394540761496813, 14.11332787939523215, -2.499999999999998668 ) ) ;
#34326 = CARTESIAN_POINT ( 'NONE',  ( 24.71293417245692225, 0.6467480212540300810, -4.786583799029410002 ) ) ;
#34327 = CIRCLE ( 'NONE', #15865, 0.1000000000000028644 ) ;
#34328 = CARTESIAN_POINT ( 'NONE',  ( 37.19703447091560378, -2.679050652368330621, -5.993601543857010938 ) ) ;
#34329 = CARTESIAN_POINT ( 'NONE',  ( 24.39286117734144810, 2.948013837470140786, -3.707038986443544015 ) ) ;
#34330 = EDGE_LOOP ( 'NONE', ( #5087, #37670, #32005, #27030 ) ) ;
#34331 = CARTESIAN_POINT ( 'NONE',  ( 66.94886299149460740, 58.16124406473343811, 3.993952884371009926 ) ) ;
#34332 = CARTESIAN_POINT ( 'NONE',  ( 37.09997507242855619, -2.920746538320391217, 5.996328951322015932 ) ) ;
#34333 = CARTESIAN_POINT ( 'NONE',  ( -1.666958026621576883, -30.04000107135736641, 7.754798119455333705 ) ) ;
#34334 = EDGE_CURVE ( 'NONE', #12118, #17239, #7836, .T. ) ;
#34335 = CARTESIAN_POINT ( 'NONE',  ( -26.97867591359219475, -24.55319635012989110, 6.700000000000000178 ) ) ;
#34337 = EDGE_CURVE ( 'NONE', #35445, #36906, #15231, .T. ) ;
#34336 = CARTESIAN_POINT ( 'NONE',  ( 84.61987491094994596, 3.070148169510762415, -1.277140785624046426 ) ) ;
#34338 = CARTESIAN_POINT ( 'NONE',  ( 25.01075926162736351, 3.329891198200423563, 1.935509954479121886 ) ) ;
#34339 = B_SPLINE_CURVE_WITH_KNOTS ( 'NONE', 3,
 ( #16863, #14575, #30042, #27147, #29638, #8191, #23268, #32542, #1257, #1650, #36420, #7407, #17060, #26756, #26361, #4340, #1857, #17455, #39700 ),
 .UNSPECIFIED., .F., .F.,
 ( 4, 3, 3, 3, 3, 3, 4 ),
 ( 0.000000000000000000, 2.546128104244612306E-05, 5.711050680483668423E-05, 8.113074941675757728E-05, 0.0001053129305727077829, 0.0001360598016347089236, 0.0001612931755713787674 ),
 .UNSPECIFIED. ) ;
#34340 = EDGE_LOOP ( 'NONE', ( #29, #37157 ) ) ;
#34341 = CARTESIAN_POINT ( 'NONE',  ( 24.69446985135231643, 2.652829802148882532, 3.917487620480931465 ) ) ;
#34342 = CARTESIAN_POINT ( 'NONE',  ( 0.000000000000000000, 0.000000000000000000, 0.000000000000000000 ) ) ;
#34343 = CARTESIAN_POINT ( 'NONE',  ( 25.11437021580303863, 164.7550792202006562, 1.000000000000000000 ) ) ;
#34344 = EDGE_CURVE ( 'NONE', #13771, #21663, #6126, .T. ) ;
#34345 = ORIENTED_EDGE ( 'NONE', *, *, #37274, .T. ) ;
#34346 = CARTESIAN_POINT ( 'NONE',  ( -35.07867591359219972, -26.64985754041175525, 6.700000000000000178 ) ) ;
#34347 = VECTOR ( 'NONE', #10344, 1000.000000000000000 ) ;
#34348 = ORIENTED_EDGE ( 'NONE', *, *, #35348, .F. ) ;
#34349 = CARTESIAN_POINT ( 'NONE',  ( 80.85043593073625345, 61.68942038033311093, -2.615973384261002010 ) ) ;
#34350 = DIRECTION ( 'NONE',  ( 1.000000000000000000, -0.000000000000000000, 0.000000000000000000 ) ) ;
#34351 = CARTESIAN_POINT ( 'NONE',  ( 79.28293246176357911, 65.06528690105534452, 3.252077313700850070 ) ) ;
#34353 = ORIENTED_EDGE ( 'NONE', *, *, #36080, .F. ) ;
#34352 = CARTESIAN_POINT ( 'NONE',  ( -2.978675913592195190, -24.55319635012989110, 6.800000000000000711 ) ) ;
#34354 = CARTESIAN_POINT ( 'NONE',  ( -22.24874870218063450, -26.64985754041175525, 6.800000000000000711 ) ) ;
#34356 = DIRECTION ( 'NONE',  ( 0.000000000000000000, 0.000000000000000000, 1.000000000000000000 ) ) ;
#34355 = CARTESIAN_POINT ( 'NONE',  ( 4.922574738379127623, -30.93651010398624379, 6.912143950357338085 ) ) ;
#34357 = CARTESIAN_POINT ( 'NONE',  ( -70.92837670882107659, 28.72470171467712063, 4.357836081054403010 ) ) ;
#34358 = CARTESIAN_POINT ( 'NONE',  ( 14.72123706662754117, -4.461849342347327330, 2.504003097347841766 ) ) ;
#34359 = CARTESIAN_POINT ( 'NONE',  ( 21.85047837349528876, 5.846451070568255304, -3.185295450005349416 ) ) ;
#34360 = ORIENTED_EDGE ( 'NONE', *, *, #21905, .F. ) ;
#34361 = DIRECTION ( 'NONE',  ( -0.000000000000000000, -1.000000000000000000, -0.000000000000000000 ) ) ;
#34362 = CIRCLE ( 'NONE', #6065, 6.781342077912186461 ) ;
#34363 = CARTESIAN_POINT ( 'NONE',  ( 24.13449073166137637, 1.731319574254092997, -6.231442870084249464 ) ) ;
#34364 = CARTESIAN_POINT ( 'NONE',  ( -79.05013602958881336, -6.599521673326993465, -5.889945335535864857 ) ) ;
#34365 = PLANE ( 'NONE',  #21534 ) ;
#34366 = CARTESIAN_POINT ( 'NONE',  ( 81.51669253445732011, 62.40826230823216036, 2.731335034814801777 ) ) ;
#34367 = CARTESIAN_POINT ( 'NONE',  ( 85.07031394220433640, 1.982162274098862476, -4.809620659748507165 ) ) ;
#34368 = DIRECTION ( 'NONE',  ( 0.5000000000000101030, -0.8660254037844328234, -0.000000000000000000 ) ) ;
#34369 = ORIENTED_EDGE ( 'NONE', *, *, #25397, .T. ) ;
#34370 = CARTESIAN_POINT ( 'NONE',  ( -64.78473723156626818, 34.77447677474216903, -6.350763366688283007 ) ) ;
#34371 = PLANE ( 'NONE',  #25529 ) ;
#34372 = CARTESIAN_POINT ( 'NONE',  ( 3.973866779147308570, -26.90885826429679284, 6.894806418505347700 ) ) ;
#34373 = CYLINDRICAL_SURFACE ( 'NONE', #26522, 1.000000000000000444 ) ;
#34374 = CARTESIAN_POINT ( 'NONE',  ( 4.791138977812089195, -27.92775596988059306, 7.753200566781576875 ) ) ;
#34375 = CARTESIAN_POINT ( 'NONE',  ( -25.39999999999996305, 0.000000000000000000, 0.000000000000000000 ) ) ;
#34376 = CARTESIAN_POINT ( 'NONE',  ( -62.89148181836048934, 37.17958841060684705, 4.327622075141189129 ) ) ;
#34377 = CARTESIAN_POINT ( 'NONE',  ( 36.19384301497849776, -2.232512094164133210, 5.855322572525271774 ) ) ;
#34378 = CARTESIAN_POINT ( 'NONE',  ( 4.297763636622812911, -31.76394919647423265, 7.775108481317161591 ) ) ;
#34379 = CARTESIAN_POINT ( 'NONE',  ( 85.56690561042726983, 2.244914964738076613, -3.295588454431229497 ) ) ;
#34380 = ORIENTED_EDGE ( 'NONE', *, *, #9558, .F. ) ;
#34382 = CARTESIAN_POINT ( 'NONE',  ( -63.58520484588292732, 35.72026407271187765, 6.999999999999999112 ) ) ;
#34381 = CARTESIAN_POINT ( 'NONE',  ( 78.91475304129780000, 66.06124928554447706, -1.777114115212672596 ) ) ;
#34383 = CARTESIAN_POINT ( 'NONE',  ( 16.46868226795076140, -3.215900133094863111, 2.776734183136223777 ) ) ;
#34384 = DIRECTION ( 'NONE',  ( -3.491481338843133750E-15, 1.000000000000000000, -0.000000000000000000 ) ) ;
#34385 = AXIS2_PLACEMENT_3D ( 'NONE', #4596, #39978, #4789 ) ;
#34386 = CARTESIAN_POINT ( 'NONE',  ( 4.152525300728761692, -32.07686114568508629, 7.501983001166816045 ) ) ;
#34387 = ADVANCED_FACE ( 'NONE', ( #40339 ), #27177, .F. ) ;
#34388 = VERTEX_POINT ( 'NONE', #33998 ) ;
#34389 = CARTESIAN_POINT ( 'NONE',  ( -1.631201490816239996, -28.89133050973324401, 7.778050822775635531 ) ) ;
#34390 = CARTESIAN_POINT ( 'NONE',  ( -0.4665940226951585945, -26.82738204011747740, 7.771081512783700518 ) ) ;
#34391 = EDGE_CURVE ( 'NONE', #25044, #3598, #24292, .T. ) ;
#34392 = ORIENTED_EDGE ( 'NONE', *, *, #39409, .F. ) ;
#34393 = EDGE_CURVE ( 'NONE', #35820, #22017, #13697, .T. ) ;
#34394 = EDGE_LOOP ( 'NONE', ( #5501, #38201, #16719, #26687, #34189, #9271 ) ) ;
#34395 = CARTESIAN_POINT ( 'NONE',  ( 79.79114114151838066, 64.70569453017795070, -3.482375488376185046 ) ) ;
#34396 = CARTESIAN_POINT ( 'NONE',  ( -12.34874870218063947, -25.49307895267003587, 6.700000000000000178 ) ) ;
#34397 = VERTEX_POINT ( 'NONE', #19345 ) ;
#34399 = DIRECTION ( 'NONE',  ( 0.000000000000000000, -0.000000000000000000, -1.000000000000000000 ) ) ;
#34398 = CARTESIAN_POINT ( 'NONE',  ( 23.42816911322859852, 2.562534313632369276, 4.299399775110970268 ) ) ;
#34400 = EDGE_LOOP ( 'NONE', ( #1275, #22228, #22682, #23177, #28576 ) ) ;
#34401 = CARTESIAN_POINT ( 'NONE',  ( 80.64500926360288702, 65.89167229754902166, -2.340562087103693845 ) ) ;
#34402 = CARTESIAN_POINT ( 'NONE',  ( 4.672772079749174523, -27.91918934176055700, 6.887041543973315250 ) ) ;
#34404 = CARTESIAN_POINT ( 'NONE',  ( 86.46381120609095206, 1.237468029981063866, -4.897693362183704657 ) ) ;
#34403 = CARTESIAN_POINT ( 'NONE',  ( -38.34874870218063592, -26.64985754041175525, 6.700000000000000178 ) ) ;
#34405 = CARTESIAN_POINT ( 'NONE',  ( 1.259933197038312302, -26.09775540055275656, 7.013842709614101167 ) ) ;
#34406 = LINE ( 'NONE', #15427, #15595 ) ;
#34407 = CARTESIAN_POINT ( 'NONE',  ( 74.36844136632052482, 60.98005461696732254, 3.924711207976818717 ) ) ;
#34408 = CARTESIAN_POINT ( 'NONE',  ( 22.61679165579552020, 3.482051183000346661, -4.061253451716217988 ) ) ;
#34409 = ORIENTED_EDGE ( 'NONE', *, *, #18569, .T. ) ;
#34410 = CARTESIAN_POINT ( 'NONE',  ( 21.85643539959776049, -15.24219007203948983, -1.854490019360333086 ) ) ;
#34411 = CARTESIAN_POINT ( 'NONE',  ( 3.518482029086511531, -26.59117190302356448, 7.780491323090174660 ) ) ;
#34412 = VERTEX_POINT ( 'NONE', #15645 ) ;
#34413 = DIRECTION ( 'NONE',  ( 1.000000000000000000, 0.000000000000000000, 0.000000000000000000 ) ) ;
#34414 = CARTESIAN_POINT ( 'NONE',  ( 79.60170308687705187, 66.12598108333452274, 2.076176908533791554 ) ) ;
#34415 = CARTESIAN_POINT ( 'NONE',  ( 85.81943862418182789, 1.961257897749014045, -4.406084401447566634 ) ) ;
#34416 = B_SPLINE_CURVE_WITH_KNOTS ( 'NONE', 3,
 ( #26299, #9834, #19512, #38635, #16210, #34980, #4275, #16798, #4479, #35771 ),
 .UNSPECIFIED., .F., .F.,
 ( 4, 3, 3, 4 ),
 ( 0.0001585009270395681339, 0.0001815657551981822698, 0.0002118214035944112315, 0.0002170292169044690887 ),
 .UNSPECIFIED. ) ;
#34417 = ORIENTED_EDGE ( 'NONE', *, *, #3346, .F. ) ;
#34418 = AXIS2_PLACEMENT_3D ( 'NONE', #12649, #39889, #28094 ) ;
#34419 = VERTEX_POINT ( 'NONE', #25121 ) ;
#34420 = CARTESIAN_POINT ( 'NONE',  ( 33.10591517636001413, -3.525528538284762980, 5.308841012747972599 ) ) ;
#34421 = CARTESIAN_POINT ( 'NONE',  ( 1.057242960569753309, -26.12952878737186424, 7.686927408461905031 ) ) ;
#34422 = CARTESIAN_POINT ( 'NONE',  ( 35.45475390766367951, -1.911721085124097108, -5.739969842391221100 ) ) ;
#34423 = CARTESIAN_POINT ( 'NONE',  ( 5.100237809806897005, -29.53775093374590810, 7.721096864323900633 ) ) ;
#34424 = CARTESIAN_POINT ( 'NONE',  ( 4.724705146729046845, -27.80824960587721506, 7.635761828346577573 ) ) ;
#34425 = DIRECTION ( 'NONE',  ( -0.6605219282605402364, 0.000000000000000000, -0.7508067542896625923 ) ) ;
#34426 = VERTEX_POINT ( 'NONE', #13357 ) ;
#34427 = CARTESIAN_POINT ( 'NONE',  ( 33.94443037723285528, -0.4909204995510449976, 5.125095304665048701 ) ) ;
#34428 = CARTESIAN_POINT ( 'NONE',  ( -71.14735168035940660, 0.1989745095792901375, 6.009053033063231020 ) ) ;
#34429 = CARTESIAN_POINT ( 'NONE',  ( 66.43484696874310202, 57.75462747860463963, -4.000000000000005329 ) ) ;
#34430 = CARTESIAN_POINT ( 'NONE',  ( 87.67362551673814153, -2.207058729090509264, -2.772829007886140396 ) ) ;
#34431 = ORIENTED_EDGE ( 'NONE', *, *, #25680, .T. ) ;
#34432 = CARTESIAN_POINT ( 'NONE',  ( -56.24615026952712782, 30.21122693717881802, 1.618048866027589572 ) ) ;
#34434 = ADVANCED_FACE ( 'NONE', ( #38271 ), #21830, .F. ) ;
#34433 = CARTESIAN_POINT ( 'NONE',  ( -73.59999746138505827, -3.294935041615913107, -9.639447355971549669 ) ) ;
#34435 = DIRECTION ( 'NONE',  ( 1.000000000000000000, 0.000000000000000000, 0.000000000000000000 ) ) ;
#34436 = FACE_BOUND ( 'NONE', #31757, .T. ) ;
#34437=STYLED_ITEM('',(#40773),#26623);
#34438 = CARTESIAN_POINT ( 'NONE',  ( -25.39999999999996305, 3.061616997868383141E-16, -2.500000000000000000 ) ) ;
#34439 = ORIENTED_EDGE ( 'NONE', *, *, #23255, .T. ) ;
#34440 = CARTESIAN_POINT ( 'NONE',  ( 22.62113927429973970, 4.590997775111404167, 3.081078265741201694 ) ) ;
#34441 = B_SPLINE_CURVE_WITH_KNOTS ( 'NONE', 3,
 ( #30419, #36791, #14149, #33527, #36189, #17629, #36592, #7969, #24230, #14965, #20521, #8369, #2225, #14747, #4696, #5298, #27530, #33104, #40082 ),
 .UNSPECIFIED., .F., .F.,
 ( 4, 3, 3, 3, 3, 3, 4 ),
 ( 0.000000000000000000, 2.546128104244709884E-05, 5.711050680483773455E-05, 8.113074941675650663E-05, 0.0001053129305727056823, 0.0001360598016347088965, 0.0001612931755702009173 ),
 .UNSPECIFIED. ) ;
#34442 = CARTESIAN_POINT ( 'NONE',  ( 82.07069543531865463, 65.18928443706812459, -1.480606629406893804 ) ) ;
#34443 = CARTESIAN_POINT ( 'NONE',  ( 81.10109024085375040, 61.27893947540407993, 1.252362053669522801 ) ) ;
#34444 = CARTESIAN_POINT ( 'NONE',  ( -38.24874870218063450, -26.64985754041175525, 6.800000000000000711 ) ) ;
#34445 = VERTEX_POINT ( 'NONE', #9874 ) ;
#34446 = CARTESIAN_POINT ( 'NONE',  ( 77.57451768555480953, 61.52186891572922178, -3.722835383490939787 ) ) ;
#34447 = CARTESIAN_POINT ( 'NONE',  ( 14.76059668380545808, 12.79626003940931334, -2.505178952959561833 ) ) ;
#34449 = CARTESIAN_POINT ( 'NONE',  ( 37.19747299874393320, -2.841585884120807481, 5.999818732555961098 ) ) ;
#34448 = CARTESIAN_POINT ( 'NONE',  ( 3.953929392453140235, -32.24611259444524336, 7.762796336881262249 ) ) ;
#34450 = CARTESIAN_POINT ( 'NONE',  ( 18.49040214524046277, 7.936735459317859842, -3.063322579770844545 ) ) ;
#34451 = CARTESIAN_POINT ( 'NONE',  ( 81.15131294690949915, 61.29729393613784083, -1.130345937366652898 ) ) ;
#34452 = PLANE ( 'NONE',  #23462 ) ;
#34453 = CARTESIAN_POINT ( 'NONE',  ( 77.57912958173200479, 64.32824690378610910, 3.266768353517001788 ) ) ;
#34454 = VERTEX_POINT ( 'NONE', #16840 ) ;
#34455 = AXIS2_PLACEMENT_3D ( 'NONE', #16165, #7500, #28729 ) ;
#34456 = CARTESIAN_POINT ( 'NONE',  ( 4.739243575545716958, -31.30641337154872161, 7.638132480492516585 ) ) ;
#34457 = CYLINDRICAL_SURFACE ( 'NONE', #32864, 3.399999999999999911 ) ;
#34458 = CARTESIAN_POINT ( 'NONE',  ( 82.26467961623025360, 63.75423115438312749, 2.259066313177354512 ) ) ;
#34460 = CARTESIAN_POINT ( 'NONE',  ( -1.582490140158303138, -30.78347898942401173, 7.640616322432099317 ) ) ;
#34459 = CARTESIAN_POINT ( 'NONE',  ( 4.253769420360524300, -31.96372510585761262, 6.961115707816238007 ) ) ;
#34461 = CARTESIAN_POINT ( 'NONE',  ( 28.29523375420085074, 1.184784106264966219, 4.843441543353563361 ) ) ;
#34462 = EDGE_CURVE ( 'NONE', #12705, #13485, #30018, .T. ) ;
#34463 = CARTESIAN_POINT ( 'NONE',  ( 5.121324086407808451, -26.64985754041175525, 6.700000000000000178 ) ) ;
#34464 = DIRECTION ( 'NONE',  ( 1.000000000000000000, 0.000000000000000000, 0.000000000000000000 ) ) ;
#34465 = CARTESIAN_POINT ( 'NONE',  ( -63.23359472962078343, 35.57513467056965339, 6.582177359050705334 ) ) ;
#34466 = CARTESIAN_POINT ( 'NONE',  ( 25.38078854466783696, 0.7236405097827043331, -4.601989520496759134 ) ) ;
#34467 = CYLINDRICAL_SURFACE ( 'NONE', #28766, 0.1000000000000028644 ) ;
#34468 = CARTESIAN_POINT ( 'NONE',  ( -0.6339409410646490439, -32.04195642642311270, 6.997764925645181933 ) ) ;
#34469 = DIRECTION ( 'NONE',  ( 0.000000000000000000, 0.000000000000000000, 1.000000000000000000 ) ) ;
#34470 = CARTESIAN_POINT ( 'NONE',  ( 33.45716606812183613, -3.829385970599605393, -5.093809925484540813 ) ) ;
#34471 = CARTESIAN_POINT ( 'NONE',  ( 36.86628255965130307, -3.288546807751189238, -5.928673330178329870 ) ) ;
#34472 = CARTESIAN_POINT ( 'NONE',  ( -10.87867591359219155, -26.64985754041175525, 6.700000000000000178 ) ) ;
#34473 = CARTESIAN_POINT ( 'NONE',  ( 31.04874620950890218, -3.764186376626990072, 4.612088004693758236 ) ) ;
#34474 = CYLINDRICAL_SURFACE ( 'NONE', #10788, 3.000000000000002665 ) ;
#34475 = CYLINDRICAL_SURFACE ( 'NONE', #16628, 0.09010775117053032579 ) ;
#34476 = CARTESIAN_POINT ( 'NONE',  ( -42.24874870218063450, -25.49307895267003587, 6.700000000000000178 ) ) ;
#34477 = CARTESIAN_POINT ( 'NONE',  ( 1.664433243520564876, -26.17012032033359148, 7.695279973900954751 ) ) ;
#34478 = CARTESIAN_POINT ( 'NONE',  ( -15.07867591359219439, -26.64985754041175525, 6.700000000000000178 ) ) ;
#34479 = CARTESIAN_POINT ( 'NONE',  ( 22.03385624869050829, -11.53008493239669718, 2.499999999999999556 ) ) ;
#34480 = ORIENTED_EDGE ( 'NONE', *, *, #18388, .F. ) ;
#34481 = DIRECTION ( 'NONE',  ( -1.000000000000000000, 0.000000000000000000, 0.000000000000000000 ) ) ;
#34482 = CARTESIAN_POINT ( 'NONE',  ( 70.63497465855112978, 60.23961165191135336, -3.862811858476220550 ) ) ;
#34483 = CIRCLE ( 'NONE', #4204, 3.499999999999999556 ) ;
#34484 = ORIENTED_EDGE ( 'NONE', *, *, #34843, .T. ) ;
#34485 = AXIS2_PLACEMENT_3D ( 'NONE', #8829, #39935, #5763 ) ;
#34486 = CYLINDRICAL_SURFACE ( 'NONE', #33139, 3.000000000000002665 ) ;
#34488 = EDGE_CURVE ( 'NONE', #24849, #22624, #5303, .T. ) ;
#34487 = CARTESIAN_POINT ( 'NONE',  ( 11.29080664838499182, -35.94265729135299381, -2.500000000000000000 ) ) ;
#34489 = CARTESIAN_POINT ( 'NONE',  ( 5.036121742574604099, -28.51026308303529788, 6.875780273367531059 ) ) ;
#34490 = CARTESIAN_POINT ( 'NONE',  ( -1.441894026320721611, -28.27145010576420248, 6.868387053540520704 ) ) ;
#34491 = CARTESIAN_POINT ( 'NONE',  ( 1.311050557978938214, -26.19229569661303358, 6.988553391373220514 ) ) ;
#34492 = CARTESIAN_POINT ( 'NONE',  ( 5.026819207240812659, -30.27339969195919522, 7.761597726988851420 ) ) ;
#34493 = ORIENTED_EDGE ( 'NONE', *, *, #36300, .F. ) ;
#34494 = CARTESIAN_POINT ( 'NONE',  ( 23.76174458026235925, 3.579459537482711173, 3.123613177595400359 ) ) ;
#34495 = DIRECTION ( 'NONE',  ( 1.000000000000000000, 0.000000000000000000, -0.000000000000000000 ) ) ;
#34496 = AXIS2_PLACEMENT_3D ( 'NONE', #20511, #40269, #36580 ) ;
#34497 = ORIENTED_EDGE ( 'NONE', *, *, #19642, .T. ) ;
#34498 = CARTESIAN_POINT ( 'NONE',  ( 79.66447349905094200, 63.54298318056227401, -3.741985197832887966 ) ) ;
#34500 = CARTESIAN_POINT ( 'NONE',  ( -1.677331764060516095, -29.95852058763195913, 6.920489980334480151 ) ) ;
#34499 = CARTESIAN_POINT ( 'NONE',  ( 25.84749379405300829, 0.9947621561361583709, 4.433988674360729298 ) ) ;
#34501 = CARTESIAN_POINT ( 'NONE',  ( 80.10847647497631385, 65.88576991956392703, -2.484976468875493172 ) ) ;
#34502 = CARTESIAN_POINT ( 'NONE',  ( 78.88927015299483969, 65.04551736973371590, 3.140153738741057410 ) ) ;
#34503 = EDGE_CURVE ( 'NONE', #1874, #18519, #9267, .T. ) ;
#34504 = CARTESIAN_POINT ( 'NONE',  ( 4.363912183534078615, -27.45669894310492865, 6.866852738645444099 ) ) ;
#34505 = CARTESIAN_POINT ( 'NONE',  ( 79.68852728668518637, 66.33522678087791746, 1.000000000000000000 ) ) ;
#34506 = CARTESIAN_POINT ( 'NONE',  ( 2.880877094127454630, -32.75841735456398851, 7.748216051605119503 ) ) ;
#34507 = CARTESIAN_POINT ( 'NONE',  ( 22.31758782591801094, 6.227955964823622459, -0.6941013191108784675 ) ) ;
#34508 = FACE_OUTER_BOUND ( 'NONE', #31161, .T. ) ;
#34509 = ORIENTED_EDGE ( 'NONE', *, *, #36402, .F. ) ;
#34510 = CARTESIAN_POINT ( 'NONE',  ( -72.92764087594211730, 1.045607383799636914, 10.95381248315954892 ) ) ;
#34511 = CARTESIAN_POINT ( 'NONE',  ( 34.98542202245123178, -3.831422351504832235, 5.422976750267761048 ) ) ;
#34512 = ORIENTED_EDGE ( 'NONE', *, *, #13258, .T. ) ;
#34513 = CARTESIAN_POINT ( 'NONE',  ( -1.593127767899503722, -28.38555688987459291, 7.635761828346575797 ) ) ;
#34514 = AXIS2_PLACEMENT_3D ( 'NONE', #37112, #33644, #14662 ) ;
#34515 = DIRECTION ( 'NONE',  ( 0.000000000000000000, -0.6605219282605379050, 0.7508067542896647018 ) ) ;
#34516 = CARTESIAN_POINT ( 'NONE',  ( 3.419202797897241908, -26.52104794612278837, 7.698786668945008849 ) ) ;
#34517 = CARTESIAN_POINT ( 'NONE',  ( 33.45672436422175622, -3.834025908535790617, -5.088635116787304291 ) ) ;
#34518 = CARTESIAN_POINT ( 'NONE',  ( 3.796999183887054929, -32.24653817131153488, 6.864276522220859711 ) ) ;
#34519 = CARTESIAN_POINT ( 'NONE',  ( 18.57920759633674379, 8.033290316770353101, 3.021679359481073579 ) ) ;
#34520 = DIRECTION ( 'NONE',  ( 0.000000000000000000, -0.000000000000000000, -1.000000000000000000 ) ) ;
#34521 = DIRECTION ( 'NONE',  ( 1.000000000000000000, -0.000000000000000000, 0.000000000000000000 ) ) ;
#34522 = EDGE_CURVE ( 'NONE', #11084, #21833, #29878, .T. ) ;
#34523 = EDGE_CURVE ( 'NONE', #35525, #19049, #6343, .T. ) ;
#34524 = CARTESIAN_POINT ( 'NONE',  ( -71.92837670882107659, -20.78299143688747819, 38.00000000000000711 ) ) ;
#34525 = EDGE_CURVE ( 'NONE', #1708, #14526, #30322, .T. ) ;
#34526 = CIRCLE ( 'NONE', #32510, 7.999999999999986677 ) ;
#34527 = LINE ( 'NONE', #18849, #38152 ) ;
#34528 = CARTESIAN_POINT ( 'NONE',  ( 22.41226710412750123, 0.3842729703838025923, -6.836439051281914203 ) ) ;
#34529 = CARTESIAN_POINT ( 'NONE',  ( 1.495091655194762614, -33.07074825365423720, 7.387053503561888057 ) ) ;
#34530 = CARTESIAN_POINT ( 'NONE',  ( 24.38031847485193992, 2.859899372990460265, -3.804262765778354094 ) ) ;
#34531 = ORIENTED_EDGE ( 'NONE', *, *, #23445, .F. ) ;
#34532 =( BOUNDED_CURVE ( )  B_SPLINE_CURVE ( 3, ( #24868, #34566, #37408, #6338 ),
 .UNSPECIFIED., .F., .F. ) 
 B_SPLINE_CURVE_WITH_KNOTS ( ( 4, 4 ),
 ( 4.748221474220558846, 4.941946782021394036 ),
 .UNSPECIFIED. ) 
 CURVE ( )  GEOMETRIC_REPRESENTATION_ITEM ( )  RATIONAL_B_SPLINE_CURVE ( ( 1.000000000000000000, 0.9968749865767494445, 0.9968749865767494445, 1.000000000000000000 ) ) 
 REPRESENTATION_ITEM ( '' )  );
#34533 = CARTESIAN_POINT ( 'NONE',  ( 67.00300875778714271, 58.01168839481970707, 3.999354069328931782 ) ) ;
#34534 = CARTESIAN_POINT ( 'NONE',  ( 37.02901651221678492, -3.025130311963915464, 5.984744259697210467 ) ) ;
#34535 = CARTESIAN_POINT ( 'NONE',  ( -1.653081132413799281, -30.13049306011495077, 7.782167645815905033 ) ) ;
#34536 = PLANE ( 'NONE',  #22078 ) ;
#34537 = CARTESIAN_POINT ( 'NONE',  ( 84.32156544206206661, 3.079100735703119707, -0.4907544566128131391 ) ) ;
#34538 = EDGE_CURVE ( 'NONE', #11704, #637, #12566, .T. ) ;
#34539 = CARTESIAN_POINT ( 'NONE',  ( 34.93825735751887152, -3.179062036616587150, -5.659358064224856655 ) ) ;
#34540 = ORIENTED_EDGE ( 'NONE', *, *, #18659, .T. ) ;
#34541 = CARTESIAN_POINT ( 'NONE',  ( 26.28029581147721316, 1.816827303229512358, 4.266281445978443720 ) ) ;
#34542 = EDGE_LOOP ( 'NONE', ( #33042, #28378, #15411, #1031, #16201 ) ) ;
#34543 = DIRECTION ( 'NONE',  ( 1.000000000000000000, 0.000000000000000000, 0.000000000000000000 ) ) ;
#34544 = AXIS2_PLACEMENT_3D ( 'NONE', #36924, #30140, #24569 ) ;
#34545 = UNCERTAINTY_MEASURE_WITH_UNIT (LENGTH_MEASURE( 1.000000000000000082E-05 ), #32553, 'distance_accuracy_value', 'NONE');
#34546 = AXIS2_PLACEMENT_3D ( 'NONE', #19709, #12918, #29180 ) ;
#34547 = ORIENTED_EDGE ( 'NONE', *, *, #6940, .F. ) ;
#34548 = DIRECTION ( 'NONE',  ( 0.000000000000000000, 0.000000000000000000, 1.000000000000000000 ) ) ;
#34549 = ORIENTED_EDGE ( 'NONE', *, *, #13773, .F. ) ;
#34550 = CARTESIAN_POINT ( 'NONE',  ( 78.99045122244679362, 65.44959329978490814, -2.843122152733564167 ) ) ;
#34551 = AXIS2_PLACEMENT_3D ( 'NONE', #333, #34521, #24615 ) ;
#34552 = B_SPLINE_CURVE_WITH_KNOTS ( 'NONE', 3,
 ( #31769, #28675, #32382, #4177, #10331, #7045, #16110, #13020, #9518, #25178, #25584, #31566, #9930, #22099, #34677, #23105, #4764, #32583, #7649 ),
 .UNSPECIFIED., .F., .F.,
 ( 4, 3, 3, 3, 3, 3, 4 ),
 ( 0.000000000000000000, 2.546128104244941632E-05, 5.711050680484522232E-05, 8.113074941676646774E-05, 0.0001053129305727113066, 0.0001360598016347110649, 0.0001612931755713681694 ),
 .UNSPECIFIED. ) ;
#34553 = CARTESIAN_POINT ( 'NONE',  ( -1.348517286369409263, -27.85116208076715694, 7.695279973900954751 ) ) ;
#34554 = CARTESIAN_POINT ( 'NONE',  ( 78.67256861866690087, 65.85712333569000521, 2.031354376635688741 ) ) ;
#34557 = VERTEX_POINT ( 'NONE', #7786 ) ;
#34556 = ORIENTED_EDGE ( 'NONE', *, *, #10029, .F. ) ;
#34555 = CARTESIAN_POINT ( 'NONE',  ( 14.61802081865033820, 12.48098255133615453, 2.500000000000000000 ) ) ;
#34558 = VECTOR ( 'NONE', #24278, 1000.000000000000000 ) ;
#34559 = ADVANCED_FACE ( 'NONE', ( #13565 ), #4318, .T. ) ;
#34560 = CARTESIAN_POINT ( 'NONE',  ( -59.01732008375349636, 27.93907603120367966, 6.194723111030699059 ) ) ;
#34561 = CARTESIAN_POINT ( 'NONE',  ( 24.86588413226784766, -5.834012684512337898, 2.864494517088915337 ) ) ;
#34562 = DIRECTION ( 'NONE',  ( -1.000000000000000000, 0.000000000000000000, 0.000000000000000000 ) ) ;
#34563 = CARTESIAN_POINT ( 'NONE',  ( -54.83702497256466302, 31.47896333382912104, 1.097604620046560564 ) ) ;
#34564 = CARTESIAN_POINT ( 'NONE',  ( 23.73594193330650626, 3.550460969293395941, -3.216120006333157644 ) ) ;
#34565 = ORIENTED_EDGE ( 'NONE', *, *, #8969, .F. ) ;
#34566 = CARTESIAN_POINT ( 'NONE',  ( 4.979517197198048528, -30.49496054528498945, 7.505001789837629111 ) ) ;
#34567 = ORIENTED_EDGE ( 'NONE', *, *, #27726, .T. ) ;
#34568 = CARTESIAN_POINT ( 'NONE',  ( 25.45397947482645762, -4.047761836529544688, -3.708248611797466232 ) ) ;
#34569 = EDGE_CURVE ( 'NONE', #6772, #38905, #5994, .T. ) ;
#34570 = CARTESIAN_POINT ( 'NONE',  ( -78.55304626648006661, -6.529379806983721224, -6.520005268348637806 ) ) ;
#34571 = CARTESIAN_POINT ( 'NONE',  ( 4.025803068412391106, -27.08951600530382464, 7.013842709614101167 ) ) ;
#34572 = CARTESIAN_POINT ( 'NONE',  ( 81.43870310587519157, 62.97649354279256784, 3.113722587674266684 ) ) ;
#34573 = CARTESIAN_POINT ( 'NONE',  ( 88.08925887309592895, -2.022426073114577338, 2.982665067064442788 ) ) ;
#34574 = DIRECTION ( 'NONE',  ( -0.4690749385695657803, -0.8831583674551003460, 0.000000000000000000 ) ) ;
#34575 = ORIENTED_EDGE ( 'NONE', *, *, #18077, .T. ) ;
#34576 = CYLINDRICAL_SURFACE ( 'NONE', #3690, 3.399999999999999911 ) ;
#34577 = DIRECTION ( 'NONE',  ( 0.000000000000000000, 0.000000000000000000, -1.000000000000000000 ) ) ;
#34578 = ADVANCED_FACE ( 'NONE', ( #29813 ), #329, .T. ) ;
#34579 = AXIS2_PLACEMENT_3D ( 'NONE', #7603, #17862, #20757 ) ;
#34580 = CARTESIAN_POINT ( 'NONE',  ( 4.077496327744512428, -27.00100707246794229, 6.895394898881669121 ) ) ;
#34581 = PLANE ( 'NONE',  #8751 ) ;
#34582 = DIRECTION ( 'NONE',  ( 0.3754033771448330725, -0.6502177225477903111, 0.6605219282605379050 ) ) ;
#34583 = CARTESIAN_POINT ( 'NONE',  ( 36.78893668764049352, -3.040219878132970344, 5.948201332539075459 ) ) ;
#34584 = EDGE_CURVE ( 'NONE', #35289, #35977, #35305, .T. ) ;
#34585 = VECTOR ( 'NONE', #6941, 1000.000000000000000 ) ;
#34586 = CARTESIAN_POINT ( 'NONE',  ( 85.19528866922426857, 2.662332751101227579, -1.941753459690362726 ) ) ;
#34587 = ORIENTED_EDGE ( 'NONE', *, *, #38462, .T. ) ;
#34589 = CARTESIAN_POINT ( 'NONE',  ( 14.75451844360372178, -5.147523147571517299, 2.499999999999998668 ) ) ;
#34588 = CARTESIAN_POINT ( 'NONE',  ( 78.66413930541318678, 66.03995068206980079, -1.171933751919276956 ) ) ;
#34590 = CARTESIAN_POINT ( 'NONE',  ( -2.726063116431162392, -27.94446379774605660, 7.635761828346577573 ) ) ;
#34591 = CARTESIAN_POINT ( 'NONE',  ( 14.72179218383689481, 13.26053291077059626, -2.500109524128790728 ) ) ;
#34592 = ORIENTED_EDGE ( 'NONE', *, *, #40516, .T. ) ;
#34593 = CARTESIAN_POINT ( 'NONE',  ( 25.13734313143301335, -5.618766742075456122, -2.946603579881577062 ) ) ;
#34594 = ORIENTED_EDGE ( 'NONE', *, *, #11414, .F. ) ;
#34595 = CARTESIAN_POINT ( 'NONE',  ( 8.290806648384990041, 0.000000000000000000, 2.500000000000000000 ) ) ;
#34597 = EDGE_LOOP ( 'NONE', ( #34540, #24017, #12774, #6921 ) ) ;
#34596 = ORIENTED_EDGE ( 'NONE', *, *, #35267, .F. ) ;
#34598 = CARTESIAN_POINT ( 'NONE',  ( 79.01164091803717326, 65.74483092438761389, -2.494286432550484989 ) ) ;
#34599 = CARTESIAN_POINT ( 'NONE',  ( 5.150819523378970644, -30.15690496803471277, 7.744938106820261403 ) ) ;
#34601 = CARTESIAN_POINT ( 'NONE',  ( 14.77315594796471743, 13.19392823276620419, 2.499999999999996891 ) ) ;
#34600 = CARTESIAN_POINT ( 'NONE',  ( 22.67068927409770041, 2.950683925037858035, 4.428361241734660503 ) ) ;
#34602 = ORIENTED_EDGE ( 'NONE', *, *, #2862, .F. ) ;
#34603 = CARTESIAN_POINT ( 'NONE',  ( 79.46293960946091772, 66.21290357410880745, -1.708467252431211003 ) ) ;
#34604 = EDGE_CURVE ( 'NONE', #12996, #2693, #2783, .T. ) ;
#34605 = AXIS2_PLACEMENT_3D ( 'NONE', #21999, #21377, #9411 ) ;
#34606 = VECTOR ( 'NONE', #23278, 1000.000000000000114 ) ;
#34607 = CARTESIAN_POINT ( 'NONE',  ( -30.24874870218063450, -25.49307895267003587, 6.800000000000000711 ) ) ;
#34609 = CARTESIAN_POINT ( 'NONE',  ( 85.73004710101714920, 2.061666699345307663, -3.754548065942108881 ) ) ;
#34608 = CARTESIAN_POINT ( 'NONE',  ( -63.99293516169446150, 35.89893413629672381, 7.506047544094577084 ) ) ;
#34610 = PLANE ( 'NONE',  #19195 ) ;
#34611 = CARTESIAN_POINT ( 'NONE',  ( 0.5567163972659970872, -26.27754685773958698, 7.785344483711591934 ) ) ;
#34612 = CARTESIAN_POINT ( 'NONE',  ( 73.17398396214588274, 60.59975200455691891, 3.944160774623525434 ) ) ;
#34613 = CARTESIAN_POINT ( 'NONE',  ( 22.59525629365376886, 3.701236930939566072, -3.909849338992366974 ) ) ;
#34614 = ORIENTED_EDGE ( 'NONE', *, *, #8241, .T. ) ;
#34615 = EDGE_CURVE ( 'NONE', #33127, #39661, #15719, .T. ) ;
#34616 = AXIS2_PLACEMENT_3D ( 'NONE', #4761, #32976, #17295 ) ;
#34617 = CARTESIAN_POINT ( 'NONE',  ( 21.85643539959776049, -14.86125632165375343, -4.251346793879176467 ) ) ;
#34618 = ADVANCED_FACE ( 'NONE', ( #12624 ), #14892, .F. ) ;
#34619 = CARTESIAN_POINT ( 'NONE',  ( 3.494148792721590180, -26.58186483752615814, 7.785593909369613819 ) ) ;
#34620 = ORIENTED_EDGE ( 'NONE', *, *, #17999, .F. ) ;
#34621 = CARTESIAN_POINT ( 'NONE',  ( -1.146144745493847150, -27.71056485836612637, 7.013842709614101167 ) ) ;
#34622 = CARTESIAN_POINT ( 'NONE',  ( 81.85373309064779335, 62.29294994509999128, 2.264354540981406316 ) ) ;
#34623 = CARTESIAN_POINT ( 'NONE',  ( 85.38025200535193449, 2.454573153073208225, 3.240196491381199362 ) ) ;
#34624 = EDGE_LOOP ( 'NONE', ( #1923, #23897, #32267, #31203 ) ) ;
#34625 = EDGE_CURVE ( 'NONE', #7910, #12163, #6748, .T. ) ;
#34626 = DIRECTION ( 'NONE',  ( 0.000000000000000000, -0.1369933068956149802, -0.9905719730871674900 ) ) ;
#34627 = CARTESIAN_POINT ( 'NONE',  ( 15.08693209430224691, -4.053257314178727810, 2.560592534577949220 ) ) ;
#34628 = EDGE_CURVE ( 'NONE', #11656, #21561, #11275, .T. ) ;
#34629 = CARTESIAN_POINT ( 'NONE',  ( 27.40697018688743825, 0.9632752721768236270, -4.483918556379298259 ) ) ;
#34630 = CARTESIAN_POINT ( 'NONE',  ( 5.098439472760125213, -29.68508405565106401, 7.761597726988852308 ) ) ;
#34631 = CARTESIAN_POINT ( 'NONE',  ( 0.5037982502477853508, -26.38745190989316214, 7.695279973900954751 ) ) ;
#34632 = CARTESIAN_POINT ( 'NONE',  ( -64.08758708074093136, 38.13199975834722721, -3.043809435734133650 ) ) ;
#34633 = DIRECTION ( 'NONE',  ( 0.000000000000000000, 0.000000000000000000, 1.000000000000000000 ) ) ;
#34634 = ORIENTED_EDGE ( 'NONE', *, *, #39884, .F. ) ;
#34635 = ORIENTED_EDGE ( 'NONE', *, *, #8302, .F. ) ;
#34636 = CARTESIAN_POINT ( 'NONE',  ( 36.68389848233819350, -1.917438981616092386, 5.804549737457618264 ) ) ;
#34637 = CARTESIAN_POINT ( 'NONE',  ( 1.605927042630150403, -33.06148854684589367, 7.776484688137386136 ) ) ;
#34638 = CIRCLE ( 'NONE', #3086, 117.6618724293813898 ) ;
#34639 = ORIENTED_EDGE ( 'NONE', *, *, #9115, .T. ) ;
#34640 = CARTESIAN_POINT ( 'NONE',  ( 66.42495344877994512, 57.78257748056734755, -4.000000000000014211 ) ) ;
#34641 = ORIENTED_EDGE ( 'NONE', *, *, #22898, .F. ) ;
#34642 = CARTESIAN_POINT ( 'NONE',  ( 88.13248502410320384, -0.6368656024474566024, -2.456193918704937751 ) ) ;
#34643 = CARTESIAN_POINT ( 'NONE',  ( -72.93001361936202898, -2.241696845072889133, -9.799423676346561862 ) ) ;
#34644 = CARTESIAN_POINT ( 'NONE',  ( 4.960094596816839285, -28.60332449888920081, 6.929923840112064859 ) ) ;
#34645 = PLANE ( 'NONE',  #24124 ) ;
#34646 = DIRECTION ( 'NONE',  ( -0.000000000000000000, -0.000000000000000000, -1.000000000000000000 ) ) ;
#34647 = B_SPLINE_CURVE_WITH_KNOTS ( 'NONE', 3,
 ( #10936, #35484, #20209, #1909, #19817, #23115, #32393, #1302, #13839, #38938 ),
 .UNSPECIFIED., .F., .F.,
 ( 4, 3, 3, 4 ),
 ( 1.964321818484475877E-18, 3.025570593002917179E-05, 6.051145698343843299E-05, 6.468151674594082310E-05 ),
 .UNSPECIFIED. ) ;
#34648 = ORIENTED_EDGE ( 'NONE', *, *, #14086, .F. ) ;
#34649 = FACE_BOUND ( 'NONE', #39659, .T. ) ;
#34650 = DIRECTION ( 'NONE',  ( 0.000000000000000000, 0.000000000000000000, 1.000000000000000000 ) ) ;
#34651 = ORIENTED_EDGE ( 'NONE', *, *, #40511, .F. ) ;
#34652 = B_SPLINE_CURVE_WITH_KNOTS ( 'NONE', 3,
 ( #16702, #7252, #20207, #39137, #29681, #32987, #19815, #32391, #4185, #38737, #20010, #4582, #1493, #14026 ),
 .UNSPECIFIED., .F., .F.,
 ( 4, 2, 2, 2, 2, 2, 4 ),
 ( 0.000000000000000000, 0.001249862075310702141, 0.001874793112966059282, 0.002499724150621416424, 0.003124655188276773566, 0.003749586225932131141, 0.004999448301242839787 ),
 .UNSPECIFIED. ) ;
#34653 = CARTESIAN_POINT ( 'NONE',  ( 81.82660409393641032, 65.45354236959398975, -1.617049763656951411 ) ) ;
#34654 = CARTESIAN_POINT ( 'NONE',  ( 78.63380675089919691, 66.01840951946610403, 1.252362053669530795 ) ) ;
#34655 = CARTESIAN_POINT ( 'NONE',  ( -70.42518057789641261, -21.65701446794189522, 3.980077070345712009 ) ) ;
#34656 = ORIENTED_EDGE ( 'NONE', *, *, #24917, .T. ) ;
#34657 = CARTESIAN_POINT ( 'NONE',  ( 77.97077402951184411, 60.66921691151929963, -3.160174624583422354 ) ) ;
#34659 = CARTESIAN_POINT ( 'NONE',  ( 1.700390093233090871, -29.56993018339339940, 7.800000000000000711 ) ) ;
#34658 = CARTESIAN_POINT ( 'NONE',  ( -72.41848181666769335, -46.91894873934776200, 5.812054902733909678 ) ) ;
#34660 = CARTESIAN_POINT ( 'NONE',  ( 17.26911231124185520, 8.751764850756153180, -2.901660649865550390 ) ) ;
#34661 = CARTESIAN_POINT ( 'NONE',  ( 81.32870865761988455, 61.49729006283355659, -1.754135932968038825 ) ) ;
#34662 = PRODUCT_RELATED_PRODUCT_CATEGORY ( 'part', '', ( #15521 ) ) ;
#34663 = CARTESIAN_POINT ( 'NONE',  ( 77.77823160594134322, 63.95155898497984026, 3.535928464255528869 ) ) ;
#34664 = VERTEX_POINT ( 'NONE', #2374 ) ;
#34665 = DIRECTION ( 'NONE',  ( -0.000000000000000000, -0.000000000000000000, 1.000000000000000000 ) ) ;
#34666 = CARTESIAN_POINT ( 'NONE',  ( 0.5278090279835240262, -32.86766614071753168, 7.737115613922530777 ) ) ;
#34667 = CARTESIAN_POINT ( 'NONE',  ( 81.91393161461820682, 61.93681595580213184, 1.358135763685229591 ) ) ;
#34669 = CARTESIAN_POINT ( 'NONE',  ( -1.697333596569175151, -29.44509923219823122, 6.863904403958576594 ) ) ;
#34668 = DIRECTION ( 'NONE',  ( -0.000000000000000000, -0.000000000000000000, 1.000000000000000000 ) ) ;
#34670 = CARTESIAN_POINT ( 'NONE',  ( 28.96592479936138176, -0.01829609152130128036, -5.755841479376210934 ) ) ;
#34671 = CARTESIAN_POINT ( 'NONE',  ( 3.011115207906999380, -26.32487479661073948, 7.754798119455333705 ) ) ;
#34672 = CIRCLE ( 'NONE', #40554, 2.000000000000000000 ) ;
#34673 = CARTESIAN_POINT ( 'NONE',  ( -1.796417132220990531, -29.56955632736885420, 7.767581361668585593 ) ) ;
#34674 = CARTESIAN_POINT ( 'NONE',  ( 1.507917389220216231, -33.06463394440479675, 6.961115707816240672 ) ) ;
#34675 = VECTOR ( 'NONE', #12214, 1000.000000000000000 ) ;
#34676 = EDGE_CURVE ( 'NONE', #650, #20163, #21291, .T. ) ;
#34677 = CARTESIAN_POINT ( 'NONE',  ( 4.676936809477505008, -31.39751676666076463, 7.776484688137385248 ) ) ;
#34678 = ORIENTED_EDGE ( 'NONE', *, *, #38521, .T. ) ;
#34679 = CARTESIAN_POINT ( 'NONE',  ( 5.200390093233089317, -29.40819670640123462, 7.383456277641987420 ) ) ;
#34680 = EDGE_CURVE ( 'NONE', #27368, #7, #9940, .T. ) ;
#34681 = CARTESIAN_POINT ( 'NONE',  ( -71.92830462699674854, -0.6503483942891489233, 3.916091967151727804 ) ) ;
#34682 = CARTESIAN_POINT ( 'NONE',  ( 35.19026967813762496, -1.105067851863670958, -5.467017298376940282 ) ) ;
#34683 = FACE_OUTER_BOUND ( 'NONE', #39929, .T. ) ;
#34684 = DIRECTION ( 'NONE',  ( -0.000000000000000000, -0.000000000000000000, -1.000000000000000000 ) ) ;
#34685 = CARTESIAN_POINT ( 'NONE',  ( 26.27415342575414314, -2.868604062501628693, -4.307115103527353384 ) ) ;
#34686 = CARTESIAN_POINT ( 'NONE',  ( 6.433851184000642043, -31.40945003658912071, 7.013842709614101167 ) ) ;
#34687 = CARTESIAN_POINT ( 'NONE',  ( 2.082970273350142065, -32.94833696851883786, 6.959317978105167057 ) ) ;
#34688 = CARTESIAN_POINT ( 'NONE',  ( -64.08758708074093136, 37.05642372031412890, -4.717683440820351848 ) ) ;
#34689 = CARTESIAN_POINT ( 'NONE',  ( -1.490741356227917702, -28.39658077851778728, 7.775108481317161591 ) ) ;
#34690 = DIRECTION ( 'NONE',  ( 1.000000000000000000, 0.000000000000000000, 0.000000000000000000 ) ) ;
#34691 = ORIENTED_EDGE ( 'NONE', *, *, #3427, .T. ) ;
#34692 = CARTESIAN_POINT ( 'NONE',  ( -70.92837670882107659, -42.37473357531882812, 0.000000000000000000 ) ) ;
#34693 = CARTESIAN_POINT ( 'NONE',  ( 67.95937142815736820, 58.56762263466062279, -3.988335407916666409 ) ) ;
#34694 = AXIS2_PLACEMENT_3D ( 'NONE', #28976, #25883, #38422 ) ;
#34695 = ORIENTED_EDGE ( 'NONE', *, *, #624, .T. ) ;
#34696 = FACE_OUTER_BOUND ( 'NONE', #4430, .T. ) ;
#34697 = CARTESIAN_POINT ( 'NONE',  ( 0.07316740502934632184, -26.58460837109326391, 6.870716933885663735 ) ) ;
#34698 = CARTESIAN_POINT ( 'NONE',  ( 23.50817669065435922, 2.991962955900060450, 3.946939482339846705 ) ) ;
#34699 = CARTESIAN_POINT ( 'NONE',  ( 3.566793122297630791, -26.60908157518823458, 6.870724624169668893 ) ) ;
#34700 = VECTOR ( 'NONE', #10449, 1000.000000000000114 ) ;
#34701 = CARTESIAN_POINT ( 'NONE',  ( -40.44874870218063734, -26.64985754041175525, 6.800000000000000711 ) ) ;
#34702 = ORIENTED_EDGE ( 'NONE', *, *, #19594, .T. ) ;
#34703 = CARTESIAN_POINT ( 'NONE',  ( 24.77118930371659999, 3.025291850199358201, 3.323350240946416179 ) ) ;
#34704 = DIRECTION ( 'NONE',  ( 0.000000000000000000, 0.000000000000000000, -1.000000000000000000 ) ) ;
#34705 = VERTEX_POINT ( 'NONE', #19819 ) ;
#34706 = LINE ( 'NONE', #29705, #21267 ) ;
#34707 = ORIENTED_EDGE ( 'NONE', *, *, #8115, .T. ) ;
#34708 = CARTESIAN_POINT ( 'NONE',  ( 78.71580656266537801, 64.90148335848421368, -3.195657361810693597 ) ) ;
#34709 = B_SPLINE_CURVE_WITH_KNOTS ( 'NONE', 3,
 ( #33781, #7831, #17083, #4747, #36053, #26779 ),
 .UNSPECIFIED., .F., .F.,
 ( 4, 2, 4 ),
 ( 0.001123090053775944184, 0.001271523439455638860, 0.001419956825135333537 ),
 .UNSPECIFIED. ) ;
#34711 = CARTESIAN_POINT ( 'NONE',  ( 1.700390093233090871, -29.56993018339339940, 7.800000000000000711 ) ) ;
#34710 = CARTESIAN_POINT ( 'NONE',  ( 22.34894292866030696, 0.2931249150505332302, 6.995814783045894103 ) ) ;
#34712 = CARTESIAN_POINT ( 'NONE',  ( 78.68741431065086545, 66.05648362737333912, -1.057717897339662372 ) ) ;
#34713 = CARTESIAN_POINT ( 'NONE',  ( 78.80159527267854003, 65.27891740916035701, 2.934133054905261773 ) ) ;
#34714 = CARTESIAN_POINT ( 'NONE',  ( -1.585676428981071862, -30.76536307146522731, 7.767720160662275219 ) ) ;
#34715 = CARTESIAN_POINT ( 'NONE',  ( -12.87867591359218977, -24.55319635012989110, 6.700000000000000178 ) ) ;
#34716 = CARTESIAN_POINT ( 'NONE',  ( 22.33830324658017830, 5.012815666754769417, -5.469126444728273029 ) ) ;
#34717 = CARTESIAN_POINT ( 'NONE',  ( 21.85643539959777115, -15.24623503193425123, 0.9260495571226281530 ) ) ;
#34718 = ORIENTED_EDGE ( 'NONE', *, *, #14222, .T. ) ;
#34719 = CARTESIAN_POINT ( 'NONE',  ( -76.82502513205872674, 9.399367495309471465, 9.598227121387571614 ) ) ;
#34720 = ORIENTED_EDGE ( 'NONE', *, *, #7128, .F. ) ;
#34721 = CARTESIAN_POINT ( 'NONE',  ( -0.1008889408765406975, -32.55456798792236128, 7.784725160561911217 ) ) ;
#34722 = AXIS2_PLACEMENT_3D ( 'NONE', #22404, #25284, #40487 ) ;
#34723 = CARTESIAN_POINT ( 'NONE',  ( 1.725082688367724160, -32.96984567890832807, 7.740055089680399014 ) ) ;
#34724 = EDGE_CURVE ( 'NONE', #651, #28942, #29294, .T. ) ;
#34725 = CARTESIAN_POINT ( 'NONE',  ( 29.47129117146416633, -2.981296461931936204, -4.806105771814197958 ) ) ;
#34726 = CARTESIAN_POINT ( 'NONE',  ( 37.21234802891099491, -2.743797681025498481, -6.000906795383097680 ) ) ;
#34727 = CARTESIAN_POINT ( 'NONE',  ( -1.799609906766908685, -29.56993018339339940, 7.620413589471895399 ) ) ;
#34728 = CARTESIAN_POINT ( 'NONE',  ( 20.71699657508508707, 6.166998326322726598, 3.398385492444088385 ) ) ;
#34729 = CARTESIAN_POINT ( 'NONE',  ( -0.01129010125266571157, -26.63221833370405633, 7.635761828346577573 ) ) ;
#34730 = B_SPLINE_CURVE_WITH_KNOTS ( 'NONE', 3,
 ( #10779, #20869, #23947, #21085, #11583, #1960, #5026, #30144, #30557, #36322, #17971, #13886, #4631, #26452, #1541, #32839, #36125, #1748, #36521, #11382, #17159, #39389, #26653, #14478, #8092, #20659, #23359, #27247, #38980, #33241, #35928 ),
 .UNSPECIFIED., .F., .F.,
 ( 4, 3, 3, 3, 3, 3, 3, 3, 3, 3, 4 ),
 ( 9.697399036122160616E-19, 2.999644130997791255E-05, 6.002588995694985201E-05, 8.960886084588235714E-05, 0.0001190604700446521423, 0.0001489538463052733738, 0.0001796139255494002673, 0.0002109707048517114425, 0.0002426195318110404252, 0.0002740640997890113882, 0.0002849778069099895153 ),
 .UNSPECIFIED. ) ;
#34731 = DIRECTION ( 'NONE',  ( 1.000000000000000000, 0.000000000000000000, 0.000000000000000000 ) ) ;
#34732 = PRODUCT_DEFINITION_FORMATION_WITH_SPECIFIED_SOURCE ( 'ANY', '', #20310, .NOT_KNOWN. ) ;
#34733 = DIRECTION ( 'NONE',  ( -0.000000000000000000, -0.000000000000000000, 1.000000000000000000 ) ) ;
#34734 = CARTESIAN_POINT ( 'NONE',  ( 6.921324086407803833, -26.64985754041175525, 6.800000000000000711 ) ) ;
#34735 = CARTESIAN_POINT ( 'NONE',  ( 22.83184364098003627, 0.9670597066702968370, -5.845920663466038114 ) ) ;
#34736 = DIRECTION ( 'NONE',  ( 7.826543628040252284E-17, -1.000000000000000000, 0.000000000000000000 ) ) ;
#34737 = DIRECTION ( 'NONE',  ( -0.000000000000000000, 1.000000000000000000, -0.000000000000000000 ) ) ;
#34738 = ORIENTED_EDGE ( 'NONE', *, *, #26724, .F. ) ;
#34739 = ORIENTED_EDGE ( 'NONE', *, *, #7348, .F. ) ;
#34740 = CARTESIAN_POINT ( 'NONE',  ( 67.15438370417800229, 58.05139456359000150, 3.999036733496184048 ) ) ;
#34741 = CARTESIAN_POINT ( 'NONE',  ( 34.98297737265904317, -1.566505368433440015, 5.666337704145168352 ) ) ;
#34742 = CARTESIAN_POINT ( 'NONE',  ( 2.205779315586366973, -33.02853860453631540, 7.771081512783697853 ) ) ;
#34743 = CARTESIAN_POINT ( 'NONE',  ( 88.12503612275229159, -2.065192647045405838, -2.806263388478303256 ) ) ;
#34744 = CARTESIAN_POINT ( 'NONE',  ( 25.06963540266364632, 3.214953575097277749, 2.439413512043087984 ) ) ;
#34745 = CARTESIAN_POINT ( 'NONE',  ( -2.113887949235214947, -26.01735098123354106, 6.894806418505347700 ) ) ;
#34746 = AXIS2_PLACEMENT_3D ( 'NONE', #31453, #12499, #25068 ) ;
#34747 = VERTEX_POINT ( 'NONE', #3597 ) ;
#34748 = CARTESIAN_POINT ( 'NONE',  ( 24.44576246782188278, 2.805470990093293704, 3.838296511438501923 ) ) ;
#34749 = EDGE_CURVE ( 'NONE', #13546, #561, #35801, .T. ) ;
#34750 = DIRECTION ( 'NONE',  ( 0.000000000000000000, 0.000000000000000000, 1.000000000000000000 ) ) ;
#34751 = CARTESIAN_POINT ( 'NONE',  ( -12.99139449055068596, 10.37661300689600097, 6.000000000000000000 ) ) ;
#34752 = FACE_OUTER_BOUND ( 'NONE', #22117, .T. ) ;
#34753 = ORIENTED_EDGE ( 'NONE', *, *, #5858, .F. ) ;
#34754 = DIRECTION ( 'NONE',  ( 1.000000000000000000, 0.000000000000000000, 0.000000000000000000 ) ) ;
#34755 = AXIS2_PLACEMENT_3D ( 'NONE', #9822, #15384, #27941 ) ;
#34756 = ORIENTED_EDGE ( 'NONE', *, *, #26276, .T. ) ;
#34757 = CARTESIAN_POINT ( 'NONE',  ( 79.64740672574774294, 64.24900652125727163, -3.657510014241809326 ) ) ;
#34758 = ADVANCED_FACE ( 'NONE', ( #893 ), #26006, .F. ) ;
#34759 = PLANE ( 'NONE',  #9560 ) ;
#34760 = VECTOR ( 'NONE', #4113, 1000.000000000000000 ) ;
#34761 = CARTESIAN_POINT ( 'NONE',  ( 80.41811942164733296, 62.87504864752338563, 3.537885823842629396 ) ) ;
#34763 = ORIENTED_EDGE ( 'NONE', *, *, #40558, .T. ) ;
#34762 = CARTESIAN_POINT ( 'NONE',  ( -0.8221774698600063935, -27.29028943795776030, 6.863904403958576594 ) ) ;
#34764 = ADVANCED_FACE ( 'NONE', ( #13034 ), #1303, .F. ) ;
#34765 = CARTESIAN_POINT ( 'NONE',  ( -58.65342201553193746, 29.17550083397324912, 5.453968810494163044 ) ) ;
#34766 = CARTESIAN_POINT ( 'NONE',  ( 1.015685340855933649, -33.00230245371492543, 6.866770815808350470 ) ) ;
#34767 = CARTESIAN_POINT ( 'NONE',  ( -71.72859902172312729, -21.39704238849792262, 9.968370014334123397 ) ) ;
#34768 = LINE ( 'NONE', #164, #18889 ) ;
#34769 = VERTEX_POINT ( 'NONE', #18281 ) ;
#34770 = CARTESIAN_POINT ( 'NONE',  ( 3.121324086407806231, -24.55319635012989110, 6.700000000000000178 ) ) ;
#34771 = DIRECTION ( 'NONE',  ( -0.3420201433256663259, -0.9396926207859092051, 0.000000000000000000 ) ) ;
#34772 = CARTESIAN_POINT ( 'NONE',  ( -80.20775046477413639, -6.649906843095007680, -3.749433596971158078 ) ) ;
#34773 = ADVANCED_FACE ( 'NONE', ( #27351 ), #33754, .F. ) ;
#34774 = CARTESIAN_POINT ( 'NONE',  ( 5.007490259822573009, -30.35928972640521195, 6.988553391373222290 ) ) ;
#34775 = CARTESIAN_POINT ( 'NONE',  ( 81.25681022244552310, 61.36874951788873034, 1.439474762807428920 ) ) ;
#34776 = CARTESIAN_POINT ( 'NONE',  ( 87.32189673294487875, -1.771757446153727322, -4.160567758657673920 ) ) ;
#34777 =( BOUNDED_CURVE ( )  B_SPLINE_CURVE ( 3, ( #32181, #32579, #16302, #23101 ),
 .UNSPECIFIED., .F., .T. ) 
 B_SPLINE_CURVE_WITH_KNOTS ( ( 4, 4 ),
 ( 4.748221474220558846, 4.941946782021393147 ),
 .UNSPECIFIED. ) 
 CURVE ( )  GEOMETRIC_REPRESENTATION_ITEM ( )  RATIONAL_B_SPLINE_CURVE ( ( 1.000000000000000000, 0.9968749865767494445, 0.9968749865767494445, 1.000000000000000000 ) ) 
 REPRESENTATION_ITEM ( '' )  );
#34778 = CARTESIAN_POINT ( 'NONE',  ( 1.700390093233090871, -29.56993018339339940, 6.000000000000001776 ) ) ;
#34779 = ORIENTED_EDGE ( 'NONE', *, *, #17, .T. ) ;
#34780 = TOROIDAL_SURFACE ( 'NONE', #16975, 98.38357402481355507, 3.000000000000000000 ) ;
#34781 = CARTESIAN_POINT ( 'NONE',  ( -17.07867591359219617, -26.64985754041175525, 6.700000000000000178 ) ) ;
#34782 = CARTESIAN_POINT ( 'NONE',  ( 22.07327628326154922, 4.461839481733763435, -0.3963575452862883597 ) ) ;
#34783 = VERTEX_POINT ( 'NONE', #1496 ) ;
#34784 = CARTESIAN_POINT ( 'NONE',  ( -32.87867591359218977, -26.64985754041175525, 6.700000000000000178 ) ) ;
#34785 = CARTESIAN_POINT ( 'NONE',  ( 15.30049896279744992, -3.947521880118775250, -2.581831727127946063 ) ) ;
#34786 = DIRECTION ( 'NONE',  ( -0.000000000000000000, -0.000000000000000000, -1.000000000000000000 ) ) ;
#34787 = CARTESIAN_POINT ( 'NONE',  ( 5.021324086407805254, -26.64985754041175525, 6.700000000000000178 ) ) ;
#34788 = CARTESIAN_POINT ( 'NONE',  ( 34.13633707975591136, -3.132998035770167888, 5.534199010363774818 ) ) ;
#34789 = EDGE_CURVE ( 'NONE', #2601, #2179, #1386, .T. ) ;
#34790 = CARTESIAN_POINT ( 'NONE',  ( 87.10491796770416784, 0.5173464865745804886, -5.275911943831619766 ) ) ;
#34791 = ORIENTED_EDGE ( 'NONE', *, *, #80, .T. ) ;
#34793 = CARTESIAN_POINT ( 'NONE',  ( 5.551251297819359110, -26.64985754041175525, 6.800000000000000711 ) ) ;
#34792 = CARTESIAN_POINT ( 'NONE',  ( 81.11573943753921867, 62.50280337846361789, -3.122598816540624433 ) ) ;
#34794 = CARTESIAN_POINT ( 'NONE',  ( 5.200371613545275551, -29.55750178647830850, 7.756555456908253987 ) ) ;
#34795 = ORIENTED_EDGE ( 'NONE', *, *, #39213, .F. ) ;
#34796 = DIRECTION ( 'NONE',  ( -0.000000000000000000, -0.000000000000000000, 1.000000000000000000 ) ) ;
#34797 = VERTEX_POINT ( 'NONE', #38436 ) ;
#34798 = CARTESIAN_POINT ( 'NONE',  ( -80.93405938708093572, -6.594533268907218471, 0.2501301618973993945 ) ) ;
#34799 = ORIENTED_EDGE ( 'NONE', *, *, #25735, .F. ) ;
#34800 = CIRCLE ( 'NONE', #38691, 0.1000000000000028644 ) ;
#34801 = CARTESIAN_POINT ( 'NONE',  ( 78.88238753611517495, 65.83802744495456238, -2.215902410107950526 ) ) ;
#34802 = EDGE_CURVE ( 'NONE', #38060, #4188, #13935, .T. ) ;
#34803 = CARTESIAN_POINT ( 'NONE',  ( 5.151091795598730094, -30.15529994797888946, 7.742274884880762542 ) ) ;
#34804 = EDGE_CURVE ( 'NONE', #19388, #34205, #794, .T. ) ;
#34806 = CARTESIAN_POINT ( 'NONE',  ( 4.582084150952498547, -31.37432464074042215, 7.754798119455333705 ) ) ;
#34805 = CARTESIAN_POINT ( 'NONE',  ( 22.26710026944065746, 2.334480711795404506, 5.248520767630765249 ) ) ;
#34808 = ORIENTED_EDGE ( 'NONE', *, *, #6574, .T. ) ;
#34807 = VERTEX_POINT ( 'NONE', #26506 ) ;
#34809 = EDGE_CURVE ( 'NONE', #26136, #212, #38843, .T. ) ;
#34810 = CARTESIAN_POINT ( 'NONE',  ( 78.68916368339945677, 66.05772639262713142, -1.037317649801933639 ) ) ;
#34811 = CARTESIAN_POINT ( 'NONE',  ( 4.676599318385033399, -27.92608080218391109, 6.880147297696981745 ) ) ;
#34813 = CARTESIAN_POINT ( 'NONE',  ( 1.300000000000000044, -0.5999999999999994227, -4.250000000000000000 ) ) ;
#34812 = CARTESIAN_POINT ( 'NONE',  ( -59.01729896555999488, 27.93936864455021762, -6.195187712944653313 ) ) ;
#34814 = PLANE ( 'NONE',  #29704 ) ;
#34815 = CARTESIAN_POINT ( 'NONE',  ( -89.00859394718985129, 2.429809908903242555, 12.50000000000000000 ) ) ;
#34816 = CARTESIAN_POINT ( 'NONE',  ( 71.13429564674895289, 59.00621471515203353, 3.925556587156296739 ) ) ;
#34817 = B_SPLINE_CURVE_WITH_KNOTS ( 'NONE', 3,
 ( #37922, #32334, #34673, #31157, #34875, #7196, #22308, #19756, #16643, #23057, #29228, #2973, #32527 ),
 .UNSPECIFIED., .F., .F.,
 ( 4, 3, 3, 3, 4 ),
 ( 2.475319317933450300E-05, 2.546128104244953829E-05, 5.711050680483697561E-05, 8.113074941675614072E-05, 8.388765757908052086E-05 ),
 .UNSPECIFIED. ) ;
#34818 = VERTEX_POINT ( 'NONE', #32890 ) ;
#34819 = CARTESIAN_POINT ( 'NONE',  ( 24.35198760066796808, 2.925641703088587064, -3.745929113794717491 ) ) ;
#34820 = ORIENTED_EDGE ( 'NONE', *, *, #9733, .F. ) ;
#34821 = ORIENTED_EDGE ( 'NONE', *, *, #22982, .F. ) ;
#34822 = VECTOR ( 'NONE', #5585, 1000.000000000000000 ) ;
#34823 = CARTESIAN_POINT ( 'NONE',  ( 21.85643539959779247, -13.31640034840845388, 0.8419676367911695936 ) ) ;
#34824 = CARTESIAN_POINT ( 'NONE',  ( -59.00110696496997775, 28.68040728033255249, -6.999999999999999112 ) ) ;
#34825 = CARTESIAN_POINT ( 'NONE',  ( -28.44874870218064444, -26.64985754041175525, 6.800000000000000711 ) ) ;
#34826 = CARTESIAN_POINT ( 'NONE',  ( 81.62235710223406215, 64.17388774702372700, 3.017922835037552431 ) ) ;
#34827 = CARTESIAN_POINT ( 'NONE',  ( 85.02879235234962607, 2.798117532367836446, 2.624272742801059710 ) ) ;
#34828 = ORIENTED_EDGE ( 'NONE', *, *, #39880, .F. ) ;
#34829 = CARTESIAN_POINT ( 'NONE',  ( 0.5551755531694614332, -32.77125548039569480, 7.748216051605118615 ) ) ;
#34830 = CARTESIAN_POINT ( 'NONE',  ( 14.74375015214041973, -5.597190475337525228, 2.503889630996063875 ) ) ;
#34831 = CARTESIAN_POINT ( 'NONE',  ( 33.46254251190648432, -3.085782718482933618, -5.429037072268634745 ) ) ;
#34832 = CARTESIAN_POINT ( 'NONE',  ( 5.100168698360202590, -29.60992969820402010, 7.784838882742139532 ) ) ;
#34833 = CARTESIAN_POINT ( 'NONE',  ( -1.348152954782936730, -27.85051585561017973, 7.710604733652631104 ) ) ;
#34834 = CARTESIAN_POINT ( 'NONE',  ( -72.91754375945518518, 1.351626832663766820, 10.95472414578862441 ) ) ;
#34835 = EDGE_LOOP ( 'NONE', ( #26949, #3545, #32011, #22168 ) ) ;
#34836 = LINE ( 'NONE', #31725, #39474 ) ;
#34837 = CARTESIAN_POINT ( 'NONE',  ( -1.303108374136985104, -31.16335321463953534, 7.754798119455333705 ) ) ;
#34838 = CARTESIAN_POINT ( 'NONE',  ( 28.66061354658119953, -3.315359872734950031, 4.679579922280550086 ) ) ;
#34839 = VERTEX_POINT ( 'NONE', #3907 ) ;
#34840 = CARTESIAN_POINT ( 'NONE',  ( 33.11155473229664636, -0.1547796613981889668, 4.947169480470523517 ) ) ;
#34841 = DIRECTION ( 'NONE',  ( 0.000000000000000000, 0.000000000000000000, 1.000000000000000000 ) ) ;
#34842 = CARTESIAN_POINT ( 'NONE',  ( 66.54830849220104483, 57.89461212714910943, -3.999444518117950764 ) ) ;
#34843 = EDGE_CURVE ( 'NONE', #25652, #1802, #15141, .T. ) ;
#34844 = AXIS2_PLACEMENT_3D ( 'NONE', #5839, #22103, #12814 ) ;
#34845 = CARTESIAN_POINT ( 'NONE',  ( -0.5390219559468002464, -26.88736040713764908, 7.773839561854632763 ) ) ;
#34846 = ORIENTED_EDGE ( 'NONE', *, *, #5494, .T. ) ;
#34847 = CARTESIAN_POINT ( 'NONE',  ( 87.76685765732969458, -0.2261755903657670097, -3.756757151743586931 ) ) ;
#34848 = EDGE_CURVE ( 'NONE', #25004, #33375, #32296, .T. ) ;
#34849 = DIRECTION ( 'NONE',  ( 0.000000000000000000, 0.000000000000000000, 1.000000000000000000 ) ) ;
#34850 = CARTESIAN_POINT ( 'NONE',  ( -4.890026461918812295, -8.951974136083761024, 6.000000000000000000 ) ) ;
#34851 = ORIENTED_EDGE ( 'NONE', *, *, #33189, .F. ) ;
#34852 = FACE_BOUND ( 'NONE', #36381, .T. ) ;
#34853 = EDGE_LOOP ( 'NONE', ( #20373, #37967, #10500, #3136 ) ) ;
#34854 = CARTESIAN_POINT ( 'NONE',  ( 24.58106864520391710, 2.978418058025279258, 3.576134102654449087 ) ) ;
#34855 = EDGE_CURVE ( 'NONE', #3598, #39064, #33927, .T. ) ;
#34856 = CARTESIAN_POINT ( 'NONE',  ( 82.47906632153704720, 63.16918237499279343, -1.623788564014418068 ) ) ;
#34857 = CARTESIAN_POINT ( 'NONE',  ( 78.99368969759480308, 65.72941799158938636, 2.506402126386323648 ) ) ;
#34858 = AXIS2_PLACEMENT_3D ( 'NONE', #31855, #38613, #35160 ) ;
#34859 = CARTESIAN_POINT ( 'NONE',  ( -24.44874870218064089, -26.64985754041175525, 6.700000000000000178 ) ) ;
#34860 = ORIENTED_EDGE ( 'NONE', *, *, #20970, .F. ) ;
#34861 = CARTESIAN_POINT ( 'NONE',  ( 76.45598340902211021, 62.40619074383518949, -3.848392762312481175 ) ) ;
#34863 = CARTESIAN_POINT ( 'NONE',  ( 1.825008882942001920, -26.07214915268203725, 7.751599049952198506 ) ) ;
#34862 = CARTESIAN_POINT ( 'NONE',  ( 2.337381470057465549, -33.01147775668546558, 7.660770905198779346 ) ) ;
#34864 = CARTESIAN_POINT ( 'NONE',  ( 16.86596627815397653, 9.683932516527400836, -2.782816404980593905 ) ) ;
#34865 = CARTESIAN_POINT ( 'NONE',  ( 81.32112198246268520, 62.31825444738111486, -2.836177733672716972 ) ) ;
#34866 = CARTESIAN_POINT ( 'NONE',  ( 77.57451768555486638, 61.52186891572913652, 3.722835383490897598 ) ) ;
#34867 = ORIENTED_EDGE ( 'NONE', *, *, #38798, .T. ) ;
#34868 = DIRECTION ( 'NONE',  ( 0.7126435865141269588, 0.000000000000000000, -0.7015262779114422864 ) ) ;
#34869 = CARTESIAN_POINT ( 'NONE',  ( -58.99290877059915772, 28.70988844028545373, 6.739549407909634304 ) ) ;
#34870 = CARTESIAN_POINT ( 'NONE',  ( 82.10888692569093905, 64.42619117010492857, 2.360008641314786715 ) ) ;
#34872 = DIRECTION ( 'NONE',  ( 0.7864880931482275406, 0.000000000000000000, 0.6176054398530382850 ) ) ;
#34871 = CARTESIAN_POINT ( 'NONE',  ( -70.92837670882107659, -31.30579396504363388, 0.000000000000000000 ) ) ;
#34873 = CARTESIAN_POINT ( 'NONE',  ( 29.67594332454466866, -2.985454744488035494, -5.114964129314456542 ) ) ;
#34874 = CARTESIAN_POINT ( 'NONE',  ( -1.422192660794930674, -31.15090360007274839, 6.951256099901591767 ) ) ;
#34875 = CARTESIAN_POINT ( 'NONE',  ( -1.794043895342124495, -29.56109672522452669, 7.773839561854631874 ) ) ;
#34876 = CARTESIAN_POINT ( 'NONE',  ( -62.78278205347341867, 35.70412497698344367, 5.569918731383189048 ) ) ;
#34877 = VECTOR ( 'NONE', #33268, 1000.000000000000114 ) ;
#34878 = DIRECTION ( 'NONE',  ( 0.000000000000000000, 0.000000000000000000, -1.000000000000000000 ) ) ;
#34879 = CARTESIAN_POINT ( 'NONE',  ( -0.6205797297147237490, -32.05451548273851614, 6.887945620086118659 ) ) ;
#34880 = B_SPLINE_CURVE_WITH_KNOTS ( 'NONE', 3,
 ( #8778, #36191, #40282, #2652, #14751, #2231, #11659, #36795, #40085, #27321, #36595, #24233, #14349, #39883, #8580, #5504, #5713, #11863, #24021, #15170, #33725, #8164, #33530, #11250, #12072, #18047, #7972, #20524, #30639, #2447, #36999 ),
 .UNSPECIFIED., .F., .F.,
 ( 4, 3, 3, 3, 3, 3, 3, 3, 3, 3, 4 ),
 ( 1.939479807224432123E-18, 2.999644130997642855E-05, 6.002588995694698565E-05, 8.960886084587837269E-05, 0.0001190604700446467484, 0.0001489538463052699857, 0.0001796139255493966894, 0.0002109707048517059944, 0.0002426195318110339471, 0.0002740640997890056961, 0.0002849778069099870217 ),
 .UNSPECIFIED. ) ;
#34881 = FACE_OUTER_BOUND ( 'NONE', #38260, .T. ) ;
#34882 = FACE_OUTER_BOUND ( 'NONE', #19925, .T. ) ;
#34883 = CARTESIAN_POINT ( 'NONE',  ( 37.09992950587152194, -2.920862267133551793, -5.996321585650099095 ) ) ;
#34884 = CARTESIAN_POINT ( 'NONE',  ( 80.71264223670345928, 61.13836533427188158, -1.655461010748698669 ) ) ;
#34885 = CARTESIAN_POINT ( 'NONE',  ( -0.9006766493021783893, -31.75956955190471120, 7.763628509615291939 ) ) ;
#34886 = CARTESIAN_POINT ( 'NONE',  ( -12.87867591359218977, -24.55319635012989110, 6.700000000000000178 ) ) ;
#34887 = DIRECTION ( 'NONE',  ( 0.4999999999999927836, 0.8660254037844429265, 0.000000000000000000 ) ) ;
#34888 = CARTESIAN_POINT ( 'NONE',  ( -77.33993978126859759, 9.671531369715314241, 9.242830849232364088 ) ) ;
#34889 = CARTESIAN_POINT ( 'NONE',  ( -64.08758708074093136, 36.87876644325631759, -4.900609702795900802 ) ) ;
#34890 = CARTESIAN_POINT ( 'NONE',  ( 21.92337503799926424, -12.52192678573947582, 2.500000000000000444 ) ) ;
#34891 = CIRCLE ( 'NONE', #17079, 0.1000000000000028644 ) ;
#34892 = EDGE_LOOP ( 'NONE', ( #22780, #11489, #36889, #24111 ) ) ;
#34893 = VERTEX_POINT ( 'NONE', #29191 ) ;
#34894 = CARTESIAN_POINT ( 'NONE',  ( -1.510909903798922427, -30.68686900403765705, 6.894806418505348589 ) ) ;
#34895 = B_SPLINE_CURVE_WITH_KNOTS ( 'NONE', 3,
 ( #37932, #35085, #31574, #9741, #10339, #32192, #25796, #16701, #38329, #3992, #3399, #35284, #19814, #15915, #28474, #7051, #16512, #29087, #13424, #22911, #7251, #32390, #4184, #1101, #26208 ),
 .UNSPECIFIED., .F., .F.,
 ( 4, 3, 3, 3, 3, 3, 3, 3, 4 ),
 ( 6.468151674593725878E-05, 9.076621574722179618E-05, 0.0001210204262067967739, 0.0001512763324577452186, 0.0001815301820994223248, 0.0002117781465860755575, 0.0002420274594459800323, 0.0002722905548971162764, 0.0002816827545175597637 ),
 .UNSPECIFIED. ) ;
#34896 = CARTESIAN_POINT ( 'NONE',  ( 68.06744372826909739, 58.27867795456629807, -3.994255761866621235 ) ) ;
#34897 = EDGE_LOOP ( 'NONE', ( #6538, #2522, #6499, #17532 ) ) ;
#34898 = CARTESIAN_POINT ( 'NONE',  ( -0.9174058041325571233, -27.26220320217948867, 7.780491323090171996 ) ) ;
#34899 = CARTESIAN_POINT ( 'NONE',  ( 30.85955166002529282, -3.509934588350169360, 4.878265527032272786 ) ) ;
#34900 = CARTESIAN_POINT ( 'NONE',  ( 22.43458216738055100, 3.371505658154835494, 4.287311446981358465 ) ) ;
#34901 = CARTESIAN_POINT ( 'NONE',  ( 3.589445461969659856, -26.62348856653665052, 6.887547729233690852 ) ) ;
#34903 = EDGE_CURVE ( 'NONE', #2062, #9255, #39036, .T. ) ;
#34902 = DIRECTION ( 'NONE',  ( -1.000000000000000000, 0.000000000000000000, 0.000000000000000000 ) ) ;
#34904 = ORIENTED_EDGE ( 'NONE', *, *, #28741, .F. ) ;
#34905 = CARTESIAN_POINT ( 'NONE',  ( 23.14179388839477269, 4.049790476811788942, 3.073817882771325838 ) ) ;
#34906 = ADVANCED_FACE ( 'NONE', ( #10041 ), #6962, .F. ) ;
#34907 = LINE ( 'NONE', #16140, #1132 ) ;
#34908 = CARTESIAN_POINT ( 'NONE',  ( 78.66413930541318678, 66.03995068206980079, 1.171933751919278732 ) ) ;
#34909 = ORIENTED_EDGE ( 'NONE', *, *, #30743, .F. ) ;
#34910 = EDGE_CURVE ( 'NONE', #4144, #1810, #13537, .T. ) ;
#34911 = CARTESIAN_POINT ( 'NONE',  ( 4.372846383550529126, -27.30984669459420289, 7.635761828346578461 ) ) ;
#34912 = VERTEX_POINT ( 'NONE', #10440 ) ;
#34913 = CARTESIAN_POINT ( 'NONE',  ( 79.10818533696262023, 64.58014521944367914, -3.489618106120226049 ) ) ;
#34915 = CARTESIAN_POINT ( 'NONE',  ( -1.665924965603348351, -30.04734292374604010, 6.864276522220859711 ) ) ;
#34914 = CARTESIAN_POINT ( 'NONE',  ( 26.64323651376993496, 1.020623712725687415, 4.378694421187283581 ) ) ;
#34916 = CARTESIAN_POINT ( 'NONE',  ( 81.65270467917648034, 63.44102909743352825, -3.019969592843240846 ) ) ;
#34917 = CARTESIAN_POINT ( 'NONE',  ( 80.10726245975679660, 62.76215410473258771, 3.584461231902855705 ) ) ;
#34918 = CIRCLE ( 'NONE', #5284, 0.1000000000000028644 ) ;
#34919 = DIRECTION ( 'NONE',  ( 0.000000000000000000, 0.000000000000000000, 1.000000000000000000 ) ) ;
#34920 = CARTESIAN_POINT ( 'NONE',  ( 24.76528640762570888, -1.939968142380837701, -6.533370004292007316 ) ) ;
#34921 = DIRECTION ( 'NONE',  ( 1.000000000000000000, -7.930164461608261228E-15, 0.000000000000000000 ) ) ;
#34922 = ORIENTED_EDGE ( 'NONE', *, *, #11645, .F. ) ;
#34923 = CARTESIAN_POINT ( 'NONE',  ( -75.71907068449459643, 8.624194553058243784, 8.809091513226231740 ) ) ;
#34924 = LINE ( 'NONE', #9976, #12762 ) ;
#34925 = DIRECTION ( 'NONE',  ( 0.9396926207859082059, 0.3420201433256695456, -0.000000000000000000 ) ) ;
#34926 = CARTESIAN_POINT ( 'NONE',  ( -81.80172258451945311, 10.46396458320884371, -1.097114612388527588 ) ) ;
#34927 = CARTESIAN_POINT ( 'NONE',  ( 32.89342118928954761, -3.693192685043988011, -5.116248522870010973 ) ) ;
#34928 = CARTESIAN_POINT ( 'NONE',  ( 34.79218682057849321, -3.833549442645881378, -5.378504871664683940 ) ) ;
#34929 = CARTESIAN_POINT ( 'NONE',  ( 3.385812859895339422, -32.63741323173702824, 6.867280401193709416 ) ) ;
#34930 = CARTESIAN_POINT ( 'NONE',  ( -1.004988036239387261, -31.79051028124264988, 6.887161170156904433 ) ) ;
#34931 = CARTESIAN_POINT ( 'NONE',  ( 5.196299276553091318, -29.73910164073445017, 7.013842709614101167 ) ) ;
#34932 = DIRECTION ( 'NONE',  ( 0.000000000000000000, 0.000000000000000000, 1.000000000000000000 ) ) ;
#34933 = CARTESIAN_POINT ( 'NONE',  ( 0.06066625181903905623, -26.47779407321028700, 7.750000000000000888 ) ) ;
#34934 = VECTOR ( 'NONE', #36270, 1000.000000000000000 ) ;
#34935 = CARTESIAN_POINT ( 'NONE',  ( 1.700390093233090871, -29.56993018339339940, 7.800000000000000711 ) ) ;
#34936 = CARTESIAN_POINT ( 'NONE',  ( 23.18106065147113526, 1.013842311355323433, -5.509883555410340250 ) ) ;
#34937 = CARTESIAN_POINT ( 'NONE',  ( 32.24397170968010329, 0.1813167479581142549, -4.768898611949658140 ) ) ;
#34938 = CARTESIAN_POINT ( 'NONE',  ( 18.51265066094652667, 11.53724448403076863, -2.500000000000001332 ) ) ;
#34939 = VERTEX_POINT ( 'NONE', #7358 ) ;
#34940 = CARTESIAN_POINT ( 'NONE',  ( 66.72344311391505300, 57.86780257000127392, 3.999628797551961767 ) ) ;
#34941 = DIRECTION ( 'NONE',  ( -0.000000000000000000, 0.000000000000000000, 1.000000000000000000 ) ) ;
#34942 = CARTESIAN_POINT ( 'NONE',  ( 86.96369117609759769, -0.5876503451053297633, 5.665127693518188678 ) ) ;
#34943 = CIRCLE ( 'NONE', #2728, 10.00000000000000888 ) ;
#34944 = EDGE_LOOP ( 'NONE', ( #23313, #14509, #14543, #34079 ) ) ;
#34945 = CARTESIAN_POINT ( 'NONE',  ( 25.54921697257007196, 2.203847488687706857, 4.114390114421843769 ) ) ;
#34946 = CARTESIAN_POINT ( 'NONE',  ( 0.000000000000000000, 0.000000000000000000, 0.000000000000000000 ) ) ;
#34947 = DIRECTION ( 'NONE',  ( 0.000000000000000000, 0.000000000000000000, 1.000000000000000000 ) ) ;
#34948 = DIRECTION ( 'NONE',  ( 1.000000000000000000, 0.000000000000000000, 0.000000000000000000 ) ) ;
#34949 = EDGE_LOOP ( 'NONE', ( #18150, #5981, #12865, #30667, #6155, #16426, #9893, #22028 ) ) ;
#34950 = CARTESIAN_POINT ( 'NONE',  ( -18.97867591359219475, -26.64985754041175525, 6.700000000000000178 ) ) ;
#34951 = ORIENTED_EDGE ( 'NONE', *, *, #39024, .F. ) ;
#34952 = ADVANCED_FACE ( 'NONE', ( #4286 ), #1211, .F. ) ;
#34953 = EDGE_LOOP ( 'NONE', ( #9772, #15665, #997, #23936, #2695 ) ) ;
#34954 = CARTESIAN_POINT ( 'NONE',  ( 78.67256861866690087, 65.85712333569000521, -2.031354376635688297 ) ) ;
#34955 = DIRECTION ( 'NONE',  ( -0.000000000000000000, -0.000000000000000000, 1.000000000000000000 ) ) ;
#34956 = CARTESIAN_POINT ( 'NONE',  ( 80.72421460287552009, 62.36539998118918504, 3.243225924683090344 ) ) ;
#34959 = ORIENTED_EDGE ( 'NONE', *, *, #2630, .T. ) ;
#34958 = EDGE_LOOP ( 'NONE', ( #36031, #25270, #24813, #13979 ) ) ;
#34957 = DIRECTION ( 'NONE',  ( 1.000000000000000000, 0.000000000000000000, 0.000000000000000000 ) ) ;
#34960 = CIRCLE ( 'NONE', #38209, 0.1000000000000028644 ) ;
#34961 = B_SPLINE_CURVE_WITH_KNOTS ( 'NONE', 3,
 ( #9263, #2515, #8852, #15446, #5784, #18322 ),
 .UNSPECIFIED., .F., .F.,
 ( 4, 2, 4 ),
 ( 0.0009802349148204147003, 0.003915514348654383289, 0.006850793782488352746 ),
 .UNSPECIFIED. ) ;
#34962 = LINE ( 'NONE', #34354, #32422 ) ;
#34963 = CARTESIAN_POINT ( 'NONE',  ( -0.5270797881493830550, -32.26962978289218853, 7.730015791551952731 ) ) ;
#34964 = CARTESIAN_POINT ( 'NONE',  ( 1.822194502883780931, -26.07228119081829476, 7.754798119455333705 ) ) ;
#34965 = CARTESIAN_POINT ( 'NONE',  ( 33.87323733507539458, -5.307943772420733453, -1.870510103425834458 ) ) ;
#34966 = CARTESIAN_POINT ( 'NONE',  ( 21.84352692530194773, 5.886300334905539167, -3.168733228457595086 ) ) ;
#34967 = ORIENTED_EDGE ( 'NONE', *, *, #3095, .F. ) ;
#34968 = CARTESIAN_POINT ( 'NONE',  ( -1.799566460562916470, -29.58736926422850999, 7.749999999999998224 ) ) ;
#34969 = ORIENTED_EDGE ( 'NONE', *, *, #13798, .T. ) ;
#34970 = CARTESIAN_POINT ( 'NONE',  ( -1.752826142657526676, -30.14031989453273752, 6.887161170156907097 ) ) ;
#34971 = CARTESIAN_POINT ( 'NONE',  ( -0.5679913539545495826, -32.21827145269413251, 7.783750581861601070 ) ) ;
#34972 = AXIS2_PLACEMENT_3D ( 'NONE', #7198, #23257, #32732 ) ;
#34973 = CARTESIAN_POINT ( 'NONE',  ( -81.58461690839780545, -5.624039435740707304, -2.430449384178134942 ) ) ;
#34974 = DIRECTION ( 'NONE',  ( 0.000000000000000000, 1.000000000000000000, 0.000000000000000000 ) ) ;
#34975 = CYLINDRICAL_SURFACE ( 'NONE', #33297, 6.329987104167475565 ) ;
#34976 = CARTESIAN_POINT ( 'NONE',  ( 78.67529526371438919, 66.04787469174290493, 1.130345937366638465 ) ) ;
#34977 = FACE_OUTER_BOUND ( 'NONE', #35239, .T. ) ;
#34978 = CARTESIAN_POINT ( 'NONE',  ( 21.71191031684054806, 6.329465815346970281, -3.192820326339156800 ) ) ;
#34979 = ORIENTED_EDGE ( 'NONE', *, *, #24838, .T. ) ;
#34980 = CARTESIAN_POINT ( 'NONE',  ( -1.576323396845137781, -30.80003141911850051, 7.710604733652623999 ) ) ;
#34981 = DIRECTION ( 'NONE',  ( -1.000000000000000000, 0.000000000000000000, 0.000000000000000000 ) ) ;
#34982 = EDGE_CURVE ( 'NONE', #38489, #32700, #7557, .T. ) ;
#34983 = CARTESIAN_POINT ( 'NONE',  ( -63.58520484588292732, 35.72026407271188475, 6.999999999999987566 ) ) ;
#34984 = DIRECTION ( 'NONE',  ( 0.000000000000000000, -1.000000000000000000, 0.000000000000000000 ) ) ;
#34985 = DIRECTION ( 'NONE',  ( 0.000000000000000000, 0.000000000000000000, 1.000000000000000000 ) ) ;
#34986 = DIRECTION ( 'NONE',  ( 0.000000000000000000, -1.332267629550187849E-14, 1.000000000000000000 ) ) ;
#34987 = CARTESIAN_POINT ( 'NONE',  ( 36.89687251559261227, -3.001234578891534444, 5.965047328928867465 ) ) ;
#34988 = EDGE_CURVE ( 'NONE', #17567, #7963, #26899, .T. ) ;
#34989 = CARTESIAN_POINT ( 'NONE',  ( 85.06303677129686491, 2.810884359907178442, 0.2996589496366894867 ) ) ;
#34990 = ORIENTED_EDGE ( 'NONE', *, *, #24548, .T. ) ;
#34992 = CARTESIAN_POINT ( 'NONE',  ( 0.000000000000000000, 0.5999999999999995337, 3.730072921939604047 ) ) ;
#34991 = CARTESIAN_POINT ( 'NONE',  ( 78.76190985582823600, 66.07042273533498644, -1.483717294826052635 ) ) ;
#34993 = CARTESIAN_POINT ( 'NONE',  ( -0.8954611659357714082, -31.76573441880953297, 7.635761828346577573 ) ) ;
#34994 = DIRECTION ( 'NONE',  ( -0.7394003126383923430, -0.1303762246624306231, 0.6605219282605377940 ) ) ;
#34995 = ORIENTED_EDGE ( 'NONE', *, *, #14719, .T. ) ;
#34996 = CARTESIAN_POINT ( 'NONE',  ( -1.654012860102806792, -29.01496998062980381, 7.703977250142846955 ) ) ;
#34997 = ORIENTED_EDGE ( 'NONE', *, *, #635, .T. ) ;
#34998 = CARTESIAN_POINT ( 'NONE',  ( -80.93573588528884954, -6.594316608410932368, -0.1743350153730407748 ) ) ;
#34999 = AXIS2_PLACEMENT_3D ( 'NONE', #5307, #11662, #36194 ) ;
#35001 = ORIENTED_EDGE ( 'NONE', *, *, #20917, .F. ) ;
#35000 = ORIENTED_EDGE ( 'NONE', *, *, #25028, .T. ) ;
#35002 = ADVANCED_FACE ( 'NONE', ( #4870 ), #5282, .F. ) ;
#35003 = CARTESIAN_POINT ( 'NONE',  ( 81.10500554505480864, 61.42844135377572456, -1.938154327158297940 ) ) ;
#35004 = CARTESIAN_POINT ( 'NONE',  ( -1.499157785959173594, -28.41975916621540321, 7.635761828346577573 ) ) ;
#35005 = CARTESIAN_POINT ( 'NONE',  ( 21.99376790462624953, 1.189524801706998369, 6.708885966919416077 ) ) ;
#35006 = ORIENTED_EDGE ( 'NONE', *, *, #35682, .F. ) ;
#35007 = CARTESIAN_POINT ( 'NONE',  ( 81.70897365440940519, 61.83459377731552564, -1.744953761006742265 ) ) ;
#35008 = CARTESIAN_POINT ( 'NONE',  ( 4.670146650652899467, -27.91446891051451118, 6.892063359921934307 ) ) ;
#35009 =( BOUNDED_SURFACE ( )  B_SPLINE_SURFACE ( 3, 2, ( 
 ( #24949, #18542, #19170 ),
 ( #15672, #2945, #15462 ),
 ( #40568, #3357, #25353 ),
 ( #28021, #6622, #37483 ),
 ( #26116, #9279, #34432 ),
 ( #3550, #38649, #13543 ),
 ( #28219, #6211, #18756 ),
 ( #31331, #25145, #9481 ),
 ( #12578, #16819, #26711 ),
 ( #14533, #27107, #10643 ),
 ( #5085, #32696, #8356 ),
 ( #35785, #23802, #17411 ),
 ( #39245, #17016, #26904 ),
 ( #32493, #8148, #10843 ),
 ( #24004, #30196, #7763 ),
 ( #36179, #1809, #1217 ),
 ( #14334, #23221, #7960 ),
 ( #26511, #36579, #39657 ),
 ( #11439, #29995, #14135 ),
 ( #20117, #23613, #36379 ),
 ( #11036, #4496, #4295 ),
 ( #20509, #33093, #4876 ) ),
 .UNSPECIFIED., .F., .F., .T. ) 
 B_SPLINE_SURFACE_WITH_KNOTS ( ( 4, 2, 2, 2, 2, 2, 2, 2, 2, 2, 4 ),
 ( 3, 3 ),
 ( 0.02037793668903936650, 0.02161998616042463614, 0.02224101089611726922, 0.02286203563180990578, 0.02410408510319517195, 0.02534613457458044158, 0.02658818404596571122, 0.02720920878165834431, 0.02783023351735097739, 0.02907228298873624703, 0.03031433246012151667 ),
 ( 0.000000000000000000, 0.8973666424348171189 ),
 .UNSPECIFIED. ) 
 GEOMETRIC_REPRESENTATION_ITEM ( )  RATIONAL_B_SPLINE_SURFACE ( (
 ( 1.000000000000000000, 0.7371673956414459550, 0.9460492146741605879),
 ( 1.000000000000000000, 0.7430206879744455373, 0.9472507007640531551),
 ( 1.000000000000000000, 0.7496157519951666126, 0.9486044478916609846),
 ( 1.000000000000000000, 0.7607417901526166704, 0.9508882531966559304),
 ( 1.000000000000000000, 0.7646561537746499049, 0.9516917417591763684),
 ( 1.000000000000000000, 0.7729170770629312237, 0.9533874343465059686),
 ( 1.000000000000000000, 0.7772865941316164928, 0.9542843507619009902),
 ( 1.000000000000000000, 0.7908687655009780659, 0.9570723184632274894),
 ( 1.000000000000000000, 0.8005515303433323737, 0.9590598677957974383),
 ( 1.000000000000000000, 0.8209981033988819066, 0.9632568686825830895),
 ( 1.000000000000000000, 0.8318680535256515185, 0.9654881076387360483),
 ( 1.000000000000000000, 0.8536763389692737514, 0.9699646227543736732),
 ( 1.000000000000000000, 0.8646174610552631590, 0.9722104709448051718),
 ( 1.000000000000000000, 0.8804437197805391468, 0.9754590750861457105),
 ( 1.000000000000000000, 0.8856184224478880207, 0.9765212693044487136),
 ( 1.000000000000000000, 0.8956081928670621695, 0.9785718366632991660),
 ( 1.000000000000000000, 0.9004099586942047040, 0.9795574793614618692),
 ( 1.000000000000000000, 0.9136990522410565196, 0.9822852879408843219),
 ( 1.000000000000000000, 0.9211930079257203419, 0.9838235476076078179),
 ( 1.000000000000000000, 0.9316451890867147867, 0.9859690325004727418),
 ( 1.000000000000000000, 0.9343530544005290706, 0.9865248671184547735),
 ( 1.000000000000000000, 0.9340560540550033597, 0.9864639028331361192) ) ) 
 REPRESENTATION_ITEM ( '' )  SURFACE ( )  );
#35011 = CARTESIAN_POINT ( 'NONE',  ( 86.04131037299104889, 1.712041018818101001, 4.434258418812279778 ) ) ;
#35010 = CARTESIAN_POINT ( 'NONE',  ( -59.00042985273041296, 28.09738993419675879, -6.357743741181010932 ) ) ;
#35012 = CARTESIAN_POINT ( 'NONE',  ( -54.79610818216033152, 31.51396769785350926, -1.000000000000000000 ) ) ;
#35013 = CARTESIAN_POINT ( 'NONE',  ( 0.6135038235497226600, -26.24384652275122676, 7.761113333117552138 ) ) ;
#35014 = CARTESIAN_POINT ( 'NONE',  ( 70.73355890789336797, 59.99733340013641936, 3.925556587156273647 ) ) ;
#35015 = CARTESIAN_POINT ( 'NONE',  ( 21.83619960343240152, 4.667953057257941296, -3.941150944126043054 ) ) ;
#35016 = ORIENTED_EDGE ( 'NONE', *, *, #20110, .F. ) ;
#35017 = ORIENTED_EDGE ( 'NONE', *, *, #31399, .F. ) ;
#35018 = EDGE_CURVE ( 'NONE', #35446, #1672, #3698, .T. ) ;
#35019 = CARTESIAN_POINT ( 'NONE',  ( 21.85643539959776049, -11.26069278398387929, -1.499473835228683383 ) ) ;
#35020 = CARTESIAN_POINT ( 'NONE',  ( 21.85643539959341197, 4.025506921158589435, -3.384544483166171069 ) ) ;
#35021 = ORIENTED_EDGE ( 'NONE', *, *, #14968, .T. ) ;
#35022 = CARTESIAN_POINT ( 'NONE',  ( 1.067007105073786599, -26.12771653675251571, 7.737115613922531665 ) ) ;
#35023 = CARTESIAN_POINT ( 'NONE',  ( 81.41826528540525487, 63.68099735520212334, 3.235508711566408291 ) ) ;
#35024 = CARTESIAN_POINT ( 'NONE',  ( 84.84279093542515682, 3.008464274580536113, -1.251974654204536908 ) ) ;
#35025 = ORIENTED_EDGE ( 'NONE', *, *, #31863, .F. ) ;
#35026 = CARTESIAN_POINT ( 'NONE',  ( 1.700390093233090871, -29.56993018339339940, 7.750000000000000888 ) ) ;
#35027 = CARTESIAN_POINT ( 'NONE',  ( 31.37023632097418613, -3.077502701871681623, 5.102482088558111251 ) ) ;
#35028 = CARTESIAN_POINT ( 'NONE',  ( 37.04378618670349255, -2.892922215093147287, -5.987976760426303890 ) ) ;
#35029 = CYLINDRICAL_SURFACE ( 'NONE', #14127, 4.357836081054403010 ) ;
#35030 = APPLICATION_CONTEXT ( 'automotive_design' ) ;
#35031 = DIRECTION ( 'NONE',  ( -0.000000000000000000, -0.000000000000000000, 1.000000000000000000 ) ) ;
#35032 = ADVANCED_FACE ( 'NONE', ( #27101 ), #2427, .F. ) ;
#35033 = EDGE_CURVE ( 'NONE', #30829, #25728, #11845, .T. ) ;
#35034 = CIRCLE ( 'NONE', #13282, 80.68529983683480111 ) ;
#35035 = EDGE_CURVE ( 'NONE', #5035, #35820, #16104, .T. ) ;
#35036 = CARTESIAN_POINT ( 'NONE',  ( -63.99293516169446150, 35.89893413629672381, -46.17089178453873188 ) ) ;
#35037 = CARTESIAN_POINT ( 'NONE',  ( 32.89336775635678833, -3.694078216458867914, 5.115754129267041428 ) ) ;
#35038 = EDGE_LOOP ( 'NONE', ( #36190, #19488, #26974, #16235 ) ) ;
#35039 = ORIENTED_EDGE ( 'NONE', *, *, #9680, .T. ) ;
#35040 = CARTESIAN_POINT ( 'NONE',  ( 35.21901955015318464, -1.051018187038459395, 5.414466639731517539 ) ) ;
#35041 = CARTESIAN_POINT ( 'NONE',  ( 1.584141490162101373, -33.06716345315124528, 7.761113333117551250 ) ) ;
#35042 = CARTESIAN_POINT ( 'NONE',  ( 66.70872257673579497, 57.90880667275003901, -3.999713739233791809 ) ) ;
#35043 = DIRECTION ( 'NONE',  ( 1.000000000000000000, 0.000000000000000000, 0.000000000000000000 ) ) ;
#35044 = EDGE_LOOP ( 'NONE', ( #14594, #16625, #20227, #31652, #12453 ) ) ;
#35045 = CARTESIAN_POINT ( 'NONE',  ( -75.55075356912415430, 10.07540306679061537, -8.875197024773052945 ) ) ;
#35046 = CARTESIAN_POINT ( 'NONE',  ( -70.92837670882107659, -20.78299143688747819, 38.00000000000000711 ) ) ;
#35047 = EDGE_CURVE ( 'NONE', #31670, #14437, #17820, .T. ) ;
#35048 =( NAMED_UNIT ( * ) SI_UNIT ( $, .STERADIAN. ) SOLID_ANGLE_UNIT ( ) );
#35049 = ORIENTED_EDGE ( 'NONE', *, *, #16724, .T. ) ;
#35050 = FACE_BOUND ( 'NONE', #35293, .T. ) ;
#35051 = DIRECTION ( 'NONE',  ( 1.000000000000000000, 0.000000000000000000, 0.000000000000000000 ) ) ;
#35052 = ORIENTED_EDGE ( 'NONE', *, *, #25587, .T. ) ;
#35053 = CARTESIAN_POINT ( 'NONE',  ( 23.15788130583384330, 3.915193624451748899, 3.265821563917845616 ) ) ;
#35054 = CARTESIAN_POINT ( 'NONE',  ( 79.66449323073855737, 66.32230831612966426, -1.250177805244664375 ) ) ;
#35055 = CARTESIAN_POINT ( 'NONE',  ( 80.62495340926818699, 62.95361341830508906, 3.497296750721714531 ) ) ;
#35056 = CARTESIAN_POINT ( 'NONE',  ( -1.752388709028311897, -28.99693776809384715, 7.707984471951056626 ) ) ;
#35057 = VERTEX_POINT ( 'NONE', #23797 ) ;
#35058 = CARTESIAN_POINT ( 'NONE',  ( 74.65712387123647886, 61.84722771748617731, -3.833662259905225689 ) ) ;
#35060 = CARTESIAN_POINT ( 'NONE',  ( -80.78329181448161478, 33.71485196875532608, -9.800414904976365804 ) ) ;
#35059 = CARTESIAN_POINT ( 'NONE',  ( 2.435848945842617574, -26.14806070922363901, 6.868546646838339598 ) ) ;
#35061 = CARTESIAN_POINT ( 'NONE',  ( 16.61524737713339306, 9.466292241573675881, -2.799609213114734096 ) ) ;
#35062 = CARTESIAN_POINT ( 'NONE',  ( 79.83674225097148280, 65.44563770485289922, -3.036434590848173354 ) ) ;
#35063 = CARTESIAN_POINT ( 'NONE',  ( 77.00710955723607753, 62.69977232050452898, 3.829716617887278129 ) ) ;
#35064 = EDGE_LOOP ( 'NONE', ( #36408, #27598, #27949, #14768 ) ) ;
#35065 = VECTOR ( 'NONE', #17573, 999.9999999999998863 ) ;
#35066 = EDGE_LOOP ( 'NONE', ( #3661, #20960 ) ) ;
#35067 = EDGE_CURVE ( 'NONE', #39825, #4011, #2370, .T. ) ;
#35068 = DIRECTION ( 'NONE',  ( 0.000000000000000000, 0.000000000000000000, 1.000000000000000000 ) ) ;
#35069 = CARTESIAN_POINT ( 'NONE',  ( 0.5306047266319490197, -32.86865754346513313, 7.730015791551945625 ) ) ;
#35070 = CARTESIAN_POINT ( 'NONE',  ( 81.63785901438880899, 61.64013749223438055, 1.421876342974067953 ) ) ;
#35072 = CARTESIAN_POINT ( 'NONE',  ( 17.73032609328552311, 9.401816658683801009, 2.500000000001603606 ) ) ;
#35071 = CARTESIAN_POINT ( 'NONE',  ( -0.2002656416234501746, -32.50890187101184381, 6.903112506833895878 ) ) ;
#35073 = CARTESIAN_POINT ( 'NONE',  ( 31.79760674661912745, -3.928098387035230843, -4.516596916592202859 ) ) ;
#35074 = CARTESIAN_POINT ( 'NONE',  ( -1.699430275127282286, -29.60499886526849167, 7.711434774245209844 ) ) ;
#35075 = CARTESIAN_POINT ( 'NONE',  ( -64.66796849410251014, 36.23110552202055601, 6.165526157072423352 ) ) ;
#35076 = ADVANCED_FACE ( 'NONE', ( #23998 ), #14729, .F. ) ;
#35077 = DIRECTION ( 'NONE',  ( -1.000000000000000000, 0.000000000000000000, 0.000000000000000000 ) ) ;
#35078 = DIRECTION ( 'NONE',  ( -0.000000000000000000, -0.000000000000000000, -1.000000000000000000 ) ) ;
#35079 = CARTESIAN_POINT ( 'NONE',  ( -69.92837670882107659, -20.78299143688747819, 38.00000000000000711 ) ) ;
#35080 = EDGE_CURVE ( 'NONE', #3524, #2073, #21343, .T. ) ;
#35081 = CARTESIAN_POINT ( 'NONE',  ( -88.78960668556791802, 4.298224710795182091, 15.50000000000000000 ) ) ;
#35082 = CARTESIAN_POINT ( 'NONE',  ( 37.14564460383387257, -2.766510155177709596, -6.000552212166151200 ) ) ;
#35083 = CARTESIAN_POINT ( 'NONE',  ( 72.82849231964733860, 58.84329089963347315, -3.620304665786997944 ) ) ;
#35084 = CARTESIAN_POINT ( 'NONE',  ( 1.714820913762807653, -33.06990055655550975, 7.636816916992233750 ) ) ;
#35085 = CARTESIAN_POINT ( 'NONE',  ( 3.431434570054125111, -32.49627346798381211, 7.703977250142848732 ) ) ;
#35086 = CARTESIAN_POINT ( 'NONE',  ( -80.92826776361104635, 10.51124857772332888, 4.601267702880412536 ) ) ;
#35087 = B_SPLINE_CURVE_WITH_KNOTS ( 'NONE', 3,
 ( #17756, #27043, #21278, #27448, #30963, #27647, #11375, #40202, #5018, #23940 ),
 .UNSPECIFIED., .F., .F.,
 ( 4, 3, 3, 4 ),
 ( 0.0001585009270395724165, 0.0001815657551981852242, 0.0002118214035944144299, 0.0002170292169044774099 ),
 .UNSPECIFIED. ) ;
#35088 = EDGE_CURVE ( 'NONE', #15576, #347, #27301, .T. ) ;
#35089 = CARTESIAN_POINT ( 'NONE',  ( 22.04113503551895192, -11.47825136006098568, -2.500000000000000000 ) ) ;
#35090 = CARTESIAN_POINT ( 'NONE',  ( 21.85643539959775694, -14.72209017798242847, 2.500000000000000000 ) ) ;
#35091 = VERTEX_POINT ( 'NONE', #36571 ) ;
#35092 = PLANE ( 'NONE',  #15280 ) ;
#35093 = CARTESIAN_POINT ( 'NONE',  ( 67.89958468297673733, 58.72729936788584837, -3.969942683317639887 ) ) ;
#35094 = ORIENTED_EDGE ( 'NONE', *, *, #18430, .T. ) ;
#35095 = LINE ( 'NONE', #6871, #31829 ) ;
#35096 = CARTESIAN_POINT ( 'NONE',  ( -64.08758708074093136, 36.14363715547680300, 3.800414904976363140 ) ) ;
#35097 = CARTESIAN_POINT ( 'NONE',  ( 23.54004410631070598, 2.893922283036513665, 4.010806277782499762 ) ) ;
#35098 = CARTESIAN_POINT ( 'NONE',  ( 1.226041064583952567, -26.20318123971300750, 7.759451378593095860 ) ) ;
#35099 = CARTESIAN_POINT ( 'NONE',  ( 1.700390093233090871, -29.56993018339339940, 7.750000000000000888 ) ) ;
#35100 = ORIENTED_EDGE ( 'NONE', *, *, #20916, .F. ) ;
#35101 = CARTESIAN_POINT ( 'NONE',  ( 22.87842739364366906, 4.334684949232740614, 3.062211079084044663 ) ) ;
#35102 = CARTESIAN_POINT ( 'NONE',  ( 79.28289924135637534, 65.69038102574751292, 2.688322534164183875 ) ) ;
#35103 = AXIS2_PLACEMENT_3D ( 'NONE', #3816, #10364, #9550 ) ;
#35104 = DIRECTION ( 'NONE',  ( -0.000000000000000000, -1.000000000000000000, -0.000000000000000000 ) ) ;
#35105 = ORIENTED_EDGE ( 'NONE', *, *, #38740, .T. ) ;
#35106 = CARTESIAN_POINT ( 'NONE',  ( 79.32744125533960755, 63.05206431288016944, -3.774260586041107590 ) ) ;
#35108 = CARTESIAN_POINT ( 'NONE',  ( -1.662903320652827421, -30.06828107640362902, 6.866852738645443210 ) ) ;
#35107 = CARTESIAN_POINT ( 'NONE',  ( 26.04583467364012250, 0.8117774137170248316, 4.422459632103364235 ) ) ;
#35109 = CARTESIAN_POINT ( 'NONE',  ( 81.44087877708807355, 61.54565157041660939, -1.662073781712719578 ) ) ;
#35110 = CARTESIAN_POINT ( 'NONE',  ( 78.82422632494606773, 64.37263203041347026, 3.536670452273166454 ) ) ;
#35111 = EDGE_CURVE ( 'NONE', #35525, #3023, #15662, .T. ) ;
#35112 = CARTESIAN_POINT ( 'NONE',  ( -66.57054062776667536, -31.30579396504363388, 0.000000000000000000 ) ) ;
#35113 = CARTESIAN_POINT ( 'NONE',  ( 80.70729934198679700, 66.20774049649591575, 1.233992409460102690 ) ) ;
#35114 = CARTESIAN_POINT ( 'NONE',  ( -64.08758708074093136, 42.49506848485115285, 2.672780004071997784 ) ) ;
#35115 = CARTESIAN_POINT ( 'NONE',  ( 25.50488203239457974, -4.522972804344248310, -2.044314315604920829 ) ) ;
#35116 = DIRECTION ( 'NONE',  ( 0.000000000000000000, 0.000000000000000000, -1.000000000000000000 ) ) ;
#35117 = EDGE_LOOP ( 'NONE', ( #11393, #5648, #2267, #10292 ) ) ;
#35118 = CARTESIAN_POINT ( 'NONE',  ( -75.60324101774568817, -3.659505646876107132, 10.24606351670531801 ) ) ;
#35119 = CARTESIAN_POINT ( 'NONE',  ( 22.28556454289693534, 0.2471178846263055173, -7.129343698686286146 ) ) ;
#35120 = ORIENTED_EDGE ( 'NONE', *, *, #36349, .T. ) ;
#35121 = CARTESIAN_POINT ( 'NONE',  ( 3.922988059513587089, -26.99698279172644177, 6.894806418505345924 ) ) ;
#35122 = ORIENTED_EDGE ( 'NONE', *, *, #36997, .F. ) ;
#35123 = LINE ( 'NONE', #7294, #18337 ) ;
#35124 = CARTESIAN_POINT ( 'NONE',  ( 29.62493821037406505, -3.849392467081528046, -4.318428163209237169 ) ) ;
#35125 = CARTESIAN_POINT ( 'NONE',  ( 36.87150573566773204, -2.086597623118781719, -5.863914357448089198 ) ) ;
#35126 =( BOUNDED_CURVE ( )  B_SPLINE_CURVE ( 3, ( #16043, #25523, #6593, #15227 ),
 .UNSPECIFIED., .F., .F. ) 
 B_SPLINE_CURVE_WITH_KNOTS ( ( 4, 4 ),
 ( 4.708531083176467291, 4.886921905584122428 ),
 .UNSPECIFIED. ) 
 CURVE ( )  GEOMETRIC_REPRESENTATION_ITEM ( )  RATIONAL_B_SPLINE_CURVE ( ( 1.000000000000000000, 0.9973498172709135412, 0.9973498172709135412, 1.000000000000000000 ) ) 
 REPRESENTATION_ITEM ( '' )  );
#35127 = CARTESIAN_POINT ( 'NONE',  ( 17.52987946391127139, 9.005527010368655993, 2.875160436497226524 ) ) ;
#35128 = CARTESIAN_POINT ( 'NONE',  ( 5.197761719230830302, -29.70585831616093841, 6.870724624169664452 ) ) ;
#35129 = PRODUCT_DEFINITION_SHAPE ( 'NONE', 'NONE',  #21965 ) ;
#35130 = CARTESIAN_POINT ( 'NONE',  ( -0.5767923600352592439, -26.91202874155498037, 7.695279973900954751 ) ) ;
#35131 = CARTESIAN_POINT ( 'NONE',  ( -2.878675913592191993, -26.64985754041175525, 6.700000000000000178 ) ) ;
#35132 = EDGE_CURVE ( 'NONE', #36027, #21196, #15357, .T. ) ;
#35133 = AXIS2_PLACEMENT_3D ( 'NONE', #3604, #38145, #28280 ) ;
#35134 = CARTESIAN_POINT ( 'NONE',  ( -69.08758708074093136, -65.19654454972992141, -3.800414904976364028 ) ) ;
#35135 = AXIS2_PLACEMENT_3D ( 'NONE', #1671, #19789, #35653 ) ;
#35136 = CARTESIAN_POINT ( 'NONE',  ( 22.16990573667704822, 0.5916043469538394550, -7.020939071362018780 ) ) ;
#35137 = CARTESIAN_POINT ( 'NONE',  ( 29.64522198537066089, 1.158353845804762638, -4.258353192414280564 ) ) ;
#35138 = ADVANCED_FACE ( 'NONE', ( #21554 ), #35254, .T. ) ;
#35139 = LINE ( 'NONE', #5380, #31507 ) ;
#35140 = ORIENTED_EDGE ( 'NONE', *, *, #5633, .F. ) ;
#35141 = CARTESIAN_POINT ( 'NONE',  ( 66.55417948260128469, 57.87814544581552667, 3.999688274315071013 ) ) ;
#35142 = AXIS2_PLACEMENT_3D ( 'NONE', #6212, #37485, #12579 ) ;
#35143 = CARTESIAN_POINT ( 'NONE',  ( -64.08758708074093136, 38.55592700272002560, 3.000000000000461409 ) ) ;
#35144 = CARTESIAN_POINT ( 'NONE',  ( 87.52176134051316581, -1.326109120332903846, -4.764847963194966063 ) ) ;
#35145 = VECTOR ( 'NONE', #29063, 1000.000000000000000 ) ;
#35146 = VERTEX_POINT ( 'NONE', #37582 ) ;
#35147 = CARTESIAN_POINT ( 'NONE',  ( -81.29308920802959904, 10.50256859448236746, -3.581322989614748042 ) ) ;
#35148 =( NAMED_UNIT ( * ) SI_UNIT ( $, .STERADIAN. ) SOLID_ANGLE_UNIT ( ) );
#35149 = CARTESIAN_POINT ( 'NONE',  ( 2.983339616719596243, -26.32124682031997409, 7.776484688137384360 ) ) ;
#35150 = LINE ( 'NONE', #25657, #28595 ) ;
#35151 = ORIENTED_EDGE ( 'NONE', *, *, #34538, .T. ) ;
#35152 = CARTESIAN_POINT ( 'NONE',  ( -38.24874870218063450, -26.64985754041175525, 6.700000000000000178 ) ) ;
#35153 = EDGE_LOOP ( 'NONE', ( #8150, #21251, #4399, #124, #21460 ) ) ;
#35154 = CARTESIAN_POINT ( 'NONE',  ( 80.14986013843031287, 63.43437088187636874, -3.706996517075248576 ) ) ;
#35155 = B_SPLINE_CURVE_WITH_KNOTS ( 'NONE', 3,
 ( #26552, #11081, #26160, #4725, #19770, #29040, #38486, #38892, #32938, #16469 ),
 .UNSPECIFIED., .F., .F.,
 ( 4, 3, 3, 4 ),
 ( 1.939479807224432123E-18, 3.025570593003303765E-05, 6.051145698344102830E-05, 6.468151674593725878E-05 ),
 .UNSPECIFIED. ) ;
#35156 = LINE ( 'NONE', #2268, #3659 ) ;
#35157 = CARTESIAN_POINT ( 'NONE',  ( 78.52976371562813540, 65.87711177338800894, 1.796258654642608255 ) ) ;
#35158 = ORIENTED_EDGE ( 'NONE', *, *, #28555, .T. ) ;
#35159 = DIRECTION ( 'NONE',  ( 0.000000000000000000, 0.000000000000000000, 1.000000000000000000 ) ) ;
#35160 = DIRECTION ( 'NONE',  ( 1.000000000000000000, 0.000000000000000000, 0.000000000000000000 ) ) ;
#35161 = CARTESIAN_POINT ( 'NONE',  ( -1.450854365928797352, -28.29334945402236556, 7.754798119455333705 ) ) ;
#35162 = CARTESIAN_POINT ( 'NONE',  ( 21.85643539959777826, -4.218647804531223677, -15.78683364351815221 ) ) ;
#35163 = PRODUCT_RELATED_PRODUCT_CATEGORY ( 'part', '', ( #19157 ) ) ;
#35164 = CARTESIAN_POINT ( 'NONE',  ( 21.84013737357207319, 5.905724203777740655, -3.160582246606867596 ) ) ;
#35165 = EDGE_LOOP ( 'NONE', ( #36325, #12106, #18754, #24640, #33866 ) ) ;
#35166 = CARTESIAN_POINT ( 'NONE',  ( 0.1384972100046504007, -34.01952225562621379, 7.695279973900954751 ) ) ;
#35167 = ORIENTED_EDGE ( 'NONE', *, *, #8300, .F. ) ;
#35168 = AXIS2_PLACEMENT_3D ( 'NONE', #30555, #36519, #11581 ) ;
#35169 = CARTESIAN_POINT ( 'NONE',  ( -0.9762178946850544881, -31.66653927404734858, 6.864276522220859711 ) ) ;
#35170 = CARTESIAN_POINT ( 'NONE',  ( -0.5849894831158207742, -32.20111717317018929, 7.785593909369613819 ) ) ;
#35171 = CARTESIAN_POINT ( 'NONE',  ( -73.67079394104450785, -1.142843423449616092, -9.674537367239850028 ) ) ;
#35172 = CARTESIAN_POINT ( 'NONE',  ( 4.714906974314832411, -27.79153115915092798, 7.720710062488890912 ) ) ;
#35173 = CYLINDRICAL_SURFACE ( 'NONE', #31364, 0.09010775117052761962 ) ;
#35174 = CARTESIAN_POINT ( 'NONE',  ( 80.64987221081617008, 64.05646366546658044, 3.549391953833848312 ) ) ;
#35175 = CARTESIAN_POINT ( 'NONE',  ( 85.62750488955801131, 0.9367966501063212936, -5.850367371124844063 ) ) ;
#35176 = CARTESIAN_POINT ( 'NONE',  ( -80.92837670882107659, 2.429809908903242555, 12.50000000000000000 ) ) ;
#35177 = CARTESIAN_POINT ( 'NONE',  ( -0.8876268677054017786, -31.77496589654743531, 7.652160403243383868 ) ) ;
#35178 = DIRECTION ( 'NONE',  ( -1.000000000000000000, -2.706168622523821592E-13, 0.000000000000000000 ) ) ;
#35179 = CARTESIAN_POINT ( 'NONE',  ( 33.61379031873056533, -1.222676232381281203, 5.452642950465561356 ) ) ;
#35180 = VERTEX_POINT ( 'NONE', #28534 ) ;
#35181 = EDGE_CURVE ( 'NONE', #29204, #3657, #15151, .T. ) ;
#35182 = LINE ( 'NONE', #33502, #1361 ) ;
#35183 = CARTESIAN_POINT ( 'NONE',  ( -0.3228067372202657603, -26.83740853018669625, 6.929923840112064859 ) ) ;
#35184 = EDGE_CURVE ( 'NONE', #21186, #30067, #34131, .T. ) ;
#35185 = CARTESIAN_POINT ( 'NONE',  ( -4.448748702180642667, -25.49307895267003587, 6.800000000000000711 ) ) ;
#35186 = CARTESIAN_POINT ( 'NONE',  ( 68.72765198451649837, 58.29585788764496357, 3.976359261632545827 ) ) ;
#35187 = CARTESIAN_POINT ( 'NONE',  ( 21.25451707795022571, 3.323545404380253920, 3.523679451088993275 ) ) ;
#35188 = VECTOR ( 'NONE', #13473, 1000.000000000000000 ) ;
#35189 = CARTESIAN_POINT ( 'NONE',  ( 4.246333203224189390, -31.82341053180756774, 7.778050822775633755 ) ) ;
#35190 = AXIS2_PLACEMENT_3D ( 'NONE', #2869, #34574, #17855 ) ;
#35191 = CARTESIAN_POINT ( 'NONE',  ( 88.38542499104009664, -0.9209797785659445957, 1.969977704346236536 ) ) ;
#35192 = VERTEX_POINT ( 'NONE', #37783 ) ;
#35194 = CARTESIAN_POINT ( 'NONE',  ( 0.9213240864078056092, -26.64985754041175525, 6.800000000000000711 ) ) ;
#35193 = CARTESIAN_POINT ( 'NONE',  ( 79.99568124201523744, 64.83088095446822763, -3.420541042474577242 ) ) ;
#35195 = AXIS2_PLACEMENT_3D ( 'NONE', #941, #25844, #32641 ) ;
#35196 = CARTESIAN_POINT ( 'NONE',  ( 2.910139986571841586, -32.85421171754464353, 7.635761828346577573 ) ) ;
#35197 = EDGE_LOOP ( 'NONE', ( #31598, #10153, #17062, #31290 ) ) ;
#35198 = FACE_OUTER_BOUND ( 'NONE', #39219, .T. ) ;
#35199 = AXIS2_PLACEMENT_3D ( 'NONE', #11953, #40570, #21456 ) ;
#35200 = ORIENTED_EDGE ( 'NONE', *, *, #3947, .T. ) ;
#35201 = DIRECTION ( 'NONE',  ( -0.9999026450364576490, -0.01395351027862084224, 0.000000000000000000 ) ) ;
#35202 = VERTEX_POINT ( 'NONE', #3254 ) ;
#35203 = CARTESIAN_POINT ( 'NONE',  ( 80.53350286136132752, 63.24990014040474051, -3.607546830629782875 ) ) ;
#35204 = CARTESIAN_POINT ( 'NONE',  ( -71.54229961110792146, 0.01730600142359826898, 5.969244343896260574 ) ) ;
#35205 = EDGE_CURVE ( 'NONE', #36353, #16830, #27960, .T. ) ;
#35206 = CARTESIAN_POINT ( 'NONE',  ( 22.50446240958931909, 2.315161088752189400, 5.067441199431872434 ) ) ;
#35207 = ORIENTED_EDGE ( 'NONE', *, *, #23533, .T. ) ;
#35208 = CARTESIAN_POINT ( 'NONE',  ( 4.742477098443226957, -31.30074747219525833, 7.743886751744250674 ) ) ;
#35209 = PRODUCT_DEFINITION_SHAPE ( 'NONE', 'NONE',  #40729 ) ;
#35211 = CARTESIAN_POINT ( 'NONE',  ( 3.964955798375757734, -32.23858942861218679, 7.643192810543823157 ) ) ;
#35210 = CARTESIAN_POINT ( 'NONE',  ( 4.564215312071829622, -31.40257868915064066, 6.871394612369934762 ) ) ;
#35212 = LINE ( 'NONE', #13162, #138 ) ;
#35213 = CARTESIAN_POINT ( 'NONE',  ( -64.08758708074093136, 44.07167558249655315, -1.395429732795050226 ) ) ;
#35214 = CARTESIAN_POINT ( 'NONE',  ( 69.52987064631375347, 59.66723168662304033, 3.901551322707137004 ) ) ;
#35215 = ORIENTED_EDGE ( 'NONE', *, *, #18929, .F. ) ;
#35216 = CARTESIAN_POINT ( 'NONE',  ( 23.45119107970727512, 3.196877576141845534, -3.804540727237317732 ) ) ;
#35217 = ORIENTED_EDGE ( 'NONE', *, *, #4448, .T. ) ;
#35218 = ORIENTED_EDGE ( 'NONE', *, *, #37599, .T. ) ;
#35219 = VECTOR ( 'NONE', #16464, 1000.000000000000000 ) ;
#35220 = CARTESIAN_POINT ( 'NONE',  ( 21.85643539959773207, -9.550271554086487313, -10.69920392963802769 ) ) ;
#35221 = VECTOR ( 'NONE', #7177, 1000.000000000000000 ) ;
#35222 = CARTESIAN_POINT ( 'NONE',  ( 21.86297326093952620, 3.431109414793966028, -3.921173740587788004 ) ) ;
#35223 = CARTESIAN_POINT ( 'NONE',  ( 0.3635682928745467835, -32.69609516209911959, 7.013842709614101167 ) ) ;
#35224 = CARTESIAN_POINT ( 'NONE',  ( 80.57438652550355584, 65.15318659309524207, 3.125353918848692292 ) ) ;
#35225 = CARTESIAN_POINT ( 'NONE',  ( 86.06476644049696745, 1.615394338423677079, -5.255309406831162988 ) ) ;
#35226 = ORIENTED_EDGE ( 'NONE', *, *, #19678, .F. ) ;
#35227 = LINE ( 'NONE', #6999, #14963 ) ;
#35228 = CARTESIAN_POINT ( 'NONE',  ( 16.20343186231441024, -3.286044633442916751, 2.735335442231370706 ) ) ;
#35229 = CARTESIAN_POINT ( 'NONE',  ( 35.94816592885891993, -2.120094059548885745, 5.816978721513569539 ) ) ;
#35230 = CARTESIAN_POINT ( 'NONE',  ( 5.078796878358532219, -29.18735000327637508, 6.959317978105165281 ) ) ;
#35231 = ADVANCED_FACE ( 'NONE', ( #3456 ), #34536, .F. ) ;
#35232 = CARTESIAN_POINT ( 'NONE',  ( 25.29827998133839628, 1.741210327013272607, -4.154806450938097306 ) ) ;
#35233 = FACE_OUTER_BOUND ( 'NONE', #15703, .T. ) ;
#35234 = DIRECTION ( 'NONE',  ( 1.000000000000000000, 0.000000000000000000, 0.000000000000000000 ) ) ;
#35235 = CARTESIAN_POINT ( 'NONE',  ( -16.24874870218063450, -26.64985754041175525, 6.700000000000000178 ) ) ;
#35236 = EDGE_LOOP ( 'NONE', ( #35105, #9083, #35510, #13862 ) ) ;
#35237 = CARTESIAN_POINT ( 'NONE',  ( 3.343728876470205336, -32.65988526930982516, 7.754798119455333705 ) ) ;
#35238 = CARTESIAN_POINT ( 'NONE',  ( 32.91125982496738800, -3.131047002244825794, 5.342996076127907834 ) ) ;
#35239 = EDGE_LOOP ( 'NONE', ( #39195, #6765 ) ) ;
#35240 = VERTEX_POINT ( 'NONE', #15775 ) ;
#35241 = CARTESIAN_POINT ( 'NONE',  ( 29.48676609661965387, 1.217395433518708492, 4.226912799969553269 ) ) ;
#35242 = CARTESIAN_POINT ( 'NONE',  ( 1.615255430553348415, -33.05865649385363980, 7.780491323090172884 ) ) ;
#35243 = CARTESIAN_POINT ( 'NONE',  ( 66.56005047484954673, 57.86167872611329699, -3.999845987730312746 ) ) ;
#35244 = VECTOR ( 'NONE', #17808, 1000.000000000000000 ) ;
#35245 = VERTEX_POINT ( 'NONE', #15568 ) ;
#35246 = AXIS2_PLACEMENT_3D ( 'NONE', #24951, #37487, #11546 ) ;
#35247 = CARTESIAN_POINT ( 'NONE',  ( -24.24874870218063450, -25.49307895267003587, 6.700000000000000178 ) ) ;
#35248 =( BOUNDED_SURFACE ( )  B_SPLINE_SURFACE ( 3, 2, ( 
 ( #17424, #29607, #39466 ),
 ( #24441, #12498, #6128 ),
 ( #15377, #5715, #15589 ),
 ( #37805, #37602, #3276 ) ),
 .UNSPECIFIED., .F., .F., .F. ) 
 B_SPLINE_SURFACE_WITH_KNOTS ( ( 4, 4 ),
 ( 3, 3 ),
 ( 4.712388980384689674, 4.860526820865776365 ),
 ( 0.000000000000000000, 1.000000000000000000 ),
 .UNSPECIFIED. ) 
 GEOMETRIC_REPRESENTATION_ITEM ( )  RATIONAL_B_SPLINE_SURFACE ( (
 ( 1.000000000000000000, 0.7071067811865473507, 1.000000000000000000),
 ( 1.000000000000000000, 0.7005474459265798037, 1.000000000000000000),
 ( 1.000000000000000000, 0.6938961412926945016, 1.000000000000000000),
 ( 1.000000000000000000, 0.6872206705711640939, 1.000000000000000000) ) ) 
 REPRESENTATION_ITEM ( '' )  SURFACE ( )  );
#35249 = ORIENTED_EDGE ( 'NONE', *, *, #13798, .F. ) ;
#35250 = FACE_BOUND ( 'NONE', #16521, .T. ) ;
#35251 = ADVANCED_FACE ( 'NONE', ( #19271 ), #19068, .T. ) ;
#35252 = CARTESIAN_POINT ( 'NONE',  ( -36.44874870218064444, -26.64985754041175525, 6.700000000000000178 ) ) ;
#35253 = VERTEX_POINT ( 'NONE', #31632 ) ;
#35254 = TOROIDAL_SURFACE ( 'NONE', #30628, 5.681288188914805026, 1.000000000000000000 ) ;
#35255 = CARTESIAN_POINT ( 'NONE',  ( 82.35700292606934170, 63.80179554273352238, -2.078018481493677516 ) ) ;
#35256 = CARTESIAN_POINT ( 'NONE',  ( 2.840026228868236302, -26.36660931603533697, 7.740055089680404343 ) ) ;
#35257 = EDGE_LOOP ( 'NONE', ( #34056, #33358, #26540, #40090, #34190 ) ) ;
#35258 = ORIENTED_EDGE ( 'NONE', *, *, #38842, .F. ) ;
#35259 = CARTESIAN_POINT ( 'NONE',  ( 75.12771622566773999, 62.30414178837923345, -3.756674307852014394 ) ) ;
#35261 = FACE_OUTER_BOUND ( 'NONE', #36949, .T. ) ;
#35260 = CARTESIAN_POINT ( 'NONE',  ( -8.978675913592192970, -24.55319635012989110, 6.700000000000000178 ) ) ;
#35262 = CARTESIAN_POINT ( 'NONE',  ( 15.42938493869426075, 10.99473164328989405, -2.614526699404854604 ) ) ;
#35263 = EDGE_CURVE ( 'NONE', #13934, #36582, #15970, .T. ) ;
#35264 = CARTESIAN_POINT ( 'NONE',  ( 77.39092423430432177, 61.90746491491122327, 3.829716617890443153 ) ) ;
#35265 = B_SPLINE_CURVE_WITH_KNOTS ( 'NONE', 3,
 ( #7573, #26719, #38656, #7966, #23622, #29601, #36186, #1416 ),
 .UNSPECIFIED., .F., .F.,
 ( 4, 2, 2, 4 ),
 ( 0.001627818838919652990, 0.002602893308734022942, 0.003577967778548392895, 0.005528116718177132800 ),
 .UNSPECIFIED. ) ;
#35266 = CARTESIAN_POINT ( 'NONE',  ( 4.425294480038274081, -27.53648579448824307, 6.903372536218453703 ) ) ;
#35267 = EDGE_CURVE ( 'NONE', #26162, #25891, #27709, .T. ) ;
#35268 = EDGE_CURVE ( 'NONE', #22017, #23856, #37993, .T. ) ;
#35269 = CARTESIAN_POINT ( 'NONE',  ( -31.07867591359219617, -24.55319635012989110, 6.700000000000000178 ) ) ;
#35270 = FACE_OUTER_BOUND ( 'NONE', #32785, .T. ) ;
#35271 = CARTESIAN_POINT ( 'NONE',  ( 81.39647959751771111, 65.22731470771827844, 2.622983904469076588 ) ) ;
#35272 = CARTESIAN_POINT ( 'NONE',  ( 86.92636418897033934, 0.7179065655219835085, -4.964803926638174048 ) ) ;
#35273 = CARTESIAN_POINT ( 'NONE',  ( 31.06145916124171436, -2.509195271462365540, -5.777646538787225339 ) ) ;
#35274 = CARTESIAN_POINT ( 'NONE',  ( 0.5248424762351729944, -26.37961863118246697, 7.635761828346577573 ) ) ;
#35275 = CARTESIAN_POINT ( 'NONE',  ( 21.85643539959777115, -13.25467889390307796, 0.8368004220631568568 ) ) ;
#35276 = CARTESIAN_POINT ( 'NONE',  ( 5.200390093233090205, -29.56993018339339940, 6.850000000000000533 ) ) ;
#35277 = DIRECTION ( 'NONE',  ( -0.000000000000000000, -0.000000000000000000, 1.000000000000000000 ) ) ;
#35278 = AXIS2_PLACEMENT_3D ( 'NONE', #4153, #32759, #26770 ) ;
#35279 = CARTESIAN_POINT ( 'NONE',  ( -1.543298022821887328, -28.25521066738867049, 7.750000000000000888 ) ) ;
#35280 = ADVANCED_FACE ( 'NONE', ( #31028 ), #40676, .F. ) ;
#35281 = CARTESIAN_POINT ( 'NONE',  ( 34.12188614642886364, -3.607431673937933958, -5.453371772074238955 ) ) ;
#35282 = LINE ( 'NONE', #7049, #28585 ) ;
#35283 = CARTESIAN_POINT ( 'NONE',  ( -73.79226524390077202, -1.360417495813321054, 15.50000000000000000 ) ) ;
#35284 = CARTESIAN_POINT ( 'NONE',  ( 3.382565993577793861, -32.52465162557860623, 7.779495906702013741 ) ) ;
#35285 = CARTESIAN_POINT ( 'NONE',  ( -70.92837670882107659, 10.37661300689600097, 0.000000000000000000 ) ) ;
#35286 = CIRCLE ( 'NONE', #31989, 0.1000000000000028644 ) ;
#35287 = PLANE ( 'NONE',  #1794 ) ;
#35288 = CARTESIAN_POINT ( 'NONE',  ( 21.88090590480122444, -13.32625148503419865, 2.500000000000000444 ) ) ;
#35289 = VERTEX_POINT ( 'NONE', #40457 ) ;
#35290 = CARTESIAN_POINT ( 'NONE',  ( -28.24874870218063805, -26.64985754041175525, 6.700000000000000178 ) ) ;
#35291 = CARTESIAN_POINT ( 'NONE',  ( 67.98336428835678191, 58.50351186300884621, -3.992939643064463695 ) ) ;
#35292 = ADVANCED_FACE ( 'NONE', ( #31227 ), #12267, .F. ) ;
#35293 = EDGE_LOOP ( 'NONE', ( #12833, #35685, #14535, #22729 ) ) ;
#35294 = DIRECTION ( 'NONE',  ( -0.000000000000000000, -0.000000000000000000, -1.000000000000000000 ) ) ;
#35295 = CARTESIAN_POINT ( 'NONE',  ( -69.92837670882107659, 28.72470171467712063, 5.916079783099620570 ) ) ;
#35296 = CARTESIAN_POINT ( 'NONE',  ( 22.21409233198261290, 3.844288165656574829, 4.110153234016473256 ) ) ;
#35297 = CARTESIAN_POINT ( 'NONE',  ( 5.048061004931336804, -28.54860354809848033, 6.989977667959443863 ) ) ;
#35298 = CARTESIAN_POINT ( 'NONE',  ( 1.075872451927647244, -26.22777759477400039, 7.712764235869105534 ) ) ;
#35299 = CARTESIAN_POINT ( 'NONE',  ( 1.175744690447600105, -26.10947541539887240, 6.865554069792297653 ) ) ;
#35300 = EDGE_LOOP ( 'NONE', ( #15832, #21889, #27462, #31689 ) ) ;
#35301 = CARTESIAN_POINT ( 'NONE',  ( 23.14157197170704805, 4.048751080929327451, 3.076040433570303989 ) ) ;
#35302 = CARTESIAN_POINT ( 'NONE',  ( -81.90888476619602443, -6.597313057213483489, -0.6545554231109771415 ) ) ;
#35303 = CARTESIAN_POINT ( 'NONE',  ( 19.12733620826224978, -3.077968911084931758, 3.134593501090364054 ) ) ;
#35304 = CARTESIAN_POINT ( 'NONE',  ( 81.21900516562017458, 61.35514353465740101, 1.483717294825997790 ) ) ;
#35305 = B_SPLINE_CURVE_WITH_KNOTS ( 'NONE', 3,
 ( #9574, #21945, #3441, #6506, #15957, #12869, #31413, #28519, #37977, #12052, #27714, #37183, #14951, #8973, #21559, #34135, #40070, #25193, #37723, #11998, #18588, #31375, #5853, #34285, #8712, #15102, #15513, #28271, #28069, #6466, #40622 ),
 .UNSPECIFIED., .F., .F.,
 ( 4, 3, 3, 3, 3, 3, 3, 3, 3, 3, 4 ),
 ( 1.748223473168675632E-18, 2.999644130997695371E-05, 6.002588995694948609E-05, 8.960886084588150333E-05, 0.0001190604700446518306, 0.0001489538463052718831, 0.0001796139255494018936, 0.0002109707048517080001, 0.0002426195318110375249, 0.0002740640997890114424, 0.0002849778069099955869 ),
 .UNSPECIFIED. ) ;
#35306 = CARTESIAN_POINT ( 'NONE',  ( 81.16957891225059996, 61.30398062001309256, 1.000000000000000000 ) ) ;
#35307 = ORIENTED_EDGE ( 'NONE', *, *, #37080, .T. ) ;
#35308 = CARTESIAN_POINT ( 'NONE',  ( 77.90798433017856439, 65.01733068894688472, -2.764360460937554720 ) ) ;
#35310 = CARTESIAN_POINT ( 'NONE',  ( -1.719074876076428948, -28.82337947204507245, 6.873192711770539809 ) ) ;
#35309 = CARTESIAN_POINT ( 'NONE',  ( 25.40142685431079528, 0.6874522221836151248, 4.599600658783209006 ) ) ;
#35311 = MECHANICAL_DESIGN_GEOMETRIC_PRESENTATION_REPRESENTATION (  '', ( #35967 ), #32015 ) ;
#35312 = EDGE_CURVE ( 'NONE', #36632, #14653, #40464, .T. ) ;
#35313 = CARTESIAN_POINT ( 'NONE',  ( 81.69769846483475817, 62.77423530097588156, -2.811330881955112382 ) ) ;
#35314 = CARTESIAN_POINT ( 'NONE',  ( 79.95886636011078963, 62.14075979114826254, 3.401284978681017090 ) ) ;
#35315 = AXIS2_PLACEMENT_3D ( 'NONE', #20097, #19706, #7341 ) ;
#35316 = ADVANCED_FACE ( 'NONE', ( #3047 ), #22973, .T. ) ;
#35317 = PRODUCT_DEFINITION ( 'UNKNOWN', '', #32740, #2437 ) ;
#35318 = DIRECTION ( 'NONE',  ( -0.000000000000000000, -0.000000000000000000, -1.000000000000000000 ) ) ;
#35319 = CARTESIAN_POINT ( 'NONE',  ( 79.68852728668518637, 66.33522678087791746, 1.065376284871803803 ) ) ;
#35320 = DIRECTION ( 'NONE',  ( -0.000000000000000000, -0.000000000000000000, -1.000000000000000000 ) ) ;
#35321 = CARTESIAN_POINT ( 'NONE',  ( 24.54460225945253526, -1.054324096271329614, -6.891227800717186547 ) ) ;
#35322 = B_SPLINE_CURVE_WITH_KNOTS ( 'NONE', 3,
 ( #177, #38228, #9832, #22408, #3891, #22210, #587, #10025, #989, #12713 ),
 .UNSPECIFIED., .F., .F.,
 ( 4, 3, 3, 4 ),
 ( 0.0001585009270395791115, 0.0001815657551981845195, 0.0002118214035944147281, 0.0002170292169044849180 ),
 .UNSPECIFIED. ) ;
#35323 = CARTESIAN_POINT ( 'NONE',  ( -64.42495406928412649, 36.58927325464082259, -5.700117363499904499 ) ) ;
#35324 = ORIENTED_EDGE ( 'NONE', *, *, #31070, .F. ) ;
#35325 = CARTESIAN_POINT ( 'NONE',  ( -75.48799235854204426, -5.171441145269375816, 8.906435695295353838 ) ) ;
#35326 = CARTESIAN_POINT ( 'NONE',  ( 25.40611314139961507, 0.6577627199992637230, -4.600311117202987354 ) ) ;
#35327 = CARTESIAN_POINT ( 'NONE',  ( -0.04364293620010380181, -32.60287272531510894, 7.762796336881260473 ) ) ;
#35328 = EDGE_LOOP ( 'NONE', ( #2226, #24007, #8406, #13855 ) ) ;
#35329 = CARTESIAN_POINT ( 'NONE',  ( -1.026852816783328626, -31.74722329408204757, 7.780491323090176436 ) ) ;
#35330 = CARTESIAN_POINT ( 'NONE',  ( 34.14206359931419854, -3.846217481392709914, -5.236744094428941843 ) ) ;
#35331 = DIRECTION ( 'NONE',  ( -0.3420201433256726542, 0.9396926207859070956, -0.000000000000000000 ) ) ;
#35332 = CYLINDRICAL_SURFACE ( 'NONE', #32141, 3.399999999999999911 ) ;
#35333 = CARTESIAN_POINT ( 'NONE',  ( 19.31057600782361305, 7.430049097904062094, 3.124219774106051783 ) ) ;
#35334 = CARTESIAN_POINT ( 'NONE',  ( 5.198825856949740754, -29.67505948803950488, 6.863784140767622333 ) ) ;
#35335 = LINE ( 'NONE', #20065, #30591 ) ;
#35336 = DIRECTION ( 'NONE',  ( 1.000000000000000000, 0.000000000000000000, 0.000000000000000000 ) ) ;
#35337 = AXIS2_PLACEMENT_3D ( 'NONE', #33902, #30810, #31411 ) ;
#35338 = LINE ( 'NONE', #7108, #739 ) ;
#35339 = CARTESIAN_POINT ( 'NONE',  ( 24.65336533415635856, 1.592875596455870513, -4.500810045853856245 ) ) ;
#35340 = CARTESIAN_POINT ( 'NONE',  ( 36.36861739423189022, -1.688192717328701686, -5.711810702524172889 ) ) ;
#35341 = CARTESIAN_POINT ( 'NONE',  ( -4.444218661349752963, -35.94265729135299381, 6.000000000000000000 ) ) ;
#35342 = EDGE_LOOP ( 'NONE', ( #31787, #18562, #27408, #19324 ) ) ;
#35343 = CARTESIAN_POINT ( 'NONE',  ( 66.68223030933245354, 57.98259542220473861, 3.998057522776775841 ) ) ;
#35344 = VECTOR ( 'NONE', #22803, 1000.000000000000000 ) ;
#35345 = CARTESIAN_POINT ( 'NONE',  ( 87.94553049950697243, -1.849565313017166535, -3.579236442506480653 ) ) ;
#35346 = ORIENTED_EDGE ( 'NONE', *, *, #29461, .F. ) ;
#35347 = CARTESIAN_POINT ( 'NONE',  ( 26.59686585277882998, 1.637759102572657888, 4.330020466781864918 ) ) ;
#35348 = EDGE_CURVE ( 'NONE', #4130, #20764, #1815, .T. ) ;
#35349 = CARTESIAN_POINT ( 'NONE',  ( 2.881058359821971226, -26.27508231979332010, 7.750000000000000000 ) ) ;
#35350 = CARTESIAN_POINT ( 'NONE',  ( -70.92837670882107659, -23.80776546975053520, 10.00000000000000533 ) ) ;
#35351 = ORIENTED_EDGE ( 'NONE', *, *, #5456, .T. ) ;
#35352 =( NAMED_UNIT ( * ) SI_UNIT ( $, .STERADIAN. ) SOLID_ANGLE_UNIT ( ) );
#35353 = EDGE_CURVE ( 'NONE', #20794, #8875, #3802, .T. ) ;
#35354 = ORIENTED_EDGE ( 'NONE', *, *, #1267, .F. ) ;
#35355 = CARTESIAN_POINT ( 'NONE',  ( 78.73521632358543343, 65.70333808056810199, -2.340042473998858785 ) ) ;
#35356 = B_SPLINE_CURVE_WITH_KNOTS ( 'NONE', 3,
 ( #10031, #1203, #28986, #789, #593, #38234, #26500, #29185, #22613, #35183, #10827, #13318, #32095, #3899, #38430, #22815, #7155, #19716, #32291, #4089, #13532, #26106, #38638, #10436, #39859, #5273, #27095, #30611, #11428, #17814, #24416 ),
 .UNSPECIFIED., .F., .F.,
 ( 4, 3, 3, 3, 3, 3, 3, 3, 3, 3, 4 ),
 ( 1.084202172485504434E-19, 2.999644130997704858E-05, 6.002588995694863906E-05, 8.960886084588055465E-05, 0.0001190604700446490523, 0.0001489538463052745123, 0.0001796139255493987494, 0.0002109707048517110088, 0.0002426195318110379857, 0.0002740640997890076477, 0.0002849778069099910332 ),
 .UNSPECIFIED. ) ;
#35357 = CARTESIAN_POINT ( 'NONE',  ( 80.96289755590217396, 61.39497013797971192, 2.048264032867408879 ) ) ;
#35358 = CARTESIAN_POINT ( 'NONE',  ( -1.299626552915077449, -31.16989897147455935, 6.864276522220859711 ) ) ;
#35359 = EDGE_CURVE ( 'NONE', #24953, #27554, #38391, .T. ) ;
#35360 = AXIS2_PLACEMENT_3D ( 'NONE', #28361, #25080, #6345 ) ;
#35362 = ADVANCED_FACE ( 'NONE', ( #10193 ), #953, .F. ) ;
#35361 = CARTESIAN_POINT ( 'NONE',  ( 24.75277909289565770, 2.391494161259001938, 4.069667844307693905 ) ) ;
#35363 = CARTESIAN_POINT ( 'NONE',  ( 0.9954086067726409803, -32.99821069240157101, 6.863654226668488789 ) ) ;
#35364 = CARTESIAN_POINT ( 'NONE',  ( -1.784401156299032509, -29.50863702383910336, 7.785387725071482024 ) ) ;
#35365 = PRODUCT_DEFINITION_FORMATION_WITH_SPECIFIED_SOURCE ( 'ANY', '', #4229, .NOT_KNOWN. ) ;
#35366 = CARTESIAN_POINT ( 'NONE',  ( 21.85643539959781023, -13.06032977194142930, 9.178732910485948082 ) ) ;
#35367 = AXIS2_PLACEMENT_3D ( 'NONE', #8697, #15495, #30962 ) ;
#35368 = CARTESIAN_POINT ( 'NONE',  ( 22.19214921742566204, 5.242882102261849475, -3.093814343854897064 ) ) ;
#35369 = VERTEX_POINT ( 'NONE', #19474 ) ;
#35370 = CARTESIAN_POINT ( 'NONE',  ( 5.200323364668523851, -29.54781842220009480, 7.743886751744250674 ) ) ;
#35371 = VECTOR ( 'NONE', #23715, 1000.000000000000000 ) ;
#35372 = ORIENTED_EDGE ( 'NONE', *, *, #19889, .F. ) ;
#35373 = CARTESIAN_POINT ( 'NONE',  ( -1.030507639981847356, -31.59532027377766283, 6.920489980334481039 ) ) ;
#35374 = DIRECTION ( 'NONE',  ( 1.000000000000000000, 0.000000000000000000, 0.000000000000000000 ) ) ;
#35375 = CARTESIAN_POINT ( 'NONE',  ( -72.84127017857981912, 2.226350102246259954, -9.875462825488979135 ) ) ;
#35376 = DIRECTION ( 'NONE',  ( -0.000000000000000000, -0.000000000000000000, -1.000000000000000000 ) ) ;
#35377 = CARTESIAN_POINT ( 'NONE',  ( -31.07867591359219617, -24.55319635012989110, 6.800000000000000711 ) ) ;
#35378 = CARTESIAN_POINT ( 'NONE',  ( 81.14353007428552189, 63.18723978346950076, 3.330128783915581092 ) ) ;
#35379 = CARTESIAN_POINT ( 'NONE',  ( 84.69769694898896262, 2.275084749292730635, 4.163914512140848068 ) ) ;
#35380 = DIRECTION ( 'NONE',  ( 0.000000000000000000, 0.000000000000000000, 1.000000000000000000 ) ) ;
#35381 = FACE_BOUND ( 'NONE', #9357, .T. ) ;
#35382 = CARTESIAN_POINT ( 'NONE',  ( -1.641543316846993505, -30.19561467464317772, 7.691066658568947112 ) ) ;
#35383 = ORIENTED_EDGE ( 'NONE', *, *, #12129, .T. ) ;
#35384 = CARTESIAN_POINT ( 'NONE',  ( 1.740389608043702241, -26.17015157826628524, 7.784838882742139532 ) ) ;
#35385 = DIRECTION ( 'NONE',  ( -0.000000000000000000, -0.000000000000000000, 1.000000000000000000 ) ) ;
#35386 = CARTESIAN_POINT ( 'NONE',  ( -1.002985311074516162, -27.34692170059995675, 7.678495282201408756 ) ) ;
#35387 = AXIS2_PLACEMENT_3D ( 'NONE', #27082, #39627, #4849 ) ;
#35388 = CARTESIAN_POINT ( 'NONE',  ( 69.25747553239096987, 58.65839085985714974, 3.984982412582168010 ) ) ;
#35389 = CARTESIAN_POINT ( 'NONE',  ( 36.19429332948913469, -2.231517989824187254, 5.855392854995553620 ) ) ;
#35390 = AXIS2_PLACEMENT_3D ( 'NONE', #37607, #34361, #22400 ) ;
#35391 = CARTESIAN_POINT ( 'NONE',  ( -64.08758708074094557, 43.44355869293354999, -1.729337825382090132 ) ) ;
#35392 = CARTESIAN_POINT ( 'NONE',  ( 86.46420362610733434, 1.237027245193318192, -5.068583899740296772 ) ) ;
#35393 = ORIENTED_EDGE ( 'NONE', *, *, #38575, .T. ) ;
#35395 = CARTESIAN_POINT ( 'NONE',  ( -0.4289785860461575728, -26.79218406234506844, 6.880828092187094569 ) ) ;
#35394 = CARTESIAN_POINT ( 'NONE',  ( 79.02829278184947270, 65.95432764922180979, -2.098997056523009164 ) ) ;
#35396 = CARTESIAN_POINT ( 'NONE',  ( 4.358291535071521672, -27.29274773012506827, 7.695279973900954751 ) ) ;
#35397 = VECTOR ( 'NONE', #21023, 1000.000000000000114 ) ;
#35398 = ORIENTED_EDGE ( 'NONE', *, *, #28785, .T. ) ;
#35399 = CARTESIAN_POINT ( 'NONE',  ( -8.448748702180639114, -26.64985754041175525, 6.800000000000000711 ) ) ;
#35400 = ORIENTED_EDGE ( 'NONE', *, *, #1283, .T. ) ;
#35401 = CARTESIAN_POINT ( 'NONE',  ( -78.87124948352045806, -6.567092532003710126, 6.089658418205694090 ) ) ;
#35402 = ORIENTED_EDGE ( 'NONE', *, *, #15044, .T. ) ;
#35403 = CARTESIAN_POINT ( 'NONE',  ( 79.23506694815775120, 65.34107492257662386, -3.003915454719717992 ) ) ;
#35404 = PLANE ( 'NONE',  #33918 ) ;
#35405 = CARTESIAN_POINT ( 'NONE',  ( 25.84952034417671740, 2.048349254327011426, 4.178021515479660941 ) ) ;
#35407 = ORIENTED_EDGE ( 'NONE', *, *, #30798, .T. ) ;
#35406 = EDGE_LOOP ( 'NONE', ( #166, #11697, #5946, #37925 ) ) ;
#35408 = EDGE_CURVE ( 'NONE', #36238, #36741, #10323, .T. ) ;
#35409 = EDGE_CURVE ( 'NONE', #40638, #24427, #21094, .T. ) ;
#35411 = EDGE_CURVE ( 'NONE', #4455, #40540, #33755, .T. ) ;
#35410 = CARTESIAN_POINT ( 'NONE',  ( 0.03050408833857739394, -32.53159980382280736, 7.712764235869104645 ) ) ;
#35412 = AXIS2_PLACEMENT_3D ( 'NONE', #24601, #27682, #5878 ) ;
#35414 = CARTESIAN_POINT ( 'NONE',  ( 85.75260874296688485, 2.036324392267200079, 3.804357317183401754 ) ) ;
#35413 = CARTESIAN_POINT ( 'NONE',  ( 4.536150672677811357, -31.44568654712173128, 6.929923840112063971 ) ) ;
#35415 = DIRECTION ( 'NONE',  ( 0.2567910337120269948, 0.7055275666422181624, 0.6605219282605379050 ) ) ;
#35416 = DIRECTION ( 'NONE',  ( 0.000000000000000000, 0.000000000000000000, 1.000000000000000000 ) ) ;
#35417 = CARTESIAN_POINT ( 'NONE',  ( 69.80049859759003539, 58.98221833774336176, 3.985452289341161691 ) ) ;
#35418 = CARTESIAN_POINT ( 'NONE',  ( 22.37633911595722935, 4.133713974500000887, -3.770963387559532087 ) ) ;
#35419 = ORIENTED_EDGE ( 'NONE', *, *, #5584, .T. ) ;
#35420 = DIRECTION ( 'NONE',  ( -0.000000000000000000, -0.000000000000000000, -1.000000000000000000 ) ) ;
#35421 = ORIENTED_EDGE ( 'NONE', *, *, #9157, .F. ) ;
#35422 = CARTESIAN_POINT ( 'NONE',  ( 21.85643539959779957, -12.42149291456256499, -5.642648835571736576 ) ) ;
#35423 = CARTESIAN_POINT ( 'NONE',  ( 21.86624219161038241, 3.264102293340214622, 3.922476187580718587 ) ) ;
#35424 = LINE ( 'NONE', #20341, #26121 ) ;
#35425 = CARTESIAN_POINT ( 'NONE',  ( 81.32842084066379584, 61.39880091617793312, 1.358900964592128391 ) ) ;
#35426 = CARTESIAN_POINT ( 'NONE',  ( 84.79389884800966115, 3.063713526918731223, 0.3112276665278714827 ) ) ;
#35427 = ORIENTED_EDGE ( 'NONE', *, *, #12021, .T. ) ;
#35428 = CIRCLE ( 'NONE', #11040, 80.68529983683480111 ) ;
#35429 = DIRECTION ( 'NONE',  ( 0.000000000000000000, -0.6662082868431825622, 0.7457657263118704360 ) ) ;
#35430 = CARTESIAN_POINT ( 'NONE',  ( 5.073402035585432124, -29.14231025274367326, 6.876076431790004939 ) ) ;
#35431 = CARTESIAN_POINT ( 'NONE',  ( 36.79795713293712112, -2.555754650487687130, -5.949609191187919421 ) ) ;
#35432 = DIRECTION ( 'NONE',  ( -0.000000000000000000, -0.000000000000000000, 1.000000000000000000 ) ) ;
#35433 = LINE ( 'NONE', #29439, #20666 ) ;
#35434 = CARTESIAN_POINT ( 'NONE',  ( 4.404045757636788849, -31.79259668886174595, 7.710604733652627552 ) ) ;
#35435 = CARTESIAN_POINT ( 'NONE',  ( 3.863272490615877519, -26.94658504119581011, 7.661510568013093270 ) ) ;
#35436 = CARTESIAN_POINT ( 'NONE',  ( -63.08379346057677139, 18.80112958435941906, -46.17089178453873188 ) ) ;
#35437 = CARTESIAN_POINT ( 'NONE',  ( 29.60505900326302609, -3.794812366572309692, 4.412074707466141277 ) ) ;
#35438 = AXIS2_PLACEMENT_3D ( 'NONE', #40609, #24777, #37322 ) ;
#35439 = VERTEX_POINT ( 'NONE', #2983 ) ;
#35440 = ORIENTED_EDGE ( 'NONE', *, *, #8566, .T. ) ;
#35441 = CARTESIAN_POINT ( 'NONE',  ( 37.00831260221009700, -3.245544418880986548, 5.947168679556439130 ) ) ;
#35442 = CARTESIAN_POINT ( 'NONE',  ( 1.578585683582428345, -33.06757917596850405, 7.754798119455333705 ) ) ;
#35443 = CARTESIAN_POINT ( 'NONE',  ( -70.92837670882107659, -23.80776546975053165, -6.000000000000005329 ) ) ;
#35444 = CARTESIAN_POINT ( 'NONE',  ( 87.90201547669775550, -2.482640368694746691, -0.9994344668162112866 ) ) ;
#35445 = VERTEX_POINT ( 'NONE', #8750 ) ;
#35446 = VERTEX_POINT ( 'NONE', #3477 ) ;
#35447 = CARTESIAN_POINT ( 'NONE',  ( -16.87867591359218977, -24.55319635012989110, 6.800000000000000711 ) ) ;
#35448 = CARTESIAN_POINT ( 'NONE',  ( 0.000000000000000000, 0.000000000000000000, 0.000000000000000000 ) ) ;
#35449 = VERTEX_POINT ( 'NONE', #10220 ) ;
#35450 = CARTESIAN_POINT ( 'NONE',  ( -55.72565997008025818, 31.19966888624891865, -3.920894724096664508 ) ) ;
#35451 = CARTESIAN_POINT ( 'NONE',  ( 3.799299724975022219, -32.37074764920551218, 6.961115707816239784 ) ) ;
#35452 = ORIENTED_EDGE ( 'NONE', *, *, #23889, .T. ) ;
#35453 = CARTESIAN_POINT ( 'NONE',  ( 23.71906029381402092, 3.521941673742745582, 3.287647665226494098 ) ) ;
#35454 = CARTESIAN_POINT ( 'NONE',  ( 81.71086237227936522, 61.67650090218637615, -1.250621450094242304 ) ) ;
#35456 = EDGE_CURVE ( 'NONE', #17660, #33469, #11115, .T. ) ;
#35455 = CARTESIAN_POINT ( 'NONE',  ( -1.316098561281709767, -31.34497840729704521, 7.730015791551948290 ) ) ;
#35457 = VERTEX_POINT ( 'NONE', #32277 ) ;
#35458 = CARTESIAN_POINT ( 'NONE',  ( 75.94307401167466764, 60.53934701228696014, -3.685888554891455282 ) ) ;
#35460 = CYLINDRICAL_SURFACE ( 'NONE', #7809, 6.000000000000005329 ) ;
#35459 = CARTESIAN_POINT ( 'NONE',  ( 2.385094845610274295, -26.13755791307188048, 6.866770815808350470 ) ) ;
#35461 = DIRECTION ( 'NONE',  ( -0.000000000000000000, -0.000000000000000000, 1.000000000000000000 ) ) ;
#35462 = CARTESIAN_POINT ( 'NONE',  ( 76.45598340902213863, 62.40619074383512555, 3.848392762312490945 ) ) ;
#35463 = FACE_OUTER_BOUND ( 'NONE', #625, .T. ) ;
#35464 = DIRECTION ( 'NONE',  ( 0.000000000000000000, 1.000000000000000000, 0.000000000000000000 ) ) ;
#35465 = CIRCLE ( 'NONE', #22970, 3.499999999999999556 ) ;
#35466 = CARTESIAN_POINT ( 'NONE',  ( 23.14565985387361025, 3.365906385940814260, -3.818838018732628292 ) ) ;
#35467 = FACE_OUTER_BOUND ( 'NONE', #38290, .T. ) ;
#35468 = CARTESIAN_POINT ( 'NONE',  ( 79.18750747900355691, 66.22443723336836285, 1.498428902123875694 ) ) ;
#35469 = CARTESIAN_POINT ( 'NONE',  ( -0.1485713413135285321, -32.54168751089497391, 6.865482280155369210 ) ) ;
#35470 = CARTESIAN_POINT ( 'NONE',  ( 29.80812890880734756, -3.278499718192964263, -4.781105184254491824 ) ) ;
#35471 = CARTESIAN_POINT ( 'NONE',  ( -1.699558106226426890, -29.58869826779166701, 7.748216051605116839 ) ) ;
#35472 = FACE_OUTER_BOUND ( 'NONE', #25509, .T. ) ;
#35473 = ORIENTED_EDGE ( 'NONE', *, *, #19034, .T. ) ;
#35474 = FACE_OUTER_BOUND ( 'NONE', #8329, .T. ) ;
#35475 = CARTESIAN_POINT ( 'NONE',  ( 66.60662334906898252, 57.77574420286332213, 3.999150726296102132 ) ) ;
#35476 = CARTESIAN_POINT ( 'NONE',  ( 35.79586196015494437, -3.408963864873948424, -5.784727818347247918 ) ) ;
#35477 = CARTESIAN_POINT ( 'NONE',  ( 1.141703107443977849, -32.92371444179612183, 7.721096864323902409 ) ) ;
#35478 = CARTESIAN_POINT ( 'NONE',  ( -39.07867591359219261, -26.64985754041175525, 6.700000000000000178 ) ) ;
#35479 = CYLINDRICAL_SURFACE ( 'NONE', #16751, 0.09010775117052885475 ) ;
#35480 = B_SPLINE_CURVE_WITH_KNOTS ( 'NONE', 3,
 ( #37704, #6236, #31154, #5621, #18567, #2760, #15286, #24554, #36910, #12194, #18780, #37510, #15697, #33843, #8691, #14868, #18161, #30956, #15079, #3183, #34669, #30755, #6447, #22094, #2970, #27838, #28249, #11976, #31357, #40392, #19000 ),
 .UNSPECIFIED., .F., .F.,
 ( 4, 3, 3, 3, 3, 3, 3, 3, 3, 3, 4 ),
 ( 0.000000000000000000, 2.999644130997664200E-05, 6.002588995694806986E-05, 8.960886084588066307E-05, 0.0001190604700446488490, 0.0001489538463052730486, 0.0001796139255493973128, 0.0002109707048517051541, 0.0002426195318110360071, 0.0002740640997890082440, 0.0002849778069099824680 ),
 .UNSPECIFIED. ) ;
#35481 = DIRECTION ( 'NONE',  ( -1.000000000000000000, -1.165409145176969993E-16, 0.000000000000000000 ) ) ;
#35482 = EDGE_CURVE ( 'NONE', #24284, #21608, #22204, .T. ) ;
#35483 = CARTESIAN_POINT ( 'NONE',  ( 22.81512952464498056, -8.568292043100733224, -2.500000000000000000 ) ) ;
#35484 = CARTESIAN_POINT ( 'NONE',  ( -0.4696069411706714214, -32.18740172037517766, 7.643333865083952183 ) ) ;
#35485 = VERTEX_POINT ( 'NONE', #580 ) ;
#35486 = CARTESIAN_POINT ( 'NONE',  ( 32.98352007369545902, -0.3890908133127232160, 5.239426168307027787 ) ) ;
#35487 = DIRECTION ( 'NONE',  ( 0.000000000000000000, 1.000000000000000000, 0.000000000000000000 ) ) ;
#35488 = CARTESIAN_POINT ( 'NONE',  ( 67.53434038244741089, 57.92037869207645429, -3.987264345885670913 ) ) ;
#35489 = CARTESIAN_POINT ( 'NONE',  ( 4.713340623123058570, -27.78888299018493058, 7.686927408461905920 ) ) ;
#35490 = EDGE_CURVE ( 'NONE', #8717, #13364, #375, .T. ) ;
#35491 = VERTEX_POINT ( 'NONE', #38626 ) ;
#35492 = DIRECTION ( 'NONE',  ( -0.000000000000000000, -0.000000000000000000, 1.000000000000000000 ) ) ;
#35493 = AXIS2_PLACEMENT_3D ( 'NONE', #12191, #25168, #22302 ) ;
#35494 = CARTESIAN_POINT ( 'NONE',  ( 30.87471915742276707, -3.492139151130889463, 4.893529281628630656 ) ) ;
#35495 = CARTESIAN_POINT ( 'NONE',  ( 22.82768571636377075, 3.344825573009538644, 4.025161535770593879 ) ) ;
#35496 = LINE ( 'NONE', #706, #12979 ) ;
#35497 = CARTESIAN_POINT ( 'NONE',  ( 4.241058378038022880, -25.24127732835732374, 7.695279973900954751 ) ) ;
#35498 = CARTESIAN_POINT ( 'NONE',  ( 4.402303332471854347, -31.79471440835236606, 7.670465701733749420 ) ) ;
#35499 = ORIENTED_EDGE ( 'NONE', *, *, #17053, .F. ) ;
#35500 = CARTESIAN_POINT ( 'NONE',  ( 4.944606980600187107, -30.88334510993980686, 7.751599049952199394 ) ) ;
#35501 = CARTESIAN_POINT ( 'NONE',  ( 78.99338515863716736, 65.92867347524024524, 2.125034277891690415 ) ) ;
#35503 = ADVANCED_FACE ( 'NONE', ( #10425 ), #13119, .T. ) ;
#35502 = CARTESIAN_POINT ( 'NONE',  ( -63.67242066106361165, 44.20199017310434897, 2.029227019513839103 ) ) ;
#35504 = VERTEX_POINT ( 'NONE', #25677 ) ;
#35505 = CARTESIAN_POINT ( 'NONE',  ( 77.70122879141796091, 65.35873351754847249, -2.061059937946295495 ) ) ;
#35507 = CARTESIAN_POINT ( 'NONE',  ( -1.731684944490798905, -28.88366151015853944, 6.865833476810890623 ) ) ;
#35506 = CARTESIAN_POINT ( 'NONE',  ( 23.59809321522951819, 0.4335636044344673423, 5.517173434541214228 ) ) ;
#35508 = CARTESIAN_POINT ( 'NONE',  ( 81.53035370526046677, 63.02147265739189663, -3.059106349689736160 ) ) ;
#35509 = CARTESIAN_POINT ( 'NONE',  ( 79.63188232868596117, 63.19436791590091218, 3.756013696796379087 ) ) ;
#35510 = ORIENTED_EDGE ( 'NONE', *, *, #12641, .F. ) ;
#35511 = VECTOR ( 'NONE', #21590, 1000.000000000000000 ) ;
#35512 = DIRECTION ( 'NONE',  ( 0.000000000000000000, 0.000000000000000000, 1.000000000000000000 ) ) ;
#35513 = CARTESIAN_POINT ( 'NONE',  ( 80.68997016403565681, 66.19852044017257242, 1.342843868341103697 ) ) ;
#35515 = VERTEX_POINT ( 'NONE', #31459 ) ;
#35514 = PLANE ( 'NONE',  #24904 ) ;
#35516 = CARTESIAN_POINT ( 'NONE',  ( 22.53953452546943126, -1.608357795960198677, 9.096105908381383998 ) ) ;
#35517 = FACE_OUTER_BOUND ( 'NONE', #13949, .T. ) ;
#35518 = EDGE_LOOP ( 'NONE', ( #12539, #38713, #27136, #37844, #11603, #35731, #82 ) ) ;
#35519 = CARTESIAN_POINT ( 'NONE',  ( -78.35162830023389802, -5.279867256489808369, 6.711823625471323496 ) ) ;
#35520 = CARTESIAN_POINT ( 'NONE',  ( 3.412070287718869999, -32.50764203308273181, 7.635761828346577573 ) ) ;
#35521 = EDGE_CURVE ( 'NONE', #19820, #3554, #3282, .T. ) ;
#35522 = CARTESIAN_POINT ( 'NONE',  ( -0.1356099412391454651, -32.54423587553223740, 7.771081512783701406 ) ) ;
#35523 = LINE ( 'NONE', #1344, #17037 ) ;
#35524 = VECTOR ( 'NONE', #28936, 1000.000000000000114 ) ;
#35525 = VERTEX_POINT ( 'NONE', #32079 ) ;
#35526 = CARTESIAN_POINT ( 'NONE',  ( 35.22022786365597824, -1.048883770861420039, -5.412378490821479815 ) ) ;
#35527 = CARTESIAN_POINT ( 'NONE',  ( -2.165713543243725780, -26.06083781805162403, 6.954324564059724878 ) ) ;
#35528 = CARTESIAN_POINT ( 'NONE',  ( -1.098727649675871554, -31.67110930927854184, 6.931070083220560285 ) ) ;
#35529 = CARTESIAN_POINT ( 'NONE',  ( 5.001438667734867671, -30.73314912614656436, 7.695279973900954751 ) ) ;
#35530 = FACE_OUTER_BOUND ( 'NONE', #15120, .T. ) ;
#35531 = CARTESIAN_POINT ( 'NONE',  ( -62.92837670882106238, 13.37661300689599742, -6.000000000000000000 ) ) ;
#35532 = CARTESIAN_POINT ( 'NONE',  ( 23.94445520861282972, 1.171759895968547349, -4.943323473430091042 ) ) ;
#35533 = CARTESIAN_POINT ( 'NONE',  ( 34.86059237354090357, -0.8869592652725889481, -5.330962963188696335 ) ) ;
#35534 = FACE_OUTER_BOUND ( 'NONE', #10644, .T. ) ;
#35535 = CARTESIAN_POINT ( 'NONE',  ( 2.244862549643315219, -33.02733246477049533, 6.870737987065013819 ) ) ;
#35536 = ORIENTED_EDGE ( 'NONE', *, *, #24723, .F. ) ;
#35537 = EDGE_CURVE ( 'NONE', #16444, #22296, #27152, .T. ) ;
#35538 = ORIENTED_EDGE ( 'NONE', *, *, #4539, .F. ) ;
#35540 = EDGE_CURVE ( 'NONE', #13794, #37354, #28349, .T. ) ;
#35539 = CARTESIAN_POINT ( 'NONE',  ( 66.56592146697632018, 57.84521198437244038, 3.999917672785076483 ) ) ;
#35541 = EDGE_CURVE ( 'NONE', #14204, #21757, #11515, .T. ) ;
#35542 = AXIS2_PLACEMENT_3D ( 'NONE', #16168, #10185, #740 ) ;
#35543 = FACE_OUTER_BOUND ( 'NONE', #24039, .T. ) ;
#35544 = EDGE_LOOP ( 'NONE', ( #40274, #21478, #14893, #12731, #29604 ) ) ;
#35545 = CARTESIAN_POINT ( 'NONE',  ( -81.60592086609160845, 10.48184527842860980, -2.319392075440308787 ) ) ;
#35546 = B_SPLINE_CURVE_WITH_KNOTS ( 'NONE', 3,
 ( #39267, #23438, #20330, #1621, #30015, #11254, #39676, #14355, #4513, #26925 ),
 .UNSPECIFIED., .F., .F.,
 ( 4, 3, 3, 4 ),
 ( 0.000000000000000000, 3.025570593003334597E-05, 6.051145698344288499E-05, 6.468151674594163625E-05 ),
 .UNSPECIFIED. ) ;
#35547 = APPLICATION_PROTOCOL_DEFINITION ( 'draft international standard', 'automotive_design', 1998, #14482 ) ;
#35548 = CARTESIAN_POINT ( 'NONE',  ( 2.279805425825974119, -32.92020578787989393, 7.775108481317161591 ) ) ;
#35549 = DIRECTION ( 'NONE',  ( 1.000000000000000000, -0.000000000000000000, 0.000000000000000000 ) ) ;
#35550 = ORIENTED_EDGE ( 'NONE', *, *, #29347, .F. ) ;
#35551 = CARTESIAN_POINT ( 'NONE',  ( -1.751664738099543150, -28.99259367712256008, 7.665454363767880253 ) ) ;
#35552 = AXIS2_PLACEMENT_3D ( 'NONE', #36665, #8240, #24518 ) ;
#35553 = ORIENTED_EDGE ( 'NONE', *, *, #29461, .T. ) ;
#35554 = CARTESIAN_POINT ( 'NONE',  ( 78.63837616148840937, 65.82632162494834915, -2.064111563736707566 ) ) ;
#35555 = CARTESIAN_POINT ( 'NONE',  ( 33.88603132824229647, -5.388632132188243773, 1.367569066300536429 ) ) ;
#35556 = B_SPLINE_CURVE_WITH_KNOTS ( 'NONE', 3,
 ( #5507, #4895, #17425, #21367 ),
 .UNSPECIFIED., .F., .F.,
 ( 4, 4 ),
 ( 2.602085213965210642E-18, 0.0006739815419856351204 ),
 .UNSPECIFIED. ) ;
#35557 = CARTESIAN_POINT ( 'NONE',  ( 78.69934701664540455, 65.67047266146715856, 2.368006059520778805 ) ) ;
#35558 = CARTESIAN_POINT ( 'NONE',  ( -89.00859394718985129, 2.429809908903242555, 15.50000000000000000 ) ) ;
#35559 = FACE_OUTER_BOUND ( 'NONE', #28385, .T. ) ;
#35560 = FACE_OUTER_BOUND ( 'NONE', #17223, .T. ) ;
#35561 = PLANE ( 'NONE',  #34096 ) ;
#35562 = CARTESIAN_POINT ( 'NONE',  ( 33.62997687085571386, -4.269399587632154436, -4.589598755017198606 ) ) ;
#35563 = CARTESIAN_POINT ( 'NONE',  ( 3.499140961715896836, -26.68471003353787196, 7.761597726988846091 ) ) ;
#35564 = ORIENTED_EDGE ( 'NONE', *, *, #12594, .T. ) ;
#35565 = CARTESIAN_POINT ( 'NONE',  ( 78.56547728078845694, 65.96989904497856116, -1.378793396233028323 ) ) ;
#35566 = VECTOR ( 'NONE', #16515, 1000.000000000000000 ) ;
#35567 = EDGE_CURVE ( 'NONE', #32407, #14576, #11367, .T. ) ;
#35568 = CARTESIAN_POINT ( 'NONE',  ( 14.75101795178193775, -5.142163552057975373, -2.499999999999998668 ) ) ;
#35569 = CARTESIAN_POINT ( 'NONE',  ( -0.6163032562860591979, -32.18389938704100217, 7.776484688137376367 ) ) ;
#35570 = CARTESIAN_POINT ( 'NONE',  ( -73.12379269740060295, 4.558640974120507394, -9.815543729773533954 ) ) ;
#35571 = CARTESIAN_POINT ( 'NONE',  ( 5.141937666525170592, -28.93293880656905870, 7.660770905198778458 ) ) ;
#35572 = FACE_OUTER_BOUND ( 'NONE', #39603, .T. ) ;
#35573 = CARTESIAN_POINT ( 'NONE',  ( 81.24750358194776823, 61.36520210808431841, 1.450104216466337581 ) ) ;
#35574 = CARTESIAN_POINT ( 'NONE',  ( 87.26468549332315661, -1.699173523771937644, 4.325011594718342067 ) ) ;
#35575 = DIRECTION ( 'NONE',  ( -1.000000000000000000, 0.000000000000000000, 0.000000000000000000 ) ) ;
#35576 = LINE ( 'NONE', #29379, #24699 ) ;
#35577 = CARTESIAN_POINT ( 'NONE',  ( 3.924861072458515565, -26.86775624777466120, 7.720710062488897130 ) ) ;
#35578 = EDGE_CURVE ( 'NONE', #5866, #33153, #26881, .T. ) ;
#35579 = CARTESIAN_POINT ( 'NONE',  ( 1.808121863982283584, -26.17162928199792304, 7.768425012602592439 ) ) ;
#35580 = EDGE_CURVE ( 'NONE', #25319, #19232, #35763, .T. ) ;
#35581 = DIRECTION ( 'NONE',  ( 0.000000000000000000, 0.000000000000000000, 1.000000000000000000 ) ) ;
#35582 = CARTESIAN_POINT ( 'NONE',  ( 4.882868366733327470, -28.37333834040810032, 7.703977250142848732 ) ) ;
#35583 = CARTESIAN_POINT ( 'NONE',  ( -63.08758708074093136, 38.76906266698302517, -3.000000000000000000 ) ) ;
#35584 = CARTESIAN_POINT ( 'NONE',  ( 68.97355662219305827, 59.39279559060015146, 3.921432738910643589 ) ) ;
#35585 = CARTESIAN_POINT ( 'NONE',  ( 36.89727170037077997, -3.002153245520217784, 5.965109631367820242 ) ) ;
#35586 = ADVANCED_FACE ( 'NONE', ( #24143 ), #30130, .F. ) ;
#35587 = CARTESIAN_POINT ( 'NONE',  ( 7.021324086407807030, -24.55319635012989110, 6.800000000000000711 ) ) ;
#35588 = CARTESIAN_POINT ( 'NONE',  ( 86.54367451126900335, 1.050056116286632646, -5.670096781828877219 ) ) ;
#35590 = CARTESIAN_POINT ( 'NONE',  ( 4.817694033729734038, -30.92728660960060338, 6.969307238440502594 ) ) ;
#35589 = CARTESIAN_POINT ( 'NONE',  ( 78.73750597996149736, 66.05139304066524630, -1.520709669156475430 ) ) ;
#35591 = PLANE ( 'NONE',  #37921 ) ;
#35592 = CARTESIAN_POINT ( 'NONE',  ( 4.360557156959933955, -27.29539480379102656, 7.670465701733752084 ) ) ;
#35593 = ORIENTED_EDGE ( 'NONE', *, *, #35456, .F. ) ;
#35594 = VECTOR ( 'NONE', #20555, 1000.000000000000000 ) ;
#35595 = CARTESIAN_POINT ( 'NONE',  ( 4.907464300517769829, -30.69894525369553762, 7.703977250142849620 ) ) ;
#35596 = EDGE_LOOP ( 'NONE', ( #5753, #21062, #12123, #26483 ) ) ;
#35597 = CARTESIAN_POINT ( 'NONE',  ( -71.36981149190343388, -21.68728802194536698, 3.984496351204982467 ) ) ;
#35598 = ORIENTED_EDGE ( 'NONE', *, *, #36764, .T. ) ;
#35599 = CARTESIAN_POINT ( 'NONE',  ( 78.96452808758077424, 65.70328965153812817, -2.526545245021140307 ) ) ;
#35600 =( BOUNDED_CURVE ( )  B_SPLINE_CURVE ( 3, ( #17219, #29791, #1604, #12780 ),
 .UNSPECIFIED., .F., .T. ) 
 B_SPLINE_CURVE_WITH_KNOTS ( ( 4, 4 ),
 ( 4.748221474220559735, 4.941946782021394036 ),
 .UNSPECIFIED. ) 
 CURVE ( )  GEOMETRIC_REPRESENTATION_ITEM ( )  RATIONAL_B_SPLINE_CURVE ( ( 1.000000000000000000, 0.9968749865767494445, 0.9968749865767494445, 1.000000000000000000 ) ) 
 REPRESENTATION_ITEM ( '' )  );
#35601 = AXIS2_PLACEMENT_3D ( 'NONE', #7187, #23441, #38873 ) ;
#35602 = CARTESIAN_POINT ( 'NONE',  ( -28.24874870218063805, -26.64985754041175525, 6.700000000000000178 ) ) ;
#35603 = CARTESIAN_POINT ( 'NONE',  ( 23.60946143526467722, 2.060598013451824251, 4.567481006929359211 ) ) ;
#35604 = ORIENTED_EDGE ( 'NONE', *, *, #10903, .T. ) ;
#35605 = VECTOR ( 'NONE', #20003, 999.9999999999998863 ) ;
#35606 = DIRECTION ( 'NONE',  ( -1.000000000000000000, 0.000000000000000000, 0.000000000000000000 ) ) ;
#35608 = DIRECTION ( 'NONE',  ( -0.9848077530122092416, 0.1736481776669241694, -0.000000000000000000 ) ) ;
#35607 = CARTESIAN_POINT ( 'NONE',  ( -59.00613449831566726, 28.05080808729636743, -6.322111786795005628 ) ) ;
#35609 = CARTESIAN_POINT ( 'NONE',  ( -8.248748702180632719, -25.49307895267003587, 6.700000000000000178 ) ) ;
#35610 = CARTESIAN_POINT ( 'NONE',  ( 70.83363217041421933, 59.75074159095914439, 3.963404584535427322 ) ) ;
#35611 = CARTESIAN_POINT ( 'NONE',  ( 22.33768170137506814, 4.516987467366701203, -3.522961905446787334 ) ) ;
#35612 = ORIENTED_EDGE ( 'NONE', *, *, #40257, .T. ) ;
#35613 = CARTESIAN_POINT ( 'NONE',  ( 5.131276765095678982, -30.20322308033647118, 7.781480525794718162 ) ) ;
#35614 = ORIENTED_EDGE ( 'NONE', *, *, #31920, .T. ) ;
#35615 = EDGE_CURVE ( 'NONE', #30983, #27757, #395, .T. ) ;
#35616 = CARTESIAN_POINT ( 'NONE',  ( 21.85643539959777115, -1.469530054879572223, 14.38030055974112464 ) ) ;
#35617 = CARTESIAN_POINT ( 'NONE',  ( 18.10407751947404265, 13.71956107776613543, 3.198739209386171733 ) ) ;
#35618 = EDGE_LOOP ( 'NONE', ( #9442, #40366, #14044, #29830, #18283 ) ) ;
#35619 = CARTESIAN_POINT ( 'NONE',  ( 0.3455553403917285271, -32.68833086202552352, 6.929923840112063083 ) ) ;
#35620 = CARTESIAN_POINT ( 'NONE',  ( 81.69418451911097634, 62.49370361017244591, 2.611089443243005181 ) ) ;
#35621 = CARTESIAN_POINT ( 'NONE',  ( 85.86339947292255204, 1.596523033150343718, -5.427711696011725984 ) ) ;
#35622 = DIRECTION ( 'NONE',  ( 0.000000000000000000, 0.000000000000000000, 1.000000000000000000 ) ) ;
#35623 = ORIENTED_EDGE ( 'NONE', *, *, #17372, .T. ) ;
#35624 = DIRECTION ( 'NONE',  ( -0.000000000000000000, 1.000000000000000000, -0.000000000000000000 ) ) ;
#35625 = CARTESIAN_POINT ( 'NONE',  ( 31.02717173337874002, -3.764723011120618690, 4.607707110895616687 ) ) ;
#35626 = CARTESIAN_POINT ( 'NONE',  ( -6.248748702180631831, -25.49307895267003587, 6.700000000000000178 ) ) ;
#35627 = CARTESIAN_POINT ( 'NONE',  ( 36.91040168402551558, -2.640011690967155378, -5.967158882866976377 ) ) ;
#35628 = DIRECTION ( 'NONE',  ( -0.000000000000000000, -0.000000000000000000, 1.000000000000000000 ) ) ;
#35629 = CARTESIAN_POINT ( 'NONE',  ( 84.47382700867750316, 2.558083702081526134, -3.350542113956249679 ) ) ;
#35630 = DIRECTION ( 'NONE',  ( -0.000000000000000000, -0.000000000000000000, -1.000000000000000000 ) ) ;
#35631 = CARTESIAN_POINT ( 'NONE',  ( 3.860356151429478189, -26.94418059254374143, 7.670860738520325128 ) ) ;
#35632 = EDGE_CURVE ( 'NONE', #32941, #39924, #8279, .T. ) ;
#35633 = EDGE_CURVE ( 'NONE', #24927, #13035, #5214, .T. ) ;
#35634 = CARTESIAN_POINT ( 'NONE',  ( -1.641525177248355893, -30.19571155489859393, 7.703977250142848732 ) ) ;
#35635 = VECTOR ( 'NONE', #37646, 1000.000000000000000 ) ;
#35636 = EDGE_CURVE ( 'NONE', #1269, #40280, #30958, .T. ) ;
#35637 = CARTESIAN_POINT ( 'NONE',  ( 30.74906057277648586, -3.703379513678140444, 4.639682255467033833 ) ) ;
#35638 = ORIENTED_EDGE ( 'NONE', *, *, #1267, .T. ) ;
#35639 = EDGE_LOOP ( 'NONE', ( #22329, #10135, #37742, #32595 ) ) ;
#35640 = CARTESIAN_POINT ( 'NONE',  ( 35.73082939662619140, -1.303437433980812576, 5.537266709372846485 ) ) ;
#35641 = CARTESIAN_POINT ( 'NONE',  ( -1.644222468574767726, -30.60122393950611652, 7.006908160621410531 ) ) ;
#35642 = CARTESIAN_POINT ( 'NONE',  ( 66.27376694609004915, 57.73522568913436004, -4.000000000000000000 ) ) ;
#35643 = CARTESIAN_POINT ( 'NONE',  ( 86.76920234060486337, -1.029458178097735654, 5.350787913367871518 ) ) ;
#35644 = EDGE_LOOP ( 'NONE', ( #17328, #22082, #24277, #31426 ) ) ;
#35645 = CARTESIAN_POINT ( 'NONE',  ( -70.92837670882107659, -56.35932253828835314, 0.000000000000000000 ) ) ;
#35646 = SHAPE_REPRESENTATION_RELATIONSHIP ( 'NONE' , 'NONE' ,  #39290, #17602 ) ;
#35647 = CARTESIAN_POINT ( 'NONE',  ( -57.95974551600830438, 28.52258727176714004, -2.765331207962145932 ) ) ;
#35648 = CARTESIAN_POINT ( 'NONE',  ( 3.807593891317279766, -32.36451543350154481, 6.912143950357347855 ) ) ;
#35649 = EDGE_LOOP ( 'NONE', ( #33148, #19630, #11751, #5159 ) ) ;
#35650 = CARTESIAN_POINT ( 'NONE',  ( 21.89662549548976500, 5.563294812639966835, 3.306681051183087305 ) ) ;
#35651 = CARTESIAN_POINT ( 'NONE',  ( 79.63539728012710839, 66.30663591242939958, -1.358135763685573760 ) ) ;
#35652 = DIRECTION ( 'NONE',  ( 0.000000000000000000, 0.000000000000000000, 1.000000000000000000 ) ) ;
#35653 = DIRECTION ( 'NONE',  ( 1.000000000000000000, 0.000000000000000000, 0.000000000000000000 ) ) ;
#35654 = ORIENTED_EDGE ( 'NONE', *, *, #17343, .T. ) ;
#35655 = CARTESIAN_POINT ( 'NONE',  ( 76.23342353645792002, 61.41352271612331037, -3.867068906741287115 ) ) ;
#35657 = CARTESIAN_POINT ( 'NONE',  ( 4.442938236509021976, -27.40294606746516592, 7.771081512783700518 ) ) ;
#35656 = CARTESIAN_POINT ( 'NONE',  ( 2.454444230655590697, -26.15211026017857421, 6.877402575842992860 ) ) ;
#35658 = CARTESIAN_POINT ( 'NONE',  ( 22.27817917822705951, 5.092324266975621683, -3.633448080353249399 ) ) ;
#35659 = CARTESIAN_POINT ( 'NONE',  ( 75.68803578311079150, 63.95394130778559116, 2.805892758485419414 ) ) ;
#35660 = ORIENTED_EDGE ( 'NONE', *, *, #23205, .F. ) ;
#35661 = VERTEX_POINT ( 'NONE', #34671 ) ;
#35662 = DIRECTION ( 'NONE',  ( -0.000000000000000000, -0.000000000000000000, -1.000000000000000000 ) ) ;
#35663 = B_SPLINE_CURVE_WITH_KNOTS ( 'NONE', 3,
 ( #7926, #16035, #29555, #26076 ),
 .UNSPECIFIED., .F., .F.,
 ( 4, 4 ),
 ( 0.000000000000000000, 6.391136169993375584E-06 ),
 .UNSPECIFIED. ) ;
#35664 = DIRECTION ( 'NONE',  ( -1.000000000000000000, -0.000000000000000000, -0.000000000000000000 ) ) ;
#35665 = DIRECTION ( 'NONE',  ( -0.000000000000000000, -0.000000000000000000, -1.000000000000000000 ) ) ;
#35666 = DIRECTION ( 'NONE',  ( 1.000000000000000000, 0.000000000000000000, 0.000000000000000000 ) ) ;
#35667 = CARTESIAN_POINT ( 'NONE',  ( 80.99701317011684409, 65.74337749817958354, 2.326649614737514860 ) ) ;
#35668 = CARTESIAN_POINT ( 'NONE',  ( 85.75774791330482572, 2.030551832223961295, -3.840166728450957301 ) ) ;
#35669 = CARTESIAN_POINT ( 'NONE',  ( 32.01248540970218670, -4.887874588265229470, -2.123135123820048875 ) ) ;
#35670 = CARTESIAN_POINT ( 'NONE',  ( 2.410368835147195021, -26.24488429107400478, 7.754798119455333705 ) ) ;
#35671 = DIRECTION ( 'NONE',  ( -0.000000000000000000, -0.000000000000000000, -1.000000000000000000 ) ) ;
#35672 = CIRCLE ( 'NONE', #17876, 0.1000000000000028644 ) ;
#35673 = CARTESIAN_POINT ( 'NONE',  ( 2.428848143534461101, -33.77897949353074836, 7.635761828346577573 ) ) ;
#35674 = CARTESIAN_POINT ( 'NONE',  ( -0.5222078730473904695, -32.14287757506037480, 6.894806418505348589 ) ) ;
#35675 = CARTESIAN_POINT ( 'NONE',  ( 3.922483456672745561, -26.86580350659783178, 7.686927408461905920 ) ) ;
#35676 = CARTESIAN_POINT ( 'NONE',  ( 31.86214199327330121, -0.1501766581728601335, -5.152687107714187142 ) ) ;
#35677 = PLANE ( 'NONE',  #6899 ) ;
#35678 = DIRECTION ( 'NONE',  ( 1.000000000000000000, 0.000000000000000000, 0.000000000000000000 ) ) ;
#35679 = DIRECTION ( 'NONE',  ( 1.000000000000000000, 0.000000000000000000, 0.000000000000000000 ) ) ;
#35680 = CARTESIAN_POINT ( 'NONE',  ( -1.559944549550448922, -28.33713295695417145, 7.785096263473211486 ) ) ;
#35681 = DIRECTION ( 'NONE',  ( -0.000000000000000000, -0.000000000000000000, -1.000000000000000000 ) ) ;
#35682 = EDGE_CURVE ( 'NONE', #22296, #18803, #40153, .T. ) ;
#35683 = CYLINDRICAL_SURFACE ( 'NONE', #13211, 6.000000000000005329 ) ;
#35684 = EDGE_CURVE ( 'NONE', #18734, #13498, #18133, .T. ) ;
#35685 = ORIENTED_EDGE ( 'NONE', *, *, #9864, .F. ) ;
#35686 = CARTESIAN_POINT ( 'NONE',  ( 36.46016930148370250, -3.391369413551937217, 5.869954818313481759 ) ) ;
#35687 = DIRECTION ( 'NONE',  ( -1.000000000000000000, 0.000000000000000000, 0.000000000000000000 ) ) ;
#35688 = CARTESIAN_POINT ( 'NONE',  ( 67.42350544106223253, 58.22289815522609047, -3.997566301760141272 ) ) ;
#35689 = CARTESIAN_POINT ( 'NONE',  ( 4.715112165605915173, -27.79188326996616709, 7.670465701733750308 ) ) ;
#35690 = ORIENTED_EDGE ( 'NONE', *, *, #29069, .T. ) ;
#35691 = CARTESIAN_POINT ( 'NONE',  ( -16.44874870218064089, -26.64985754041175525, 6.700000000000000178 ) ) ;
#35692 = CARTESIAN_POINT ( 'NONE',  ( -64.08758708074094557, 36.44316031593028526, 3.600279212593497480 ) ) ;
#35693 = CARTESIAN_POINT ( 'NONE',  ( 78.69038500580363404, 66.05859403932464602, 1.000000000000000000 ) ) ;
#35694 = CARTESIAN_POINT ( 'NONE',  ( 2.326171464738295835, -32.91184545387483951, 7.695279973900954751 ) ) ;
#35695 = CARTESIAN_POINT ( 'NONE',  ( 3.608358685920158848, -26.63570720646865198, 6.989977667959445640 ) ) ;
#35696 = CIRCLE ( 'NONE', #15963, 3.499999999999999556 ) ;
#35697 = CARTESIAN_POINT ( 'NONE',  ( 4.393959771609395659, -31.80480879032751673, 7.643192810543820492 ) ) ;
#35698 = ORIENTED_EDGE ( 'NONE', *, *, #17592, .T. ) ;
#35699 = CARTESIAN_POINT ( 'NONE',  ( 22.87846517050438067, 4.335907691735916281, 3.060191673758243969 ) ) ;
#35700 = CARTESIAN_POINT ( 'NONE',  ( 81.26055678261324999, 61.79680472324191243, 2.407735119910396016 ) ) ;
#35701 = CARTESIAN_POINT ( 'NONE',  ( -63.57031559648750374, 43.64086948594911064, 2.909459873249482076 ) ) ;
#35702 = VERTEX_POINT ( 'NONE', #16108 ) ;
#35703 = CARTESIAN_POINT ( 'NONE',  ( 79.57145864546818359, 62.55878779196849848, -3.641957811749160445 ) ) ;
#35705 = CARTESIAN_POINT ( 'NONE',  ( -1.709989797022098301, -28.78296037949930408, 6.995077437911115581 ) ) ;
#35704 = CARTESIAN_POINT ( 'NONE',  ( 26.71945218434455427, 0.9447924085842542841, 4.381674605026809388 ) ) ;
#35706 = CARTESIAN_POINT ( 'NONE',  ( 80.65926296283754482, 64.83599339274806539, -3.316380171282755196 ) ) ;
#35707 = ADVANCED_FACE ( 'NONE', ( #3385 ), #21686, .F. ) ;
#35708 = CARTESIAN_POINT ( 'NONE',  ( 80.51696178947716476, 61.27878891920005344, 2.305838555345019802 ) ) ;
#35709 = ORIENTED_EDGE ( 'NONE', *, *, #4092, .T. ) ;
#35710 = PLANE ( 'NONE',  #5016 ) ;
#35711 = CARTESIAN_POINT ( 'NONE',  ( 80.71704827558885142, 66.21292280724348700, 1.118100487915077546 ) ) ;
#35712 = DIRECTION ( 'NONE',  ( -0.000000000000000000, 1.000000000000000000, -0.000000000000000000 ) ) ;
#35713 = CARTESIAN_POINT ( 'NONE',  ( 22.81791704898701667, -6.824503531841428661, 2.299112860430994054 ) ) ;
#35714 = CARTESIAN_POINT ( 'NONE',  ( -55.15112219448760555, 31.23515184556838165, 9.800414904976365804 ) ) ;
#35715 = ORIENTED_EDGE ( 'NONE', *, *, #29842, .T. ) ;
#35716 = CARTESIAN_POINT ( 'NONE',  ( -72.63519498226254711, -1.653156654010232041, 9.855318911829444417 ) ) ;
#35717 = CARTESIAN_POINT ( 'NONE',  ( 24.12370628256579508, 0.4970018228905133673, -5.094551904089473560 ) ) ;
#35718 = EDGE_CURVE ( 'NONE', #12332, #23121, #35286, .T. ) ;
#35719 = CARTESIAN_POINT ( 'NONE',  ( -0.9821796830226547925, -31.80934223257329663, 7.773839561854631874 ) ) ;
#35720 = CARTESIAN_POINT ( 'NONE',  ( 36.88786849831456749, -3.351047888682084697, -5.910680165042082379 ) ) ;
#35721 = CARTESIAN_POINT ( 'NONE',  ( 30.79114401576465809, -3.336758667098143061, -4.962072607841499838 ) ) ;
#35722 = CARTESIAN_POINT ( 'NONE',  ( -13.07867591359219617, -26.64985754041175525, 6.700000000000000178 ) ) ;
#35723 = CARTESIAN_POINT ( 'NONE',  ( 5.126355467162643009, -30.28602164449890566, 6.864641613908471385 ) ) ;
#35724 = DIRECTION ( 'NONE',  ( 1.000000000000000000, 0.000000000000000000, 0.000000000000000000 ) ) ;
#35725 = CARTESIAN_POINT ( 'NONE',  ( 5.095244238841699413, -29.75692037041947913, 7.013842709614101167 ) ) ;
#35726 = CARTESIAN_POINT ( 'NONE',  ( 5.585000075404096265, -26.15135101585522293, 7.754798119455333705 ) ) ;
#35727 = AXIS2_PLACEMENT_3D ( 'NONE', #11458, #33115, #20529 ) ;
#35728 = CARTESIAN_POINT ( 'NONE',  ( 1.892862797245994821, -26.07522642238200561, 6.961115707816238007 ) ) ;
#35729 = CARTESIAN_POINT ( 'NONE',  ( 4.337032230407563915, -31.84938093442232088, 7.785344483711591934 ) ) ;
#35730 = ADVANCED_FACE ( 'NONE', ( #21480 ), #15699, .F. ) ;
#35731 = ORIENTED_EDGE ( 'NONE', *, *, #40430, .T. ) ;
#35732 = B_SPLINE_CURVE_WITH_KNOTS ( 'NONE', 3,
 ( #37140, #21512, #30786, #34491, #6265, #21303, #18812, #21101, #39248, #11039, #11798, #18401, #37343, #23616, #36182, #21711, #5449, #2793, #8519, #33878, #17990, #30576, #2383, #34296, #27871, #34088, #40632, #40419, #12224, #14905, #6064 ),
 .UNSPECIFIED., .F., .F.,
 ( 4, 3, 3, 3, 3, 3, 3, 3, 3, 3, 4 ),
 ( 2.168404344971008868E-19, 2.999644130997720782E-05, 6.002588995694745999E-05, 8.960886084588085281E-05, 0.0001190604700446486864, 0.0001489538463052727233, 0.0001796139255493992102, 0.0002109707048517083525, 0.0002426195318110370642, 0.0002740640997890074850, 0.0002849778069099842027 ),
 .UNSPECIFIED. ) ;
#35733 = VERTEX_POINT ( 'NONE', #28251 ) ;
#35734 = CARTESIAN_POINT ( 'NONE',  ( 66.87313677512783272, 57.91234881663538658, 3.999382933222194847 ) ) ;
#35735 = CARTESIAN_POINT ( 'NONE',  ( 72.04157359233609270, 60.08177168861285367, -3.962431611490357053 ) ) ;
#35736 = CARTESIAN_POINT ( 'NONE',  ( 2.290977028701361107, -26.12011756940199447, 7.750000000000000888 ) ) ;
#35737 = AXIS2_PLACEMENT_3D ( 'NONE', #37327, #17970, #40405 ) ;
#35738 = CARTESIAN_POINT ( 'NONE',  ( 87.47045099524558509, -1.608924759093422807, 4.367130927193085377 ) ) ;
#35739 = CARTESIAN_POINT ( 'NONE',  ( 2.863609035986291573, -26.26888160889163615, 7.695279973900954751 ) ) ;
#35740 = APPLICATION_PROTOCOL_DEFINITION ( 'draft international standard', 'automotive_design', 1998, #27896 ) ;
#35741 = CARTESIAN_POINT ( 'NONE',  ( 2.948025465462910777, -26.31577733493585569, 7.785593909369613819 ) ) ;
#35742 = PLANE ( 'NONE',  #39089 ) ;
#35743 = EDGE_CURVE ( 'NONE', #34769, #38692, #40600, .T. ) ;
#35744 = EDGE_LOOP ( 'NONE', ( #4729, #7593, #9095, #40580, #29820 ) ) ;
#35745 = CARTESIAN_POINT ( 'NONE',  ( -1.748756095191392523, -28.97546355617463121, 7.635761828346576685 ) ) ;
#35746 = AXIS2_PLACEMENT_3D ( 'NONE', #11794, #40025, #20883 ) ;
#35747 = ORIENTED_EDGE ( 'NONE', *, *, #33230, .F. ) ;
#35748 = CARTESIAN_POINT ( 'NONE',  ( 80.67643653137164961, 61.85813826494483436, -2.902290250791175197 ) ) ;
#35749 = CARTESIAN_POINT ( 'NONE',  ( 37.07689334178120077, -2.357884832068502856, 5.940193581006886880 ) ) ;
#35750 = CARTESIAN_POINT ( 'NONE',  ( 78.75315097705565393, 65.71977079011902845, 2.326060681237297256 ) ) ;
#35752 = VERTEX_POINT ( 'NONE', #12809 ) ;
#35751 = CARTESIAN_POINT ( 'NONE',  ( -1.270646089883737506, -31.22309432593480594, 6.889465824494256374 ) ) ;
#35753 = DIRECTION ( 'NONE',  ( -0.000000000000000000, -0.000000000000000000, -1.000000000000000000 ) ) ;
#35754 = CARTESIAN_POINT ( 'NONE',  ( 18.29952987130526765, 8.276640680725938282, -2.983475682558551334 ) ) ;
#35755 = LINE ( 'NONE', #19887, #22245 ) ;
#35756 = EDGE_CURVE ( 'NONE', #40083, #35192, #21885, .T. ) ;
#35757 = CARTESIAN_POINT ( 'NONE',  ( 33.45716606812183613, -3.829385970599605393, -5.093809925484540813 ) ) ;
#35758 = CARTESIAN_POINT ( 'NONE',  ( 21.71434179704859346, 6.308304841617775161, -3.200288761970310869 ) ) ;
#35759 = ORIENTED_EDGE ( 'NONE', *, *, #10784, .F. ) ;
#35760 = B_SPLINE_CURVE_WITH_KNOTS ( 'NONE', 3,
 ( #11540, #24109, #36673, #8457, #34845, #22067, #12161, #16078, #18967, #34233, #238, #13494, #9232, #9645, #37235, #34390, #6576, #34188, #6162 ),
 .UNSPECIFIED., .F., .F.,
 ( 4, 3, 3, 3, 3, 3, 4 ),
 ( 3.252606517456513302E-19, 2.546128104244800008E-05, 5.711050680483939474E-05, 8.113074941675944753E-05, 0.0001053129305727065632, 0.0001360598016347085713, 0.0001612931755702024352 ),
 .UNSPECIFIED. ) ;
#35761 = DIRECTION ( 'NONE',  ( -0.1736481776669340227, 0.9848077530122074652, -0.000000000000000000 ) ) ;
#35762 = ADVANCED_FACE ( 'NONE', ( #37111 ), #6848, .F. ) ;
#35763 = LINE ( 'NONE', #30336, #4329 ) ;
#35764 = DIRECTION ( 'NONE',  ( 0.000000000000000000, 1.000000000000000000, 0.000000000000000000 ) ) ;
#35765 = AXIS2_PLACEMENT_3D ( 'NONE', #30319, #33627, #2128 ) ;
#35766 = CARTESIAN_POINT ( 'NONE',  ( -76.37480731197182138, -4.247693215982008219, -9.858617499677098550 ) ) ;
#35767 = CARTESIAN_POINT ( 'NONE',  ( -0.02174174371171335232, -26.63833058205436899, 7.652160403243381204 ) ) ;
#35768 = FACE_OUTER_BOUND ( 'NONE', #3237, .T. ) ;
#35769 = CARTESIAN_POINT ( 'NONE',  ( 81.24448906778437163, 62.55865020921709885, 3.071811904357649947 ) ) ;
#35770 = CARTESIAN_POINT ( 'NONE',  ( -1.488097077937502899, -30.75041718428775184, 7.748216051605120391 ) ) ;
#35771 = CARTESIAN_POINT ( 'NONE',  ( -1.576062547484235354, -30.80072589882973944, 7.695279973900954751 ) ) ;
#35772 = DIRECTION ( 'NONE',  ( -0.1736481776669207000, -0.9848077530122097967, -0.000000000000000000 ) ) ;
#35773 = VECTOR ( 'NONE', #10141, 1000.000000000000000 ) ;
#35774 = CARTESIAN_POINT ( 'NONE',  ( 4.501207559045222517, -27.47102055165149892, 6.961115707816242448 ) ) ;
#35775 = CYLINDRICAL_SURFACE ( 'NONE', #18660, 5.950000000000010836 ) ;
#35776 = CARTESIAN_POINT ( 'NONE',  ( 1.300000000000000044, 0.000000000000000000, 0.000000000000000000 ) ) ;
#35777 = EDGE_CURVE ( 'NONE', #6472, #3076, #29076, .T. ) ;
#35778 = CARTESIAN_POINT ( 'NONE',  ( 22.92125608552839466, 2.653312946985113552, 3.783814383456351127 ) ) ;
#35779 = DIRECTION ( 'NONE',  ( 1.000000000000000000, 0.000000000000000000, 0.000000000000000000 ) ) ;
#35780 = CARTESIAN_POINT ( 'NONE',  ( 85.38025200535193449, 2.454573153073208225, 3.240196491381199362 ) ) ;
#35782 = CARTESIAN_POINT ( 'NONE',  ( -0.4037637910173453304, -26.77305041633264793, 6.921725064902943814 ) ) ;
#35781 = CARTESIAN_POINT ( 'NONE',  ( 78.83705574937599181, 66.00318003113706311, -1.852607187800925148 ) ) ;
#35783 = B_SPLINE_CURVE_WITH_KNOTS ( 'NONE', 3,
 ( #7004, #10287, #26547, #7403, #22861, #13789, #29239, #1252, #16465, #10082, #36024, #20354, #19762, #23456, #22668, #29037, #4337, #7604, #13978, #1047, #38687, #7801, #10484, #35829, #841, #32343, #10882, #38482, #35629, #23064, #32538, #10681, #20156, #32738, #13373, #32933, #4721, #20418, #20023, #38753, #36281, #32999, #33421, #27012, #13849, #36481, #7466, #23323, #10547, #26815, #20615, #33201, #26419, #1506, #23125, #39557, #14040, #32604, #35892, #4402, #20825, #1314, #16923, #4593, #1711, #11341, #38948, #17723, #36093, #26221, #26615, #8056 ),
 .UNSPECIFIED., .F., .F.,
 ( 4, 2, 2, 2, 2, 2, 2, 2, 1, 1, 1, 1, 1, 2, 2, 2, 2, 2, 1, 1, 1, 1, 1, 2, 2, 2, 2, 1, 1, 1, 1, 1, 2, 2, 2, 1, 1, 1, 2, 2, 2, 1, 1, 1, 1, 2, 4 ),
 ( 0.5000000000000000000, 0.5601148001498211793, 0.6202296002996423585, 0.6502870003745532257, 0.6803444004494640929, 0.7104018005243749601, 0.7404592005992858272, 0.7406940240373710571, 0.7409288474754562870, 0.7413984943516267467, 0.7423377881039677773, 0.7442163756086496162, 0.7479735506180135163, 0.7554879006367413163, 0.7705166006741968054, 0.8005740007491080057, 0.8606888008989305172, 0.8609236243370157471, 0.8611584477751008659, 0.8616280946512711036, 0.8625673884036118011, 0.8644459759082925299, 0.8682031509176542095, 0.8757175009363780127, 0.8907462009738250641, 0.9208036010487191669, 0.9210384244868041748, 0.9212732479248892936, 0.9217428948010597534, 0.9226821885534011169, 0.9245607760580834000, 0.9283179510674484103, 0.9358323010861785418, 0.9508610011236386939, 0.9513306479998092646, 0.9518002948759799464, 0.9527395886283216431, 0.9546181761330045923, 0.9583753511423709348, 0.9658897011611035088, 0.9661245245991884056, 0.9663593480372733024, 0.9668289949134435401, 0.9677682886657839045, 0.9696468761704649664, 0.9734040511798274231, 0.9809184011985525586 ),
 .UNSPECIFIED. ) ;
#35784 = CARTESIAN_POINT ( 'NONE',  ( -1.239502271792400689, -27.67071116441090695, 7.006908160621413195 ) ) ;
#35785 = CARTESIAN_POINT ( 'NONE',  ( -58.49128007771433602, 30.53048970692593400, 5.009453334674668135 ) ) ;
#35786 = VERTEX_POINT ( 'NONE', #13828 ) ;
#35787 = CARTESIAN_POINT ( 'NONE',  ( -80.56383756236691340, 11.49139298559813582, -2.708314019505869474 ) ) ;
#35788 = DIRECTION ( 'NONE',  ( 1.000000000000000000, -0.000000000000000000, 0.000000000000000000 ) ) ;
#35789 = ORIENTED_EDGE ( 'NONE', *, *, #32551, .F. ) ;
#35790 = FACE_OUTER_BOUND ( 'NONE', #24127, .T. ) ;
#35791 = AXIS2_PLACEMENT_3D ( 'NONE', #13435, #26012, #38542 ) ;
#35792 = VECTOR ( 'NONE', #30422, 1000.000000000000000 ) ;
#35793 = AXIS2_PLACEMENT_3D ( 'NONE', #28925, #19048, #31612 ) ;
#35794 = VERTEX_POINT ( 'NONE', #32782 ) ;
#35795 = CARTESIAN_POINT ( 'NONE',  ( 80.10672643282856598, 63.77302114994530768, -3.692178340560190453 ) ) ;
#35796 = DIRECTION ( 'NONE',  ( -0.000000000000000000, 0.000000000000000000, -1.000000000000000000 ) ) ;
#35797 = CARTESIAN_POINT ( 'NONE',  ( 79.92294945466714751, 64.42298636752006757, 3.607546830629786427 ) ) ;
#35798 = CARTESIAN_POINT ( 'NONE',  ( 25.78559136093029380, 1.048118573953673582, 4.433432929157029356 ) ) ;
#35799 = DIRECTION ( 'NONE',  ( 0.6427876096865481337, -0.7660444431189707970, -0.000000000000000000 ) ) ;
#35800 = AXIS2_PLACEMENT_3D ( 'NONE', #20405, #10338, #10727 ) ;
#35801 = B_SPLINE_CURVE_WITH_KNOTS ( 'NONE', 3,
 ( #10537, #3796, #22916, #28479, #286, #28890, #13234, #6865, #1107, #6667, #19419, #698, #29091, #38335, #3998 ),
 .UNSPECIFIED., .F., .F.,
 ( 4, 1, 1, 1, 1, 1, 1, 1, 2, 2, 4 ),
 ( 0.000000000000000000, 0.2500000000002247647, 0.3750000000003386735, 0.4375000000003986811, 0.4687500000004286571, 0.4843750000004435896, 0.4921875000004510281, 0.4960937500004519163, 0.4980468750004553025, 0.5000000000004587442, 1.000000000000000000 ),
 .UNSPECIFIED. ) ;
#35802 = EDGE_CURVE ( 'NONE', #32452, #40515, #30046, .T. ) ;
#35803 = CARTESIAN_POINT ( 'NONE',  ( -0.01738578663354513332, -32.50409796781847405, 7.779495906702013741 ) ) ;
#35804 = CIRCLE ( 'NONE', #30535, 0.1000000000000028644 ) ;
#35806 = CARTESIAN_POINT ( 'NONE',  ( 3.960473582032317363, -32.24238647371081612, 7.635761828346576685 ) ) ;
#35805 = CARTESIAN_POINT ( 'NONE',  ( 37.83867290611771494, -6.084034091406928191, 6.000000000000000000 ) ) ;
#35807 = DIRECTION ( 'NONE',  ( -0.000000000000000000, -0.000000000000000000, -1.000000000000000000 ) ) ;
#35808 = FACE_OUTER_BOUND ( 'NONE', #31905, .T. ) ;
#35809 = CARTESIAN_POINT ( 'NONE',  ( 23.92706582939273474, 3.251021385653534601, -3.516417206103825688 ) ) ;
#35810 = VERTEX_POINT ( 'NONE', #13414 ) ;
#35811 = DIRECTION ( 'NONE',  ( -0.000000000000000000, -0.000000000000000000, -1.000000000000000000 ) ) ;
#35812 = EDGE_CURVE ( 'NONE', #1652, #12108, #15066, .T. ) ;
#35813 = CARTESIAN_POINT ( 'NONE',  ( 22.63946314531691328, -3.430231901737621492, -8.286483013797429464 ) ) ;
#35814 = CARTESIAN_POINT ( 'NONE',  ( 18.03538663863764668, 13.77327480705089258, 8.406736845118375017E-13 ) ) ;
#35815 = CARTESIAN_POINT ( 'NONE',  ( 17.36540171046607384, 9.558839590344177850, 2.500000000000280664 ) ) ;
#35816 = CARTESIAN_POINT ( 'NONE',  ( 0.4503279196356648750, -32.73180316670461565, 6.866852738645443210 ) ) ;
#35817 = CARTESIAN_POINT ( 'NONE',  ( 78.82533416220519484, 66.11379887182081916, 1.400336002811356950 ) ) ;
#35818 = CARTESIAN_POINT ( 'NONE',  ( 88.80100535589549793, -2.068446212231642711, -0.8863989573356614304 ) ) ;
#35819 = FACE_OUTER_BOUND ( 'NONE', #437, .T. ) ;
#35820 = VERTEX_POINT ( 'NONE', #35274 ) ;
#35821 = B_SPLINE_CURVE_WITH_KNOTS ( 'NONE', 3,
 ( #17969, #39812, #11781, #14676, #24571, #24157, #6047, #5845, #8500, #11991 ),
 .UNSPECIFIED., .F., .F.,
 ( 4, 3, 3, 4 ),
 ( 8.673617379884035472E-19, 3.025570593003166546E-05, 6.051145698344096054E-05, 6.468151674593702839E-05 ),
 .UNSPECIFIED. ) ;
#35822 = CARTESIAN_POINT ( 'NONE',  ( 14.62163843994035517, -5.048694678019860937, 2.488458322851438975 ) ) ;
#35823 = CIRCLE ( 'NONE', #1001, 0.1000000000000028644 ) ;
#35824 = AXIS2_PLACEMENT_3D ( 'NONE', #30959, #23737, #36308 ) ;
#35825 = DIRECTION ( 'NONE',  ( -3.491481338843133750E-15, 1.000000000000000000, -0.000000000000000000 ) ) ;
#35826 = CARTESIAN_POINT ( 'NONE',  ( 23.83095679137812084, -2.714704696622131319, -3.925795179799298928 ) ) ;
#35827 = CARTESIAN_POINT ( 'NONE',  ( 25.29653240654878132, 1.736439669007842523, -4.154533699626928644 ) ) ;
#35828 = CARTESIAN_POINT ( 'NONE',  ( 0.5713750229309363382, -32.77700439067807281, 7.693875151218753317 ) ) ;
#35829 = CARTESIAN_POINT ( 'NONE',  ( 84.13406293396636215, 2.976669663089178020, -1.005002158774620069 ) ) ;
#35830 = PLANE ( 'NONE',  #3847 ) ;
#35831 = CARTESIAN_POINT ( 'NONE',  ( 3.858277372750224643, -26.94247466732882756, 7.691066658568944447 ) ) ;
#35832 = VECTOR ( 'NONE', #11498, 1000.000000000000000 ) ;
#35833 = CARTESIAN_POINT ( 'NONE',  ( 1.669309969508061764, -33.06979218437418666, 6.894806418505347700 ) ) ;
#35834 = CARTESIAN_POINT ( 'NONE',  ( 31.25759568107904585, -2.934864719164037794, -5.084901792477391602 ) ) ;
#35835 = ORIENTED_EDGE ( 'NONE', *, *, #40468, .F. ) ;
#35836 = ORIENTED_EDGE ( 'NONE', *, *, #17895, .F. ) ;
#35837 = CARTESIAN_POINT ( 'NONE',  ( 32.06846522142977562, 0.2517277866219041482, 4.728932550735457596 ) ) ;
#35838 =( BOUNDED_CURVE ( )  B_SPLINE_CURVE ( 3, ( #17018, #16821, #35984, #23420 ),
 .UNSPECIFIED., .F., .T. ) 
 B_SPLINE_CURVE_WITH_KNOTS ( ( 4, 4 ),
 ( 1.381924640371169577, 1.574767692156077148 ),
 .UNSPECIFIED. ) 
 CURVE ( )  GEOMETRIC_REPRESENTATION_ITEM ( )  RATIONAL_B_SPLINE_CURVE ( ( 1.000000000000000000, 0.9969033633783033199, 0.9969033633783033199, 1.000000000000000000 ) ) 
 REPRESENTATION_ITEM ( '' )  );
#35839 = CARTESIAN_POINT ( 'NONE',  ( -1.616388873120942593, -30.68750670799986224, 6.865554069792297653 ) ) ;
#35840 = CARTESIAN_POINT ( 'NONE',  ( 66.27376694609004915, 57.73522568913436004, -4.000000000000000000 ) ) ;
#35841 = CARTESIAN_POINT ( 'NONE',  ( 86.23726074625430726, -0.1810272084941833837, 5.933124737898375578 ) ) ;
#35842 = VERTEX_POINT ( 'NONE', #1090 ) ;
#35843 = CARTESIAN_POINT ( 'NONE',  ( 4.916835462155118464, -28.46786787629711668, 6.880147297696980857 ) ) ;
#35844 =( NAMED_UNIT ( * ) PLANE_ANGLE_UNIT ( ) SI_UNIT ( $, .RADIAN. ) );
#35845 = ORIENTED_EDGE ( 'NONE', *, *, #15538, .F. ) ;
#35846 = EDGE_CURVE ( 'NONE', #10250, #36200, #26196, .T. ) ;
#35847 = CARTESIAN_POINT ( 'NONE',  ( 23.67393339541625608, 3.433482753640386242, 3.460823878934576658 ) ) ;
#35848 = CARTESIAN_POINT ( 'NONE',  ( 81.23565735523285980, 65.86993722804045603, -1.793694987646317074 ) ) ;
#35849 = VECTOR ( 'NONE', #22608, 1000.000000000000000 ) ;
#35850 = EDGE_CURVE ( 'NONE', #23072, #25044, #20197, .T. ) ;
#35851 = CARTESIAN_POINT ( 'NONE',  ( -1.225953191357326277, -31.30097466021442187, 7.695279973900954751 ) ) ;
#35852 = ORIENTED_EDGE ( 'NONE', *, *, #32001, .F. ) ;
#35854 = DIRECTION ( 'NONE',  ( 0.000000000000000000, 0.000000000000000000, 1.000000000000000000 ) ) ;
#35853 = CARTESIAN_POINT ( 'NONE',  ( 2.494101229020593724, -26.16111475381571339, 6.974994249511788702 ) ) ;
#35855 = CARTESIAN_POINT ( 'NONE',  ( 20.51835354428452618, 5.903611222923889734, -3.408783327478037695 ) ) ;
#35856 = CARTESIAN_POINT ( 'NONE',  ( 74.85245598970902847, 62.88263772385703732, 3.424891502433892843 ) ) ;
#35857 = EDGE_LOOP ( 'NONE', ( #37731, #16657, #30666, #37275, #33411, #14604, #9472, #13296, #917, #14641, #37159, #15266, #18141, #20934, #36620, #5975, #4979, #26358, #13392, #3161, #9419, #26246, #19130, #323, #29118, #9195, #3462 ) ) ;
#35858 = CARTESIAN_POINT ( 'NONE',  ( 22.89638698299516761, 2.867431784428169816, -4.347809372303917286 ) ) ;
#35859 = DIRECTION ( 'NONE',  ( 0.000000000000000000, 0.000000000000000000, 1.000000000000000000 ) ) ;
#35860 = EDGE_CURVE ( 'NONE', #37042, #14030, #32813, .T. ) ;
#35861 = CIRCLE ( 'NONE', #23361, 0.04999999999999991257 ) ;
#35862 = EDGE_CURVE ( 'NONE', #39757, #2177, #17492, .T. ) ;
#35863 = CYLINDRICAL_SURFACE ( 'NONE', #36151, 31.65266504832700534 ) ;
#35864 = CARTESIAN_POINT ( 'NONE',  ( 0.6711941891205337463, -0.5999999999999994227, -3.974981096219152299 ) ) ;
#35865 = LINE ( 'NONE', #7643, #10961 ) ;
#35866 = CARTESIAN_POINT ( 'NONE',  ( 82.17930952126353361, 63.71034004053225175, 2.400449347018089430 ) ) ;
#35867 = CARTESIAN_POINT ( 'NONE',  ( 87.25792211136258913, 0.3454849704027515567, -4.698443967043519187 ) ) ;
#35868 = CARTESIAN_POINT ( 'NONE',  ( 30.98800548345937855, -0.8519925708576415735, -5.886550247782252221 ) ) ;
#35869 = CARTESIAN_POINT ( 'NONE',  ( -20.87867591359218977, -26.64985754041175525, 6.700000000000000178 ) ) ;
#35870 = CARTESIAN_POINT ( 'NONE',  ( -69.95445451253289093, -21.04503801384016271, 9.952588678376169895 ) ) ;
#35871 = DIRECTION ( 'NONE',  ( 1.000000000000000000, 0.000000000000000000, 0.000000000000000000 ) ) ;
#35872 = CARTESIAN_POINT ( 'NONE',  ( 0.7214101843820232007, -26.31391371107089228, 7.006423389747790331 ) ) ;
#35873 = CARTESIAN_POINT ( 'NONE',  ( 0.006252119912152956024, -26.50725532007327701, 6.870737987065012931 ) ) ;
#35874 = CARTESIAN_POINT ( 'NONE',  ( 23.01850269868070242, 2.906672717470778267, -3.798992069357586487 ) ) ;
#35875 = DIRECTION ( 'NONE',  ( -0.000000000000000000, -0.000000000000000000, 1.000000000000000000 ) ) ;
#35876 = DIRECTION ( 'NONE',  ( -1.000000000000000000, 0.000000000000000000, 0.000000000000000000 ) ) ;
#35877 = DIRECTION ( 'NONE',  ( -0.6427876096865430267, 0.7660444431189749048, -0.000000000000000000 ) ) ;
#35878 = DIRECTION ( 'NONE',  ( -0.8660254037844381525, 0.000000000000000000, 0.5000000000000007772 ) ) ;
#35879 = AXIS2_PLACEMENT_3D ( 'NONE', #33341, #2466, #5118 ) ;
#35880 = CARTESIAN_POINT ( 'NONE',  ( -20.97867591359219475, -24.55319635012989110, 6.800000000000000711 ) ) ;
#35881 = CIRCLE ( 'NONE', #40429, 0.1000000000000028644 ) ;
#35882 = CARTESIAN_POINT ( 'NONE',  ( -14.34874870218063769, -25.49307895267003587, 6.700000000000000178 ) ) ;
#35883 = VERTEX_POINT ( 'NONE', #23692 ) ;
#35884 = CARTESIAN_POINT ( 'NONE',  ( 35.04481386660351205, -1.406658151536976042, 5.661173613261942350 ) ) ;
#35885 = LINE ( 'NONE', #10939, #2824 ) ;
#35886 = CARTESIAN_POINT ( 'NONE',  ( 67.45521008556633547, 58.13638817365040978, -3.998402061830689025 ) ) ;
#35887 = VECTOR ( 'NONE', #24627, 1000.000000000000000 ) ;
#35888 = CARTESIAN_POINT ( 'NONE',  ( 5.081024546220614724, -29.99328066215961996, 7.139196562012270597 ) ) ;
#35889 = ORIENTED_EDGE ( 'NONE', *, *, #39341, .F. ) ;
#35890 = DIRECTION ( 'NONE',  ( -0.000000000000000000, -0.000000000000000000, 1.000000000000000000 ) ) ;
#35891 = CARTESIAN_POINT ( 'NONE',  ( 3.904729273020431712, -32.15854446160317082, 7.740055089680403455 ) ) ;
#35892 = CARTESIAN_POINT ( 'NONE',  ( 85.49121078020223763, 1.153260294498703376, -5.693899337874601230 ) ) ;
#35893 = CARTESIAN_POINT ( 'NONE',  ( 0.9072453234131299116, -32.87612686815500496, 6.979335674598003969 ) ) ;
#35894 = CARTESIAN_POINT ( 'NONE',  ( 0.3246626803113665805, -32.78821847042190996, 6.965379264086542399 ) ) ;
#35895 = DIRECTION ( 'NONE',  ( 1.000000000000000000, 0.000000000000000000, 0.000000000000000000 ) ) ;
#35896 = ORIENTED_EDGE ( 'NONE', *, *, #22528, .T. ) ;
#35897 = CARTESIAN_POINT ( 'NONE',  ( 22.38310836802325099, 4.932112375007561944, 3.055667184124356783 ) ) ;
#35898 = CARTESIAN_POINT ( 'NONE',  ( -1.752498985642892304, -28.99760421947164701, 7.695279973900954751 ) ) ;
#35899 = CARTESIAN_POINT ( 'NONE',  ( 81.20616577872307573, 61.45478060783981533, 1.852607187800907385 ) ) ;
#35900 = CARTESIAN_POINT ( 'NONE',  ( -0.02773757890651329036, -32.61354788820055006, 7.651421919295149365 ) ) ;
#35901 = ORIENTED_EDGE ( 'NONE', *, *, #865, .T. ) ;
#35902 = CARTESIAN_POINT ( 'NONE',  ( 78.94057287092958575, 63.80484286357250312, -3.729426069516720954 ) ) ;
#35904 = CARTESIAN_POINT ( 'NONE',  ( -1.723318791039416764, -28.84314446823831091, 6.866645518795387204 ) ) ;
#35903 = CARTESIAN_POINT ( 'NONE',  ( 27.38238008918371946, 1.067659690267280581, 4.479658769764347959 ) ) ;
#35905 = CARTESIAN_POINT ( 'NONE',  ( 80.14223387231542972, 65.61881967979002184, -2.852119850606566143 ) ) ;
#35906 = CARTESIAN_POINT ( 'NONE',  ( 78.28284693538141426, 65.31437991193503478, 2.608847861177645111 ) ) ;
#35907 = EDGE_CURVE ( 'NONE', #14785, #7534, #33793, .T. ) ;
#35908 = VECTOR ( 'NONE', #34118, 1000.000000000000000 ) ;
#35909 = CYLINDRICAL_SURFACE ( 'NONE', #22111, 0.09010775117053086702 ) ;
#35910 = CIRCLE ( 'NONE', #1064, 4.075022672948151126 ) ;
#35911 = EDGE_CURVE ( 'NONE', #5317, #462, #37864, .T. ) ;
#35912 = CARTESIAN_POINT ( 'NONE',  ( 81.58705100058477910, 65.69127060146946917, 1.444831904608907092 ) ) ;
#35913 = DIRECTION ( 'NONE',  ( -0.000000000000000000, -0.000000000000000000, -1.000000000000000000 ) ) ;
#35914 = CARTESIAN_POINT ( 'NONE',  ( 24.06190720129734473, 2.407014782553678955, 5.659300396313236448 ) ) ;
#35915 = CARTESIAN_POINT ( 'NONE',  ( -62.81463675898083210, 36.67811266762163314, -4.600311178732271244 ) ) ;
#35916 = EDGE_LOOP ( 'NONE', ( #34695, #15203, #24400, #16546, #31328, #29639 ) ) ;
#35917 = CARTESIAN_POINT ( 'NONE',  ( -76.83427164388604069, -4.573425012487537522, 8.089458760140365357 ) ) ;
#35918 = CARTESIAN_POINT ( 'NONE',  ( 25.40388266914231252, 0.6804681363941469385, -4.599446440314822304 ) ) ;
#35919 = VECTOR ( 'NONE', #24557, 1000.000000000000000 ) ;
#35920 = DIRECTION ( 'NONE',  ( -0.000000000000000000, -0.000000000000000000, 1.000000000000000000 ) ) ;
#35921 = VERTEX_POINT ( 'NONE', #36068 ) ;
#35922 = CARTESIAN_POINT ( 'NONE',  ( -0.8786759135921904385, -26.64985754041175525, 6.700000000000000178 ) ) ;
#35923 = ORIENTED_EDGE ( 'NONE', *, *, #26054, .T. ) ;
#35924 = CARTESIAN_POINT ( 'NONE',  ( 33.11160242427654055, -0.1547984075289232930, -4.947179439121399902 ) ) ;
#35925 = CARTESIAN_POINT ( 'NONE',  ( 3.617749134298497538, -32.38632682485276604, 7.505001789837626447 ) ) ;
#35926 = CARTESIAN_POINT ( 'NONE',  ( -1.093319172033571984, -31.67829984452200875, 6.998987538705438993 ) ) ;
#35927 = CARTESIAN_POINT ( 'NONE',  ( 4.995891145035052716, -30.74877403122573938, 7.643192810543820492 ) ) ;
#35928 = CARTESIAN_POINT ( 'NONE',  ( 2.817328913877361618, -32.78123018042540338, 6.894806418505346812 ) ) ;
#35929 = DIRECTION ( 'NONE',  ( 1.000000000000000000, 0.000000000000000000, 0.000000000000000000 ) ) ;
#35930 = DIRECTION ( 'NONE',  ( -0.000000000000000000, -0.000000000000000000, 1.000000000000000000 ) ) ;
#35931 = EDGE_LOOP ( 'NONE', ( #12474, #20563, #9032, #23711 ) ) ;
#35932 = CARTESIAN_POINT ( 'NONE',  ( 66.42396409678352143, 57.78537248076371213, 4.000000000000012434 ) ) ;
#35933 = CARTESIAN_POINT ( 'NONE',  ( 73.22742653720867168, 60.47695785811286839, -3.944160774617319287 ) ) ;
#35934 = CARTESIAN_POINT ( 'NONE',  ( 84.61114100273776728, 2.563204847888557403, 3.486439758113726306 ) ) ;
#35935 = DIRECTION ( 'NONE',  ( 1.000000000000000000, 0.000000000000000000, 0.000000000000000000 ) ) ;
#35936 = VECTOR ( 'NONE', #29949, 1000.000000000000000 ) ;
#35937 = DIRECTION ( 'NONE',  ( -0.000000000000000000, -0.000000000000000000, -1.000000000000000000 ) ) ;
#35938 = DIRECTION ( 'NONE',  ( 0.000000000000000000, 0.000000000000000000, -1.000000000000000000 ) ) ;
#35939 = VECTOR ( 'NONE', #781, 1000.000000000000114 ) ;
#35940 = CARTESIAN_POINT ( 'NONE',  ( 6.089801904741589667, -27.84269339272794852, 7.754798119455333705 ) ) ;
#35941 = DIRECTION ( 'NONE',  ( 0.000000000000000000, 0.000000000000000000, 1.000000000000000000 ) ) ;
#35942 = CARTESIAN_POINT ( 'NONE',  ( 5.053714827962103584, -30.13136871382624804, 7.661510568013096822 ) ) ;
#35943 = ORIENTED_EDGE ( 'NONE', *, *, #34337, .F. ) ;
#35944 = VECTOR ( 'NONE', #36448, 1000.000000000000000 ) ;
#35945 = CARTESIAN_POINT ( 'NONE',  ( 80.80786883982545987, 61.35646782832053248, -2.148686496494742304 ) ) ;
#35946 = CARTESIAN_POINT ( 'NONE',  ( 33.76263401838073008, -4.744560827115999579, 3.708591629391344568 ) ) ;
#35947 = CARTESIAN_POINT ( 'NONE',  ( 80.26059561567569745, 63.13455243780983750, 3.653685850874063501 ) ) ;
#35949 = ORIENTED_EDGE ( 'NONE', *, *, #37960, .F. ) ;
#35948 = FACE_OUTER_BOUND ( 'NONE', #2475, .T. ) ;
#35950 = CARTESIAN_POINT ( 'NONE',  ( -23.07867591359219617, -26.64985754041175525, 6.700000000000000178 ) ) ;
#35951 = EDGE_CURVE ( 'NONE', #4319, #21175, #23410, .T. ) ;
#35952 = CARTESIAN_POINT ( 'NONE',  ( 0.9205786840771784663, -32.98195322516173178, 7.006248344249653037 ) ) ;
#35953 = CARTESIAN_POINT ( 'NONE',  ( -16.87867591359218977, -26.64985754041175525, 6.700000000000000178 ) ) ;
#35954 = CARTESIAN_POINT ( 'NONE',  ( 21.85643539959776760, 9.193408351192362105, 7.099988578988766008 ) ) ;
#35955 = CARTESIAN_POINT ( 'NONE',  ( -14.24874870218063450, -26.64985754041175525, 6.800000000000000711 ) ) ;
#35956 = ORIENTED_EDGE ( 'NONE', *, *, #29522, .T. ) ;
#35957 = CARTESIAN_POINT ( 'NONE',  ( 5.200239449971241434, -29.53745742343132719, 7.670465701733749420 ) ) ;
#35958 = CARTESIAN_POINT ( 'NONE',  ( 14.69492309387330664, -4.882291126226618871, 2.500000000000903277 ) ) ;
#35959 = CARTESIAN_POINT ( 'NONE',  ( -73.64256375807426025, -3.340549628714686303, -9.625460544246696060 ) ) ;
#35960 = CARTESIAN_POINT ( 'NONE',  ( 5.140791489254627145, -28.92678305073006939, 7.686927408461905031 ) ) ;
#35961 = LINE ( 'NONE', #28977, #35939 ) ;
#35962 = CARTESIAN_POINT ( 'NONE',  ( 78.76190985582825022, 66.07042273533500065, 1.483717294826051081 ) ) ;
#35963 = CARTESIAN_POINT ( 'NONE',  ( -1.524152690418147493, -30.64804141902853374, 7.778050822775631090 ) ) ;
#35964 = DIRECTION ( 'NONE',  ( -0.000000000000000000, -0.000000000000000000, -1.000000000000000000 ) ) ;
#35965 = DIRECTION ( 'NONE',  ( -1.000000000000000000, 0.000000000000000000, 0.000000000000000000 ) ) ;
#35966 = FACE_OUTER_BOUND ( 'NONE', #23276, .T. ) ;
#35967=STYLED_ITEM('',(#40745),#39670);
#35968 = AXIS2_PLACEMENT_3D ( 'NONE', #14579, #5338, #39705 ) ;
#35969 = B_SPLINE_CURVE_WITH_KNOTS ( 'NONE', 3,
 ( #4344, #29449, #1261, #20165, #13797, #10692, #34383, #21604, #31077, #2264, #15407, #37027, #11690, #2685, #5541, #18287, #20983, #18699, #24895, #9226, #21190, #27357, #27760, #37431, #33973, #18488, #5949, #2887, #39916, #12319, #2479, #12103, #11492, #24270, #27966, #33761, #21398, #18082, #15002, #27562, #5745, #17872, #40314, #24681, #11897 ),
 .UNSPECIFIED., .F., .F.,
 ( 4, 1, 2, 2, 1, 1, 1, 1, 1, 1, 1, 2, 2, 1, 1, 1, 1, 1, 1, 1, 1, 2, 2, 1, 1, 1, 1, 1, 1, 1, 1, 2, 2, 1, 4 ),
 ( 0.01538690458847954794, 0.1384635415149992888, 0.1423096864189528632, 0.1442327588709294284, 0.1461558313229059380, 0.1538481211308128094, 0.1692327007466265243, 0.2000018599782546203, 0.2307710192098827440, 0.2461555988256970695, 0.2480786712776741343, 0.2490402075036624030, 0.2500017437296506717, 0.2538478886336021367, 0.2615401784415042341, 0.3846168153679325186, 0.4461551338311469661, 0.4769242930627539123, 0.4923088726785574409, 0.4961550175825084064, 0.4980780900344842221, 0.4990396262604720468, 0.5000011624864599824, 0.5076934522943629124, 0.6307700892208103483, 0.6923084076840340106, 0.7230775669156456198, 0.7384621465314512578, 0.7461544363393539658, 0.7480775087913299481, 0.7490390450173182169, 0.7495198131303120181, 0.7500005812433059305, 0.7538467261472543424, 1.000000000000000000 ),
 .UNSPECIFIED. ) ;
#35970 = CIRCLE ( 'NONE', #17534, 0.1000000000000028644 ) ;
#35971 = CARTESIAN_POINT ( 'NONE',  ( -64.28431955412808918, 34.79066690201138812, 5.195917981389134965 ) ) ;
#35972 = CARTESIAN_POINT ( 'NONE',  ( 15.58401231752230842, 10.76254152672632536, -2.638660041548260615 ) ) ;
#35973 = CARTESIAN_POINT ( 'NONE',  ( 4.927871323695246275, -28.50060760253348491, 7.774064877406527074 ) ) ;
#35974 = CARTESIAN_POINT ( 'NONE',  ( 4.270010460102485972, -31.79637552378333964, 6.889465824494252821 ) ) ;
#35975 = CARTESIAN_POINT ( 'NONE',  ( 67.40765644887963504, 58.26613713413648554, 3.996173465816879489 ) ) ;
#35976 = EDGE_CURVE ( 'NONE', #23918, #12935, #21222, .T. ) ;
#35977 = VERTEX_POINT ( 'NONE', #27187 ) ;
#35978 = CARTESIAN_POINT ( 'NONE',  ( 88.68641656676298624, -1.259067802340008146, 0.2042187262504959744 ) ) ;
#35980 = CARTESIAN_POINT ( 'NONE',  ( -0.4140453450342095332, -26.78081456870760135, 7.009310105710483185 ) ) ;
#35979 = CARTESIAN_POINT ( 'NONE',  ( 81.02087009143656360, 62.46468763289096415, -3.155412080370040950 ) ) ;
#35981 = CARTESIAN_POINT ( 'NONE',  ( -1.287707616843211778, -27.74749443005756433, 6.865554069792297653 ) ) ;
#35982 = CARTESIAN_POINT ( 'NONE',  ( 2.399720784871332224, -26.14781977356483011, 7.776484688137385248 ) ) ;
#35983 = VERTEX_POINT ( 'NONE', #5573 ) ;
#35984 = CARTESIAN_POINT ( 'NONE',  ( 1.494999628127195779, -32.97077268039931397, 7.386948897581450346 ) ) ;
#35985 = CARTESIAN_POINT ( 'NONE',  ( -4.978675913592189417, -24.55319635012989110, 6.800000000000000711 ) ) ;
#35986 = ORIENTED_EDGE ( 'NONE', *, *, #21712, .T. ) ;
#35987 = CARTESIAN_POINT ( 'NONE',  ( -71.87291851043532631, -21.11138264414386612, 3.925186983125783513 ) ) ;
#35988 = EDGE_CURVE ( 'NONE', #33555, #22827, #20293, .T. ) ;
#35989 = ORIENTED_EDGE ( 'NONE', *, *, #24683, .T. ) ;
#35990 = CARTESIAN_POINT ( 'NONE',  ( 80.30571993285261101, 63.50758298881786601, -3.683925914261567236 ) ) ;
#35991 = PLANE ( 'NONE',  #20081 ) ;
#35992 = AXIS2_PLACEMENT_3D ( 'NONE', #13417, #22905, #885 ) ;
#35993 = CARTESIAN_POINT ( 'NONE',  ( 80.96353394671049841, 62.18107606247197339, 2.978180346930981770 ) ) ;
#35994 = CARTESIAN_POINT ( 'NONE',  ( 21.74229646505971658, 0.4512508753831538377, 8.537182636489522025 ) ) ;
#35996 = ORIENTED_EDGE ( 'NONE', *, *, #5387, .F. ) ;
#35995 = CARTESIAN_POINT ( 'NONE',  ( -0.7754396137877683781, -27.23962715764706033, 7.006423389747792108 ) ) ;
#35997 = AXIS2_PLACEMENT_3D ( 'NONE', #31454, #31658, #15800 ) ;
#35998 = CARTESIAN_POINT ( 'NONE',  ( 0.01152222936319628917, -32.52082164920695817, 7.756377446753164762 ) ) ;
#35999 = EDGE_CURVE ( 'NONE', #3093, #15456, #39745, .T. ) ;
#36000 = B_SPLINE_CURVE_WITH_KNOTS ( 'NONE', 3,
 ( #1956, #11780, #20865, #36715, #17967, #33457, #5226, #30348, #2154, #24361 ),
 .UNSPECIFIED., .F., .F.,
 ( 4, 3, 3, 4 ),
 ( 1.939479807224432123E-18, 3.025570593003208558E-05, 6.051145698344203796E-05, 6.468151674592953384E-05 ),
 .UNSPECIFIED. ) ;
#36002 = DIRECTION ( 'NONE',  ( -0.000000000000000000, -1.000000000000000000, -0.000000000000000000 ) ) ;
#36001 = CARTESIAN_POINT ( 'NONE',  ( 14.69558838330753758, 3.996311804371543985, 6.000000000000000000 ) ) ;
#36003 = CARTESIAN_POINT ( 'NONE',  ( -1.246815083620857134, -27.87462772991113980, 7.763628509615285722 ) ) ;
#36004 = CARTESIAN_POINT ( 'NONE',  ( -12.34874870218063947, -26.64985754041175525, 6.700000000000000178 ) ) ;
#36005 = CARTESIAN_POINT ( 'NONE',  ( 22.94357577811185323, 4.016617617340873636, -3.383606566543657213 ) ) ;
#36006 = ORIENTED_EDGE ( 'NONE', *, *, #38625, .F. ) ;
#36007 = DIRECTION ( 'NONE',  ( 1.000000000000000000, 6.938893903907229167E-15, 0.000000000000000000 ) ) ;
#36008 = CARTESIAN_POINT ( 'NONE',  ( 22.35506120569036170, 4.170988562608182626, 6.826273348963533216 ) ) ;
#36009 = CARTESIAN_POINT ( 'NONE',  ( 15.27436587416087121, 8.240068014946416497, 3.484044188646821638 ) ) ;
#36010 = ORIENTED_EDGE ( 'NONE', *, *, #2540, .T. ) ;
#36011 = CARTESIAN_POINT ( 'NONE',  ( 1.127397677933556830, -33.02270898565480906, 7.707984471951054850 ) ) ;
#36012 = CARTESIAN_POINT ( 'NONE',  ( 81.29907532208984833, 61.38588276545821998, 1.392093260605081317 ) ) ;
#36013 = CARTESIAN_POINT ( 'NONE',  ( 87.91375683397511409, -1.031045523906674033, -4.794500835981626352 ) ) ;
#36014 = CARTESIAN_POINT ( 'NONE',  ( -17.27251170661583402, -8.656638842136340273, 6.000000000000000000 ) ) ;
#36015 = ORIENTED_EDGE ( 'NONE', *, *, #297, .T. ) ;
#36017 = ADVANCED_FACE ( 'NONE', ( #18113 ), #1483, .T. ) ;
#36016 = VERTEX_POINT ( 'NONE', #24091 ) ;
#36018 = LINE ( 'NONE', #34120, #34236 ) ;
#36019 = AXIS2_PLACEMENT_3D ( 'NONE', #28875, #6849, #29077 ) ;
#36020 = ADVANCED_FACE ( 'NONE', ( #23502 ), #7846, .F. ) ;
#36021 = CARTESIAN_POINT ( 'NONE',  ( 33.96234278159153774, -3.201214304958433843, -5.507042992068187814 ) ) ;
#36022 = CARTESIAN_POINT ( 'NONE',  ( 34.77309710796683362, -3.158688717209038543, -5.633580812866661347 ) ) ;
#36023 = DIRECTION ( 'NONE',  ( -0.000000000000000000, 1.000000000000000000, -0.000000000000000000 ) ) ;
#36024 = CARTESIAN_POINT ( 'NONE',  ( 84.18174941840253211, 2.918289511092787780, 1.655912298728576815 ) ) ;
#36025 = PRODUCT_DEFINITION_FORMATION_WITH_SPECIFIED_SOURCE ( 'ANY', '', #8239, .NOT_KNOWN. ) ;
#36026 = CARTESIAN_POINT ( 'NONE',  ( 29.31288836536752029, -3.867418896606279688, -4.320839978493723699 ) ) ;
#36027 = VERTEX_POINT ( 'NONE', #29873 ) ;
#36028 = PLANE ( 'NONE',  #37484 ) ;
#36029 = DIRECTION ( 'NONE',  ( 1.000000000000000000, 0.000000000000000000, -0.000000000000000000 ) ) ;
#36030 = CARTESIAN_POINT ( 'NONE',  ( -1.196375916356071212, -27.78980578152105352, 6.866852738645442322 ) ) ;
#36031 = ORIENTED_EDGE ( 'NONE', *, *, #8685, .F. ) ;
#36032 = VERTEX_POINT ( 'NONE', #30084 ) ;
#36033 = CARTESIAN_POINT ( 'NONE',  ( 25.73396967306546657, 2.637378028382216577, 3.518935617133692961 ) ) ;
#36034 = CARTESIAN_POINT ( 'NONE',  ( -70.92837670882107659, -56.35932253828836025, 0.000000000000000000 ) ) ;
#36035 = EDGE_CURVE ( 'NONE', #4710, #14798, #20593, .T. ) ;
#36036 = EDGE_CURVE ( 'NONE', #23904, #8980, #13259, .T. ) ;
#36037 = CARTESIAN_POINT ( 'NONE',  ( 66.27376694609004915, 57.73522568913436004, -4.000000000000000000 ) ) ;
#36038 = CARTESIAN_POINT ( 'NONE',  ( 87.89153558153043377, -2.469980296156808475, 1.041252188155484149 ) ) ;
#36039 = ADVANCED_FACE ( 'NONE', ( #7486, #923 ), #35710, .F. ) ;
#36040 = ORIENTED_EDGE ( 'NONE', *, *, #20042, .T. ) ;
#36041 = CARTESIAN_POINT ( 'NONE',  ( 4.890701645444022638, -28.39438256639548896, 7.635761828346577573 ) ) ;
#36042 = CARTESIAN_POINT ( 'NONE',  ( -12.34874870218063947, -26.64985754041175525, 6.700000000000000178 ) ) ;
#36043 = VECTOR ( 'NONE', #2608, 1000.000000000000000 ) ;
#36044 = ORIENTED_EDGE ( 'NONE', *, *, #37080, .F. ) ;
#36045 = DIRECTION ( 'NONE',  ( 0.9848077530122080203, 0.1736481776669307198, -0.000000000000000000 ) ) ;
#36046 = CARTESIAN_POINT ( 'NONE',  ( 4.777618136733515541, -27.90236538453207515, 6.863805608295729499 ) ) ;
#36047 = ORIENTED_EDGE ( 'NONE', *, *, #17431, .F. ) ;
#36048 = CARTESIAN_POINT ( 'NONE',  ( 22.95533607554538946, 3.919416367836303206, 3.470897119079664250 ) ) ;
#36049 = CARTESIAN_POINT ( 'NONE',  ( 82.50803812506887880, 63.51743744066179431, -1.680016503630877178 ) ) ;
#36050 = VECTOR ( 'NONE', #32394, 1000.000000000000000 ) ;
#36051 = CARTESIAN_POINT ( 'NONE',  ( -1.225969928216009475, -31.30094636736736291, 7.692469944509197965 ) ) ;
#36052 = ORIENTED_EDGE ( 'NONE', *, *, #18670, .F. ) ;
#36054 = CARTESIAN_POINT ( 'NONE',  ( 22.13111492170271077, -2.652485278638713861, -3.660493745205452232 ) ) ;
#36053 = CARTESIAN_POINT ( 'NONE',  ( -4.547719893808338520E-15, -0.5999999999999994227, -3.779600343874077062 ) ) ;
#36055 = CARTESIAN_POINT ( 'NONE',  ( 4.416430171046111575, -31.62687967920297538, 7.139196562012270597 ) ) ;
#36056 = CARTESIAN_POINT ( 'NONE',  ( 74.52260502535293085, 62.13706486897681458, 3.724166978290282426 ) ) ;
#36057 = CARTESIAN_POINT ( 'NONE',  ( 24.01690006195003235, 2.804734595017727372, -3.921598103404013713 ) ) ;
#36058 = DIRECTION ( 'NONE',  ( -1.000000000000000000, 0.000000000000000000, 0.000000000000000000 ) ) ;
#36059 = AXIS2_PLACEMENT_3D ( 'NONE', #25434, #32238, #3442 ) ;
#36060 = CARTESIAN_POINT ( 'NONE',  ( -26.87867591359219333, -24.55319635012989110, 6.700000000000000178 ) ) ;
#36061 = CARTESIAN_POINT ( 'NONE',  ( 24.12827207576258104, 2.707173303308993528, -3.972198420524792439 ) ) ;
#36062 = CARTESIAN_POINT ( 'NONE',  ( -1.261893907174904905, -27.90113615618628273, 7.692469944509197965 ) ) ;
#36063 = FACE_OUTER_BOUND ( 'NONE', #2247, .T. ) ;
#36064 = CARTESIAN_POINT ( 'NONE',  ( 81.59006957456236364, 61.61658442860581175, 1.498428902123875028 ) ) ;
#36065 = B_SPLINE_CURVE_WITH_KNOTS ( 'NONE', 3,
 ( #9045, #12749, #3124, #31302, #12342, #25117, #22445, #31502, #22249, #34611, #21623, #18512, #2907, #27987, #24915, #15640, #38068, #35013, #419 ),
 .UNSPECIFIED., .F., .F.,
 ( 4, 3, 3, 3, 3, 3, 4 ),
 ( 9.697399036122160616E-19, 2.546128104244831518E-05, 5.711050680484053993E-05, 8.113074941675944753E-05, 0.0001053129305727060888, 0.0001360598016347089236, 0.0001612931755701964992 ),
 .UNSPECIFIED. ) ;
#36066 = CARTESIAN_POINT ( 'NONE',  ( 85.88453125851971492, 1.888142761377891832, -4.329341218647970280 ) ) ;
#36067 = CARTESIAN_POINT ( 'NONE',  ( 31.38399832331403161, -1.255798082282080008, 5.972680360385385079 ) ) ;
#36068 = CARTESIAN_POINT ( 'NONE',  ( 4.200390093233091093, -29.56993018339339940, 6.000000000000000000 ) ) ;
#36069 = LINE ( 'NONE', #8036, #535 ) ;
#36070 = CARTESIAN_POINT ( 'NONE',  ( -73.08996536204158190, 0.4269082215137926517, -10.93610844367175261 ) ) ;
#36071 = EDGE_CURVE ( 'NONE', #35752, #12705, #10905, .T. ) ;
#36072 = DIRECTION ( 'NONE',  ( -1.000000000000000000, 0.000000000000000000, 0.000000000000000000 ) ) ;
#36073 = CARTESIAN_POINT ( 'NONE',  ( 0.1091738275826929783, -26.45254908979351782, 6.998987538705438105 ) ) ;
#36074 = CARTESIAN_POINT ( 'NONE',  ( 20.66010564244338354, 4.228422099284120605, -3.378132346044065315 ) ) ;
#36075 = DIRECTION ( 'NONE',  ( 1.000000000000000000, 0.000000000000000000, -0.000000000000000000 ) ) ;
#36076 = CARTESIAN_POINT ( 'NONE',  ( -1.699609906766909040, -29.57443106709385816, 7.625529685907138422 ) ) ;
#36077 =( BOUNDED_CURVE ( )  B_SPLINE_CURVE ( 3, ( #11446, #24227, #8983, #5707 ),
 .UNSPECIFIED., .F., .T. ) 
 B_SPLINE_CURVE_WITH_KNOTS ( ( 4, 4 ),
 ( 4.748221474220559735, 4.941946782021394036 ),
 .UNSPECIFIED. ) 
 CURVE ( )  GEOMETRIC_REPRESENTATION_ITEM ( )  RATIONAL_B_SPLINE_CURVE ( ( 1.000000000000000000, 0.9968749865767494445, 0.9968749865767494445, 1.000000000000000000 ) ) 
 REPRESENTATION_ITEM ( '' )  );
#36078 = CIRCLE ( 'NONE', #13052, 6.138794830819693793 ) ;
#36079 = LINE ( 'NONE', #890, #24358 ) ;
#36080 = EDGE_CURVE ( 'NONE', #33085, #6054, #39633, .T. ) ;
#36081 = CARTESIAN_POINT ( 'NONE',  ( -2.500070672423774454, -28.79276407692314876, 7.695279973900954751 ) ) ;
#36082 = EDGE_CURVE ( 'NONE', #23016, #36632, #4213, .T. ) ;
#36083 = ORIENTED_EDGE ( 'NONE', *, *, #5387, .T. ) ;
#36084 = CARTESIAN_POINT ( 'NONE',  ( 23.13399157829620734, 3.188628281914902107, 3.769246907791176771 ) ) ;
#36085 = CARTESIAN_POINT ( 'NONE',  ( -6.978675913592191193, -24.55319635012989110, 6.700000000000000178 ) ) ;
#36086 = CARTESIAN_POINT ( 'NONE',  ( 67.06698855917106528, 57.83491659372258908, -3.993952884371010814 ) ) ;
#36087 = EDGE_CURVE ( 'NONE', #32959, #32120, #26042, .T. ) ;
#36088 = CIRCLE ( 'NONE', #18311, 3.000000000000002665 ) ;
#36089 = DIRECTION ( 'NONE',  ( -0.000000000000000000, -1.000000000000000000, -0.000000000000000000 ) ) ;
#36090 = ORIENTED_EDGE ( 'NONE', *, *, #17230, .F. ) ;
#36091 = DIRECTION ( 'NONE',  ( 0.000000000000000000, -0.7126435865141234061, -0.7015262779114458391 ) ) ;
#36092 = CARTESIAN_POINT ( 'NONE',  ( 86.18567091879171471, -0.09149539399120916461, -5.958500351614375745 ) ) ;
#36093 = CARTESIAN_POINT ( 'NONE',  ( 85.80843657999245977, 0.6132022408405360947, -5.953866110284497637 ) ) ;
#36094 = CARTESIAN_POINT ( 'NONE',  ( 2.319715055549975702, -32.91304797836431106, 7.661510568013096822 ) ) ;
#36095 = CARTESIAN_POINT ( 'NONE',  ( 0.4392850896841424269, -32.83485164247554877, 6.869132338375689706 ) ) ;
#36096 = CARTESIAN_POINT ( 'NONE',  ( -59.00110696496997775, 28.68040728033253473, 6.999999999999999112 ) ) ;
#36097 = VERTEX_POINT ( 'NONE', #23339 ) ;
#36098 = CARTESIAN_POINT ( 'NONE',  ( 24.38107346567219480, 3.152084082324316139, 3.324539938462093058 ) ) ;
#36099 = CARTESIAN_POINT ( 'NONE',  ( 81.47505553675507883, 61.46950381087523141, -1.000000000000000000 ) ) ;
#36100 = CARTESIAN_POINT ( 'NONE',  ( 79.87286157980665280, 64.75688458792350843, 3.459421039841300338 ) ) ;
#36101 = VECTOR ( 'NONE', #5426, 1000.000000000000000 ) ;
#36102 = DIRECTION ( 'NONE',  ( -0.8660254037844415942, 0.4999999999999950040, -0.000000000000000000 ) ) ;
#36103 = EDGE_LOOP ( 'NONE', ( #18616, #2852, #32496, #36090, #29349, #2610, #14376, #13841, #35604, #32445, #34484, #17518 ) ) ;
#36104 = CARTESIAN_POINT ( 'NONE',  ( 79.32401137462355223, 60.77278567581102209, -2.512892981323172847 ) ) ;
#36106 = CARTESIAN_POINT ( 'NONE',  ( -1.712868897180792382, -28.79555068392009431, 7.013024433893851217 ) ) ;
#36105 = CARTESIAN_POINT ( 'NONE',  ( 23.58291269724494654, 0.3979865196799417526, 5.534407531907699074 ) ) ;
#36107 = CARTESIAN_POINT ( 'NONE',  ( 81.29907532209045939, 61.38588276545838340, -1.392093260604376326 ) ) ;
#36108 = CARTESIAN_POINT ( 'NONE',  ( 78.30161670990426614, 64.30707665991987199, 3.470679136763274553 ) ) ;
#36109 = DIRECTION ( 'NONE',  ( -0.9999026450364576490, -0.01395351027862084224, 0.000000000000000000 ) ) ;
#36110 = CARTESIAN_POINT ( 'NONE',  ( 81.79239483946132339, 65.43557760269897017, 1.755995906647956240 ) ) ;
#36112 = ORIENTED_EDGE ( 'NONE', *, *, #40626, .F. ) ;
#36111 = DIRECTION ( 'NONE',  ( 1.000000000000000000, 0.000000000000000000, 0.000000000000000000 ) ) ;
#36113 = CARTESIAN_POINT ( 'NONE',  ( 27.46505532721044318, 0.1961140298417080874, 5.884446595982424810 ) ) ;
#36114 = CARTESIAN_POINT ( 'NONE',  ( -62.74554520265134272, 35.90271204080874412, -5.263896983009520802 ) ) ;
#36115 = ORIENTED_EDGE ( 'NONE', *, *, #16177, .F. ) ;
#36116 = CARTESIAN_POINT ( 'NONE',  ( 5.784498025276203492, -28.13289436698813972, 6.954324564059724878 ) ) ;
#36117 = CARTESIAN_POINT ( 'NONE',  ( 26.75173391963811298, 0.8966615678213633034, -4.382807213102920763 ) ) ;
#36118 = AXIS2_PLACEMENT_3D ( 'NONE', #31410, #28102, #40657 ) ;
#36119 = CARTESIAN_POINT ( 'NONE',  ( -12.97867591359219297, -24.55319635012989110, 6.700000000000000178 ) ) ;
#36120 = ORIENTED_EDGE ( 'NONE', *, *, #18644, .T. ) ;
#36121 = CARTESIAN_POINT ( 'NONE',  ( 36.87059600844250440, -2.088011045112093900, -5.864540870269784101 ) ) ;
#36122 = DIRECTION ( 'NONE',  ( 0.000000000000000000, 0.000000000000000000, 1.000000000000000000 ) ) ;
#36123 = CARTESIAN_POINT ( 'NONE',  ( -1.087582253741100846, -31.68587304350735323, 7.011627023500185629 ) ) ;
#36124 = LINE ( 'NONE', #7905, #23234 ) ;
#36125 = CARTESIAN_POINT ( 'NONE',  ( 2.707230893317792653, -32.81744307353336154, 6.876076431790004939 ) ) ;
#36126 = CARTESIAN_POINT ( 'NONE',  ( 2.324081863996483310, -32.91946213718349412, 7.257242401810565013 ) ) ;
#36127 = CARTESIAN_POINT ( 'NONE',  ( 1.885627875660562003, -26.07483424866503086, 6.989977667959444751 ) ) ;
#36128 = VECTOR ( 'NONE', #7974, 1000.000000000000000 ) ;
#36129 = ORIENTED_EDGE ( 'NONE', *, *, #14631, .F. ) ;
#36130 = CARTESIAN_POINT ( 'NONE',  ( 66.27376694608996388, 57.73522568913447373, 4.000000000000000000 ) ) ;
#36131 = CARTESIAN_POINT ( 'NONE',  ( 71.82805326594559858, 60.58951223549524201, -3.882941974849172695 ) ) ;
#36132 = EDGE_CURVE ( 'NONE', #8785, #17194, #26437, .T. ) ;
#36133 = EDGE_CURVE ( 'NONE', #6636, #34747, #16734, .T. ) ;
#36134 = VERTEX_POINT ( 'NONE', #29319 ) ;
#36135 = CARTESIAN_POINT ( 'NONE',  ( 85.07031394220433640, 1.982162274098862476, -4.809620659748507165 ) ) ;
#36136 = EDGE_CURVE ( 'NONE', #6925, #579, #19650, .T. ) ;
#36137 = CARTESIAN_POINT ( 'NONE',  ( 0.1827919725910926718, -26.52741295444542047, 6.979335674598004857 ) ) ;
#36138 = FACE_OUTER_BOUND ( 'NONE', #233, .T. ) ;
#36139 = CARTESIAN_POINT ( 'NONE',  ( -70.92837670882107659, -37.87473357531881391, 6.000000000000002665 ) ) ;
#36140 = LINE ( 'NONE', #20469, #33069 ) ;
#36141 = CYLINDRICAL_SURFACE ( 'NONE', #39120, 0.1000000000000028644 ) ;
#36142 = AXIS2_PLACEMENT_3D ( 'NONE', #31851, #25665, #22590 ) ;
#36143 = CARTESIAN_POINT ( 'NONE',  ( 5.053090684323510828, -30.13509655968624656, 7.652160403243382980 ) ) ;
#36144 = VERTEX_POINT ( 'NONE', #38363 ) ;
#36145 = CARTESIAN_POINT ( 'NONE',  ( 80.79830692519209379, 61.67796721187826847, -2.640205493567933992 ) ) ;
#36146 = CARTESIAN_POINT ( 'NONE',  ( 33.78549810770471851, -4.844043753022709176, 3.475806433684239583 ) ) ;
#36147 = CARTESIAN_POINT ( 'NONE',  ( 80.87649832867062116, 61.25867624111137388, 1.827177995460258941 ) ) ;
#36148 = ORIENTED_EDGE ( 'NONE', *, *, #40018, .T. ) ;
#36149 = B_SPLINE_CURVE_WITH_KNOTS ( 'NONE', 3,
 ( #9968, #27031, #20436, #14459, #21266, #36907, #5209, #1939, #14057, #1729, #2344, #27226, #8686, #36698, #5413, #17335, #30534, #11361, #26831, #17744, #33636, #23929, #33839, #8272, #29912, #7887, #8481 ),
 .UNSPECIFIED., .F., .F.,
 ( 4, 2, 2, 1, 1, 1, 1, 2, 2, 2, 1, 1, 1, 1, 1, 2, 2, 4 ),
 ( 0.000000000000000000, 0.08933253011160632862, 0.09003044050310334001, 0.09072835089460033753, 0.09212417167759436032, 0.09491581324358161487, 0.1004990963755560823, 0.1116656626395058499, 0.1339987951674053990, 0.1341732727652801827, 0.1343477503631549386, 0.1346967055589049223, 0.1353946159504048896, 0.1367904367334048243, 0.1395820782994046938, 0.1451653614314038776, 0.1563319276954028281, 0.1786650602234007013 ),
 .UNSPECIFIED. ) ;
#36150 = DIRECTION ( 'NONE',  ( 1.000000000000000000, 0.000000000000000000, -0.000000000000000000 ) ) ;
#36151 = AXIS2_PLACEMENT_3D ( 'NONE', #7641, #4565, #17092 ) ;
#36152 = CARTESIAN_POINT ( 'NONE',  ( 4.042482038083015539, -27.10525874040772365, 6.959317978105166169 ) ) ;
#36153 = CARTESIAN_POINT ( 'NONE',  ( 18.54920515881659782, 13.18659104987385433, 2.500000000000000000 ) ) ;
#36154 = CARTESIAN_POINT ( 'NONE',  ( 21.85643539959774984, 7.798985686765059100, -6.733359799098007414 ) ) ;
#36155 = ORIENTED_EDGE ( 'NONE', *, *, #20775, .F. ) ;
#36156 = DIRECTION ( 'NONE',  ( -0.000000000000000000, -0.000000000000000000, 1.000000000000000000 ) ) ;
#36157 = CARTESIAN_POINT ( 'NONE',  ( -61.24591834330252027, -23.80776546975053520, 2.500000000000000000 ) ) ;
#36158 = CARTESIAN_POINT ( 'NONE',  ( -72.46315804115566550, 6.112692013474589459, -9.882615271681798319 ) ) ;
#36159 = DIRECTION ( 'NONE',  ( 1.000000000000000000, 0.000000000000000000, 0.000000000000000000 ) ) ;
#36160 = CARTESIAN_POINT ( 'NONE',  ( 37.10495453580936953, -3.127303634092527762, -5.976092241509372016 ) ) ;
#36161 = CARTESIAN_POINT ( 'NONE',  ( 80.95462345035979013, 63.09697225074527438, 3.406228740995796311 ) ) ;
#36162 = CARTESIAN_POINT ( 'NONE',  ( 3.651251297819360531, -25.49307895267003587, 6.800000000000000711 ) ) ;
#36163 = CARTESIAN_POINT ( 'NONE',  ( 0.9940451555042898457, -25.35698173488204432, 7.695279973900954751 ) ) ;
#36164 = CYLINDRICAL_SURFACE ( 'NONE', #3717, 1.000000000000000444 ) ;
#36165 = CARTESIAN_POINT ( 'NONE',  ( 0.6407229928749871295, -26.23419853405188462, 6.875780273367531059 ) ) ;
#36166 = AXIS2_PLACEMENT_3D ( 'NONE', #20086, #32266, #16579 ) ;
#36167 = CARTESIAN_POINT ( 'NONE',  ( 3.977455998898224099, -32.22793147407356429, 7.700536657684220465 ) ) ;
#36168 = CARTESIAN_POINT ( 'NONE',  ( -70.92837670882107659, -36.87473357531881391, 0.000000000000000000 ) ) ;
#36169 = CARTESIAN_POINT ( 'NONE',  ( 4.169743078853456630, -31.90708568365600684, 6.988553391373226731 ) ) ;
#36170 = CARTESIAN_POINT ( 'NONE',  ( -69.42837670882107659, -47.11702805680359063, 5.809475019311128641 ) ) ;
#36171 = CARTESIAN_POINT ( 'NONE',  ( 67.78936902810559673, 58.13140593263176470, 3.993918888840294557 ) ) ;
#36172 = CARTESIAN_POINT ( 'NONE',  ( 2.288810108494835571, -33.01126522079324843, 7.778495531946296282 ) ) ;
#36173 = CARTESIAN_POINT ( 'NONE',  ( 85.09863483756090830, 2.770898922293168809, 1.806811963633389695 ) ) ;
#36174 = AXIS2_PLACEMENT_3D ( 'NONE', #18505, #6, #31292 ) ;
#36175 = ADVANCED_FACE ( 'NONE', ( #13458 ), #20753, .T. ) ;
#36177 = CARTESIAN_POINT ( 'NONE',  ( 33.33049225550245609, -1.121405412915873256, -5.408427436109264796 ) ) ;
#36176 = CARTESIAN_POINT ( 'NONE',  ( 80.13254067770888867, 64.54635310605580401, -3.552238747020024512 ) ) ;
#36178 = CARTESIAN_POINT ( 'NONE',  ( -1.605806591528507354, -28.77678541357339981, 6.979335674598005745 ) ) ;
#36179 = CARTESIAN_POINT ( 'NONE',  ( -58.75407610588014506, 29.59432899155028807, 5.651746018159727214 ) ) ;
#36180 = VERTEX_POINT ( 'NONE', #16343 ) ;
#36181 = CARTESIAN_POINT ( 'NONE',  ( -79.78869251280185892, 11.50862393811266138, -4.655148827077255191 ) ) ;
#36182 = CARTESIAN_POINT ( 'NONE',  ( 1.288977975861898662, -26.19490350224902642, 6.887945620086118659 ) ) ;
#36183 = ORIENTED_EDGE ( 'NONE', *, *, #13212, .T. ) ;
#36184 = FACE_OUTER_BOUND ( 'NONE', #17449, .T. ) ;
#36185 = CARTESIAN_POINT ( 'NONE',  ( 81.09055442218975429, 61.42501475223627949, -1.950029235564217478 ) ) ;
#36186 = CARTESIAN_POINT ( 'NONE',  ( 24.93765456293620275, 3.473447388903421196, 1.305885461667957825 ) ) ;
#36187 = CARTESIAN_POINT ( 'NONE',  ( 80.93548213101078659, 62.17232332437959030, 2.988136994358705056 ) ) ;
#36188 = CARTESIAN_POINT ( 'NONE',  ( 22.50932894906165060, 0.7908534467655897737, 6.383121493648327593 ) ) ;
#36190 = ORIENTED_EDGE ( 'NONE', *, *, #10132, .F. ) ;
#36189 = CARTESIAN_POINT ( 'NONE',  ( 4.731075428271440231, -27.83036318828329669, 7.773839561854632763 ) ) ;
#36191 = CARTESIAN_POINT ( 'NONE',  ( 3.229898424385141187, -32.60648237212752321, 7.006423389747791219 ) ) ;
#36193 = DIRECTION ( 'NONE',  ( 0.000000000000000000, 0.6605219282605402364, -0.7508067542896625923 ) ) ;
#36192 = CARTESIAN_POINT ( 'NONE',  ( 0.000000000000000000, 0.000000000000000000, -3.961287410364449979 ) ) ;
#36194 = DIRECTION ( 'NONE',  ( -0.7660444431189770143, 0.6427876096865404731, 0.000000000000000000 ) ) ;
#36195 = DIRECTION ( 'NONE',  ( -0.3420201433256663259, 0.9396926207859092051, 0.000000000000000000 ) ) ;
#36196 = ADVANCED_FACE ( 'NONE', ( #26032 ), #35909, .F. ) ;
#36197 = CARTESIAN_POINT ( 'NONE',  ( 23.19158755795082882, 3.577708210753886675, -3.605410824286771732 ) ) ;
#36198 = EDGE_LOOP ( 'NONE', ( #4362, #30570, #34967, #12227 ) ) ;
#36199 = DIRECTION ( 'NONE',  ( -0.000000000000000000, -0.000000000000000000, -1.000000000000000000 ) ) ;
#36200 = VERTEX_POINT ( 'NONE', #22948 ) ;
#36201 = CARTESIAN_POINT ( 'NONE',  ( 22.45979449916501736, 0.3571986981647585768, -9.138524188866155029 ) ) ;
#36202 = DIRECTION ( 'NONE',  ( -0.5991095979999732091, 0.2428960078352054019, 0.7629346098860835257 ) ) ;
#36203 = LINE ( 'NONE', #7982, #26149 ) ;
#36204 = CARTESIAN_POINT ( 'NONE',  ( 81.56787793378551044, 61.92707632880442503, 2.226826180281122447 ) ) ;
#36205 = CARTESIAN_POINT ( 'NONE',  ( 86.75210013534866960, -0.2795847087395720298, -5.842668109216860195 ) ) ;
#36206 = DIRECTION ( 'NONE',  ( 1.000000000000000000, -0.000000000000000000, 0.000000000000000000 ) ) ;
#36207 = EDGE_LOOP ( 'NONE', ( #34193, #27097, #746, #15460 ) ) ;
#36208 = CARTESIAN_POINT ( 'NONE',  ( -1.425774885472621767, -28.23310838303483550, 7.013842709614101167 ) ) ;
#36209 = EDGE_CURVE ( 'NONE', #7270, #34797, #13668, .T. ) ;
#36210 = CARTESIAN_POINT ( 'NONE',  ( 4.733915118986097958, -28.03444136281207832, 7.013842709614101167 ) ) ;
#36211 = CARTESIAN_POINT ( 'NONE',  ( 18.24203027604363214, -3.069080384045527410, -3.024498425576051197 ) ) ;
#36212 = CARTESIAN_POINT ( 'NONE',  ( 29.10051722050815215, 0.3561458739526577322, -4.748237529565580317 ) ) ;
#36213 = DIRECTION ( 'NONE',  ( 0.000000000000000000, 0.000000000000000000, 1.000000000000000000 ) ) ;
#36214 = CARTESIAN_POINT ( 'NONE',  ( 24.11505776774735921, 0.5870443042865580718, -5.089557059125589866 ) ) ;
#36215 = CARTESIAN_POINT ( 'NONE',  ( 1.700390093233090871, -29.56993018339339940, 7.750000000000000888 ) ) ;
#36216 = EDGE_LOOP ( 'NONE', ( #30950, #34369, #21258, #36015, #26117, #37950, #28564 ) ) ;
#36217 = CARTESIAN_POINT ( 'NONE',  ( 2.792826902421812196, -32.89234763507269577, 7.766640943994341129 ) ) ;
#36218 = VECTOR ( 'NONE', #5851, 1000.000000000000000 ) ;
#36219 = LINE ( 'NONE', #10289, #34289 ) ;
#36220 = CARTESIAN_POINT ( 'NONE',  ( -1.135147046452389397, -27.69383203199361532, 6.979335674598006634 ) ) ;
#36221 = EDGE_CURVE ( 'NONE', #26557, #30200, #29521, .T. ) ;
#36222 = ORIENTED_EDGE ( 'NONE', *, *, #23382, .T. ) ;
#36223 = ORIENTED_EDGE ( 'NONE', *, *, #2622, .T. ) ;
#36224 = CARTESIAN_POINT ( 'NONE',  ( 30.88296028701921259, 0.6986673433299844804, 4.492958028923911940 ) ) ;
#36225 = AXIS2_PLACEMENT_3D ( 'NONE', #19556, #38072, #31506 ) ;
#36226 = CARTESIAN_POINT ( 'NONE',  ( -1.646367189487829119, -30.59424959516734432, 6.912143950357346078 ) ) ;
#36227 = CARTESIAN_POINT ( 'NONE',  ( 3.411265863501067308, -26.50879084905291450, 7.255881584735163869 ) ) ;
#36228 = CARTESIAN_POINT ( 'NONE',  ( 86.31054848189137374, -0.3087909235149370879, 5.883766619840620216 ) ) ;
#36229 = ORIENTED_EDGE ( 'NONE', *, *, #23255, .F. ) ;
#36230 = B_SPLINE_CURVE_WITH_KNOTS ( 'NONE', 3,
 ( #20389, #14416, #1893, #17093, #1286, #29666, #17290, #13823, #14608, #11519, #26984, #39530, #24086, #23496 ),
 .UNSPECIFIED., .F., .F.,
 ( 4, 2, 2, 2, 2, 2, 4 ),
 ( 0.000000000000000000, 0.0007708628662404179172, 0.001156294299360619612, 0.001541725732480821306, 0.001927157165601023001, 0.002312588598721224912, 0.003083451464961651720 ),
 .UNSPECIFIED. ) ;
#36231 = VERTEX_POINT ( 'NONE', #13059 ) ;
#36232 = VECTOR ( 'NONE', #24983, 1000.000000000000000 ) ;
#36233 = CARTESIAN_POINT ( 'NONE',  ( -12.87867591359218977, -26.64985754041175525, 6.700000000000000178 ) ) ;
#36234 = CARTESIAN_POINT ( 'NONE',  ( -57.73493806181993904, 28.75062263012298303, -2.538950603207570378 ) ) ;
#36235 = ORIENTED_EDGE ( 'NONE', *, *, #17399, .T. ) ;
#36237 = CARTESIAN_POINT ( 'NONE',  ( 4.318115897878434417, -27.40022832085480786, 7.779495906702013741 ) ) ;
#36236 = FACE_OUTER_BOUND ( 'NONE', #35300, .T. ) ;
#36238 = VERTEX_POINT ( 'NONE', #25621 ) ;
#36239 = CARTESIAN_POINT ( 'NONE',  ( 22.06452787639179647, 5.259082593475454814, 3.268497644756389597 ) ) ;
#36240 = CARTESIAN_POINT ( 'NONE',  ( 82.21693166776705652, 64.09145645796273527, -2.325514254129002367 ) ) ;
#36241 = EDGE_CURVE ( 'NONE', #24175, #22597, #36149, .T. ) ;
#36242 = DIRECTION ( 'NONE',  ( 0.000000000000000000, 0.000000000000000000, -1.000000000000000000 ) ) ;
#36243 = ORIENTED_EDGE ( 'NONE', *, *, #29614, .T. ) ;
#36245 = CARTESIAN_POINT ( 'NONE',  ( 26.13518495524960983, -2.760235698259291492, -4.285425712740152271 ) ) ;
#36244 = DIRECTION ( 'NONE',  ( -0.000000000000000000, -0.000000000000000000, 1.000000000000000000 ) ) ;
#36246 = DIRECTION ( 'NONE',  ( -1.000000000000000000, 0.000000000000000000, 0.000000000000000000 ) ) ;
#36247 = CARTESIAN_POINT ( 'NONE',  ( 74.79578028543750179, 61.54621940999656715, 3.896954863271602232 ) ) ;
#36248 = ORIENTED_EDGE ( 'NONE', *, *, #24547, .F. ) ;
#36249 = CARTESIAN_POINT ( 'NONE',  ( 24.49589214427983208, 2.769561699705143099, -3.859156718590324164 ) ) ;
#36250 = CYLINDRICAL_SURFACE ( 'NONE', #29357, 3.399999999999999911 ) ;
#36251 = LINE ( 'NONE', #23290, #1762 ) ;
#36252 = CARTESIAN_POINT ( 'NONE',  ( -1.432293644835494373, -27.47664038617742577, 4.000000000000000000 ) ) ;
#36253 = FACE_OUTER_BOUND ( 'NONE', #35064, .T. ) ;
#36254 = CARTESIAN_POINT ( 'NONE',  ( 1.677877769585896628, -26.06999691478939241, 7.646866513072557048 ) ) ;
#36255 = CARTESIAN_POINT ( 'NONE',  ( 81.70897365440946203, 61.83459377731555406, 1.744953761006670989 ) ) ;
#36256 = CARTESIAN_POINT ( 'NONE',  ( 87.93559242015480493, -0.4157064846058496355, 3.292354338654781998 ) ) ;
#36257 = CARTESIAN_POINT ( 'NONE',  ( 30.65010716405877034, -0.4808061152566996399, -5.754690052858093097 ) ) ;
#36258 = EDGE_CURVE ( 'NONE', #17469, #33252, #28794, .T. ) ;
#36259 = ADVANCED_FACE ( 'NONE', ( #23731 ), #36301, .F. ) ;
#36260 = CARTESIAN_POINT ( 'NONE',  ( 3.472143277054946076, -26.66805309164448801, 6.870716933885665512 ) ) ;
#36261 = EDGE_CURVE ( 'NONE', #30067, #1864, #8075, .T. ) ;
#36262 = CARTESIAN_POINT ( 'NONE',  ( -81.80090188080514224, -5.603160304130404334, -0.6545554231109831367 ) ) ;
#36263 = CARTESIAN_POINT ( 'NONE',  ( 0.5908764294676954743, -26.35605721920861555, 6.887041543973314361 ) ) ;
#36264 = DIRECTION ( 'NONE',  ( 1.000000000000000000, 0.000000000000000000, 0.000000000000000000 ) ) ;
#36265 = AXIS2_PLACEMENT_3D ( 'NONE', #26956, #11692, #5340 ) ;
#36266 = CARTESIAN_POINT ( 'NONE',  ( 33.68680382786263294, -1.062740808955847660, -5.464038474404074641 ) ) ;
#36267 = CYLINDRICAL_SURFACE ( 'NONE', #31916, 0.09010775117052929883 ) ;
#36268 = LINE ( 'NONE', #8044, #39056 ) ;
#36269 = CARTESIAN_POINT ( 'NONE',  ( 11.29080664838498649, 1.564594260697056104E-15, 6.000000000000000000 ) ) ;
#36270 = DIRECTION ( 'NONE',  ( 0.000000000000000000, 1.000000000000000000, 0.000000000000000000 ) ) ;
#36271 = EDGE_CURVE ( 'NONE', #27940, #25461, #33018, .T. ) ;
#36272 = VERTEX_POINT ( 'NONE', #5006 ) ;
#36273 = CARTESIAN_POINT ( 'NONE',  ( 36.86636322194920723, -3.288495969527875040, 5.928692945992483310 ) ) ;
#36274 = B_SPLINE_CURVE_WITH_KNOTS ( 'NONE', 3,
 ( #22366, #3444, #26256, #10585, #38181, #13688, #15960, #28522, #35334, #38582, #4228, #35128, #6906, #29335, #23157, #25843, #10179, #19462, #332, #26051, #38790, #1154, #19257, #12872, #37981, #22768, #32432, #25436, #9984, #7103, #34931 ),
 .UNSPECIFIED., .F., .F.,
 ( 4, 3, 3, 3, 3, 3, 3, 3, 3, 3, 4 ),
 ( 4.336808689942017736E-18, 3.077658087705547918E-05, 6.152638666998892195E-05, 9.267501192706379103E-05, 0.0001241882240135189545, 0.0001556618703051619482, 0.0001866161554452189968, 0.0002167966385860955179, 0.0002463805737537769474, 0.0002758761370306513517, 0.0002847094172290125843 ),
 .UNSPECIFIED. ) ;
#36275 = CARTESIAN_POINT ( 'NONE',  ( 1.217126534916886937, -26.10345411493373291, 7.750000000000000888 ) ) ;
#36276 = CARTESIAN_POINT ( 'NONE',  ( 67.66003928550829016, 58.48093499090138891, -3.988165415173012374 ) ) ;
#36277 = DIRECTION ( 'NONE',  ( 0.000000000000000000, 1.000000000000000000, 0.000000000000000000 ) ) ;
#36278 = ORIENTED_EDGE ( 'NONE', *, *, #22662, .F. ) ;
#36279 = FACE_OUTER_BOUND ( 'NONE', #21827, .T. ) ;
#36280 = CARTESIAN_POINT ( 'NONE',  ( 3.802248482306934463, -32.24242835236076843, 7.768425012602589774 ) ) ;
#36281 = CARTESIAN_POINT ( 'NONE',  ( 84.89441094598296900, 2.017138685944319221, -4.674259599216689764 ) ) ;
#36282 = CARTESIAN_POINT ( 'NONE',  ( -80.15742618671445996, 11.51087320173220263, 3.873033802042450180 ) ) ;
#36283 = LINE ( 'NONE', #8058, #2390 ) ;
#36284 = CARTESIAN_POINT ( 'NONE',  ( 1.281736550542457831, -26.09505782811984176, 6.971170733404104425 ) ) ;
#36285 = ORIENTED_EDGE ( 'NONE', *, *, #18826, .F. ) ;
#36286 = CARTESIAN_POINT ( 'NONE',  ( 22.38435940742265373, 4.925671751812593868, 3.061725572434287557 ) ) ;
#36287 = CARTESIAN_POINT ( 'NONE',  ( 79.68852728668518637, 66.33522678087791746, -1.000000000000000000 ) ) ;
#36288 = CARTESIAN_POINT ( 'NONE',  ( 81.17684021745370160, 61.76890268566523901, 2.450942308261411018 ) ) ;
#36289 = VECTOR ( 'NONE', #3927, 1000.000000000000000 ) ;
#36290 = CARTESIAN_POINT ( 'NONE',  ( -0.03790328338398483987, -32.60774784362404688, 7.635761828346575797 ) ) ;
#36291 = VERTEX_POINT ( 'NONE', #30125 ) ;
#36292 = CARTESIAN_POINT ( 'NONE',  ( 78.15185181088403965, 63.91595853815784523, -3.616565173810658784 ) ) ;
#36294 = CARTESIAN_POINT ( 'NONE',  ( 14.77487148941764694, -5.166432627237171893, -2.500000000170817138 ) ) ;
#36293 = CARTESIAN_POINT ( 'NONE',  ( 27.44318431746329878, 0.9300348501808439750, 4.489570647297722594 ) ) ;
#36295 = CARTESIAN_POINT ( 'NONE',  ( 81.16204935228429918, 61.30122352005675168, -1.083735637652199602 ) ) ;
#36296 = LINE ( 'NONE', #20632, #13691 ) ;
#36297 = CARTESIAN_POINT ( 'NONE',  ( 79.81867444595899030, 61.24600406626226601, 2.764360460937574260 ) ) ;
#36298 = EDGE_LOOP ( 'NONE', ( #13602, #27805, #22554, #23683, #21457, #22076, #3463, #22629, #29649, #31735, #37393, #6422 ) ) ;
#36299 = EDGE_LOOP ( 'NONE', ( #9813, #31904, #25514, #24231 ) ) ;
#36300 = EDGE_CURVE ( 'NONE', #18734, #33979, #3726, .T. ) ;
#36301 = PLANE ( 'NONE',  #27993 ) ;
#36302 = EDGE_CURVE ( 'NONE', #37237, #22023, #25167, .T. ) ;
#36303 = CARTESIAN_POINT ( 'NONE',  ( 82.53887461166632988, 63.53329618120201161, 1.555014038482367633 ) ) ;
#36304 =( BOUNDED_SURFACE ( )  B_SPLINE_SURFACE ( 3, 3, ( 
 ( #30215, #23236, #17234, #20735 ),
 ( #26524, #14548, #8166, #29806 ),
 ( #7779, #17635, #17031, #23816 ),
 ( #36001, #35805, #20134, #8374 ),
 ( #29606, #7580, #17841, #20327 ),
 ( #5102, #32715, #27322, #2032 ),
 ( #32909, #36392, #20948, #27122 ) ),
 .UNSPECIFIED., .T., .F., .T. ) 
 B_SPLINE_SURFACE_WITH_KNOTS ( ( 4, 3, 4 ),
 ( 4, 4 ),
 ( 0.000000000000000000, 0.5000000000000000000, 1.000000000000000000 ),
 ( 0.000000000000000000, 1.000000000000000000 ),
 .UNSPECIFIED. ) 
 GEOMETRIC_REPRESENTATION_ITEM ( )  RATIONAL_B_SPLINE_SURFACE ( (
 ( 1.000000000000000000, 0.9563893749471424899, 0.9563893749471424899, 1.000000000000000000),
 ( 0.3333333333333333703, 0.3187964583157141818, 0.3187964583157141818, 0.3333333333333333703),
 ( 0.3333333333333333703, 0.3187964583157141818, 0.3187964583157141818, 0.3333333333333333703),
 ( 1.000000000000000000, 0.9563893749471424899, 0.9563893749471424899, 1.000000000000000000),
 ( 0.3333333333333333703, 0.3187964583157141818, 0.3187964583157141818, 0.3333333333333333703),
 ( 0.3333333333333333703, 0.3187964583157141818, 0.3187964583157141818, 0.3333333333333333703),
 ( 1.000000000000000000, 0.9563893749471424899, 0.9563893749471424899, 1.000000000000000000) ) ) 
 REPRESENTATION_ITEM ( '' )  SURFACE ( )  );
#36306 = DIRECTION ( 'NONE',  ( -0.000000000000000000, -0.000000000000000000, 1.000000000000000000 ) ) ;
#36305 = CARTESIAN_POINT ( 'NONE',  ( 3.426543769787936622, -26.64069931422037030, 7.782167645815906809 ) ) ;
#36307 = CARTESIAN_POINT ( 'NONE',  ( 27.31903677934867147, 0.4900422023718347675, -5.740875207198388175 ) ) ;
#36308 = DIRECTION ( 'NONE',  ( 1.000000000000000000, 0.000000000000000000, -0.000000000000000000 ) ) ;
#36309 = ORIENTED_EDGE ( 'NONE', *, *, #9779, .T. ) ;
#36310 = CARTESIAN_POINT ( 'NONE',  ( -80.68111603624291206, -5.697143737140332398, 2.247291075986532771 ) ) ;
#36311 = CARTESIAN_POINT ( 'NONE',  ( 26.76128115921286721, 0.8698978912984448586, -4.383280502865230410 ) ) ;
#36312 = ADVANCED_FACE ( 'NONE', ( #28456 ), #37506, .T. ) ;
#36313 = CARTESIAN_POINT ( 'NONE',  ( -2.718383313029612225, -27.92336371131444750, 7.695279973900954751 ) ) ;
#36314 = PLANE ( 'NONE',  #11224 ) ;
#36315 = CARTESIAN_POINT ( 'NONE',  ( 5.174553870628630037, -29.14543674784208704, 6.989977667959446528 ) ) ;
#36316 = CARTESIAN_POINT ( 'NONE',  ( -71.19099899316580604, 0.1905038897469244485, 3.995461420880249470 ) ) ;
#36317 = CARTESIAN_POINT ( 'NONE',  ( 33.94448162299985938, -0.4909416048696789159, -5.125106431712468158 ) ) ;
#36318 = CARTESIAN_POINT ( 'NONE',  ( 0.2000000000000000111, 0.000000000000000000, 0.000000000000000000 ) ) ;
#36319 = LINE ( 'NONE', #20062, #23563 ) ;
#36320 = CARTESIAN_POINT ( 'NONE',  ( -1.040518353328913959, -31.74651596798171127, 6.863805608295729499 ) ) ;
#36321 = CARTESIAN_POINT ( 'NONE',  ( 4.993907954365692348, -30.75430347691218813, 7.635761828346578461 ) ) ;
#36322 = CARTESIAN_POINT ( 'NONE',  ( 2.666995777737314111, -32.82963468697713694, 6.929923840112063083 ) ) ;
#36323 = CARTESIAN_POINT ( 'NONE',  ( 11.65737507970504439, -29.56993018339339940, 6.800000000000000711 ) ) ;
#36324 = CARTESIAN_POINT ( 'NONE',  ( 1.892518328694925422, -26.07520748464628468, 6.951256099901589991 ) ) ;
#36325 = ORIENTED_EDGE ( 'NONE', *, *, #9059, .F. ) ;
#36326 = EDGE_CURVE ( 'NONE', #29204, #7215, #37218, .T. ) ;
#36327 = CARTESIAN_POINT ( 'NONE',  ( 66.27376694608996388, 57.73522568913447373, 4.000000000000000000 ) ) ;
#36328 = CARTESIAN_POINT ( 'NONE',  ( 73.78163614357571021, 59.18917187859454998, -3.552420216828422461 ) ) ;
#36329 = AXIS2_PLACEMENT_3D ( 'NONE', #25811, #512, #10551 ) ;
#36330 = ORIENTED_EDGE ( 'NONE', *, *, #16410, .T. ) ;
#36331 = CARTESIAN_POINT ( 'NONE',  ( 85.00114435706898064, 2.071954908684588759, 4.651167869591634307 ) ) ;
#36332 = CARTESIAN_POINT ( 'NONE',  ( -60.66839582778040807, 24.84364830758653397, 8.800414904976364028 ) ) ;
#36333 = CARTESIAN_POINT ( 'NONE',  ( 2.923652617287828992, -26.39759808583085388, 6.880147297696980857 ) ) ;
#36334 = B_SPLINE_CURVE_WITH_KNOTS ( 'NONE', 3,
 ( #7922, #14296, #20677, #35551, #17178, #4249, #20079, #20471, #963, #35745 ),
 .UNSPECIFIED., .F., .F.,
 ( 4, 3, 3, 4 ),
 ( 8.673617379884034509E-19, 3.025505781527745516E-05, 6.051003801291361255E-05, 6.468145402690660616E-05 ),
 .UNSPECIFIED. ) ;
#36335 = ORIENTED_EDGE ( 'NONE', *, *, #18727, .F. ) ;
#36336 = DIRECTION ( 'NONE',  ( -0.000000000000000000, 1.000000000000000000, -0.000000000000000000 ) ) ;
#36337 = CYLINDRICAL_SURFACE ( 'NONE', #27116, 2.500000000000002220 ) ;
#36338 = CARTESIAN_POINT ( 'NONE',  ( 33.89725028478159174, -5.465908938576614418, 0.4877600842561391481 ) ) ;
#36339 = DIRECTION ( 'NONE',  ( 1.000000000000000000, 0.000000000000000000, 0.000000000000000000 ) ) ;
#36340 = EDGE_CURVE ( 'NONE', #39584, #14639, #14518, .T. ) ;
#36341 = ORIENTED_EDGE ( 'NONE', *, *, #7615, .T. ) ;
#36342 = ORIENTED_EDGE ( 'NONE', *, *, #34615, .F. ) ;
#36343 = CARTESIAN_POINT ( 'NONE',  ( 78.88927015299483969, 65.04551736973371590, -3.140153738741058298 ) ) ;
#36344 = CARTESIAN_POINT ( 'NONE',  ( 17.62552264067466012, 11.92971595993793699, -2.499999999999990230 ) ) ;
#36345 = CARTESIAN_POINT ( 'NONE',  ( 79.40660192983034449, 64.44177602733365973, 3.564905221331805762 ) ) ;
#36347 = EDGE_LOOP ( 'NONE', ( #17147, #10165, #2502, #26416, #21863 ) ) ;
#36346 = CARTESIAN_POINT ( 'NONE',  ( -70.92837670882107659, 28.72470171467712063, 4.406751979251624540 ) ) ;
#36348 = DIRECTION ( 'NONE',  ( 1.000000000000000000, 0.000000000000000000, 0.000000000000000000 ) ) ;
#36349 = EDGE_CURVE ( 'NONE', #13245, #36422, #31352, .T. ) ;
#36350 = CARTESIAN_POINT ( 'NONE',  ( 4.002494580657026901, -27.06784897793791700, 6.871394612369936539 ) ) ;
#36351 = DIRECTION ( 'NONE',  ( 0.9396926207859135349, -0.3420201433256548351, 0.000000000000000000 ) ) ;
#36352 = CARTESIAN_POINT ( 'NONE',  ( 21.85643539959774273, 10.54442680926682208, -0.8960936389291185300 ) ) ;
#36353 = VERTEX_POINT ( 'NONE', #37699 ) ;
#36354 = CARTESIAN_POINT ( 'NONE',  ( -80.70058103876492339, 10.56056044066735389, 2.265492480125265828 ) ) ;
#36355 = VECTOR ( 'NONE', #39104, 1000.000000000000000 ) ;
#36356 = EDGE_CURVE ( 'NONE', #20068, #9480, #21680, .T. ) ;
#36357 = CARTESIAN_POINT ( 'NONE',  ( 14.72816174088550412, -4.874090160042384490, 2.502238201714006571 ) ) ;
#36358 = EDGE_CURVE ( 'NONE', #32142, #33506, #14839, .T. ) ;
#36359 = CARTESIAN_POINT ( 'NONE',  ( -79.68352313332665915, 11.50554291592259304, -4.849210015756803216 ) ) ;
#36360 = CARTESIAN_POINT ( 'NONE',  ( 1.491082739486949471, -32.96348259045947060, 6.939395833800441338 ) ) ;
#36361 = CARTESIAN_POINT ( 'NONE',  ( 2.485966948262496867, -26.26192714095899561, 6.997764925645182821 ) ) ;
#36362 = CARTESIAN_POINT ( 'NONE',  ( 80.94524665917968775, 63.44345826879091277, 3.487490852634240301 ) ) ;
#36363 = CARTESIAN_POINT ( 'NONE',  ( -1.504793647276889246, -30.70430101763167841, 7.782167645815905033 ) ) ;
#36364 = DIRECTION ( 'NONE',  ( 1.000000000000000000, 0.000000000000000000, 0.000000000000000000 ) ) ;
#36365 = CARTESIAN_POINT ( 'NONE',  ( 0.6760706814591578295, -26.22317290067247342, 6.912143950357346078 ) ) ;
#36366 = CARTESIAN_POINT ( 'NONE',  ( 4.411012430042179133, -27.35574694287801378, 6.880608371227947551 ) ) ;
#36367 = CARTESIAN_POINT ( 'NONE',  ( 87.84483433992669177, -0.3137627012552636763, 3.545048087552764571 ) ) ;
#36368 = CARTESIAN_POINT ( 'NONE',  ( 4.180051228910634187, -31.89615321790286018, 6.895222827070024429 ) ) ;
#36369 = CARTESIAN_POINT ( 'NONE',  ( 67.92345958529671179, 58.66354838738842403, 3.978477839347868361 ) ) ;
#36370 = CARTESIAN_POINT ( 'NONE',  ( 37.04660275223199761, -2.800648277598226876, 5.988416353595834352 ) ) ;
#36371 = VERTEX_POINT ( 'NONE', #9508 ) ;
#36372 = CARTESIAN_POINT ( 'NONE',  ( 3.976596914110534620, -33.75953324440050096, 6.954324564059724878 ) ) ;
#36373 = CARTESIAN_POINT ( 'NONE',  ( 86.79297523138272652, 0.7501027249346864378, -5.742269118526623473 ) ) ;
#36375 = CARTESIAN_POINT ( 'NONE',  ( -62.86576508122317364, 38.67912974266874926, 7.000000000000000000 ) ) ;
#36374 = CARTESIAN_POINT ( 'NONE',  ( 79.72815809223409644, 65.03555043453916085, -3.332694751021849200 ) ) ;
#36376 = CARTESIAN_POINT ( 'NONE',  ( 0.1649012726517564975, -26.53640515764040231, 7.013842709614101167 ) ) ;
#36377 = DIRECTION ( 'NONE',  ( -0.000000000000000000, -0.000000000000000000, -1.000000000000000000 ) ) ;
#36378 = VECTOR ( 'NONE', #19785, 1000.000000000000114 ) ;
#36379 = CARTESIAN_POINT ( 'NONE',  ( -59.61240458878657478, 26.78407864000505612, 6.268956829791734187 ) ) ;
#36380 = DIRECTION ( 'NONE',  ( 1.000000000000000000, 0.000000000000000000, 0.000000000000000000 ) ) ;
#36381 = EDGE_LOOP ( 'NONE', ( #11106, #34565, #25497, #27766 ) ) ;
#36382 = CARTESIAN_POINT ( 'NONE',  ( -71.92837670882107659, -20.89404664731295114, 5.928123921495630277 ) ) ;
#36383 = CARTESIAN_POINT ( 'NONE',  ( 80.77881921633029094, 62.12902493665696824, -3.041370705153006782 ) ) ;
#36384 = CARTESIAN_POINT ( 'NONE',  ( -1.679395455362387102, -29.14213866777389228, 7.134148492716103185 ) ) ;
#36385 = CARTESIAN_POINT ( 'NONE',  ( 80.57397677244617284, 62.93365480201040896, 3.508091314521097903 ) ) ;
#36386 = CARTESIAN_POINT ( 'NONE',  ( 21.76373982720479461, 0.8608337276742248356, 7.726924402482800325 ) ) ;
#36388 = ORIENTED_EDGE ( 'NONE', *, *, #7349, .F. ) ;
#36387 = CARTESIAN_POINT ( 'NONE',  ( -0.7953160622768807864, -27.26092192145711124, 6.876076431790005827 ) ) ;
#36389 = VECTOR ( 'NONE', #31826, 1000.000000000000000 ) ;
#36390 = CARTESIAN_POINT ( 'NONE',  ( 75.14412900705532650, 60.78131343986104440, -3.865308561588337799 ) ) ;
#36391 = FACE_OUTER_BOUND ( 'NONE', #14899, .T. ) ;
#36393 = CARTESIAN_POINT ( 'NONE',  ( -38.97867591359219119, -24.55319635012989110, 6.700000000000000178 ) ) ;
#36392 = CARTESIAN_POINT ( 'NONE',  ( 37.83867290611771494, -6.084034091406928191, -6.000000000000000000 ) ) ;
#36394 = DIRECTION ( 'NONE',  ( 0.000000000000000000, 0.000000000000000000, -1.000000000000000000 ) ) ;
#36395 = DIRECTION ( 'NONE',  ( 1.000000000000000000, 0.000000000000000000, 0.000000000000000000 ) ) ;
#36396 = DIRECTION ( 'NONE',  ( -0.000000000000000000, -0.000000000000000000, 1.000000000000000000 ) ) ;
#36397 = CARTESIAN_POINT ( 'NONE',  ( 23.89311878034035530, 3.219763706263101266, -3.577746201333754428 ) ) ;
#36398 = ORIENTED_EDGE ( 'NONE', *, *, #23652, .F. ) ;
#36399 = CARTESIAN_POINT ( 'NONE',  ( 5.022340310865588187, -30.29431027711538249, 6.865637334398153158 ) ) ;
#36400 = EDGE_CURVE ( 'NONE', #5208, #28633, #25374, .T. ) ;
#36401 = CARTESIAN_POINT ( 'NONE',  ( 22.67874324181232737, -4.030091496876125667, 7.802482278901700319 ) ) ;
#36402 = EDGE_CURVE ( 'NONE', #9101, #1346, #12601, .T. ) ;
#36403 = CARTESIAN_POINT ( 'NONE',  ( 2.896889677700020371, -32.75244314399080281, 7.691066658568946224 ) ) ;
#36404 = CARTESIAN_POINT ( 'NONE',  ( 11.65737507970504439, -23.60493063168009442, 6.800000000000000711 ) ) ;
#36405 = CARTESIAN_POINT ( 'NONE',  ( 81.06025503659105880, 64.27053461117903055, 3.341858160559717739 ) ) ;
#36406 = CARTESIAN_POINT ( 'NONE',  ( 85.64278173364962754, 1.868356560669967470, -5.099220668941490509 ) ) ;
#36407 = CARTESIAN_POINT ( 'NONE',  ( 5.123610338733788794, -30.29864684015847232, 7.753200566781575986 ) ) ;
#36408 = ORIENTED_EDGE ( 'NONE', *, *, #20472, .T. ) ;
#36409 = CARTESIAN_POINT ( 'NONE',  ( -0.5160548967603080239, -32.28747347318100935, 7.255881584735161205 ) ) ;
#36410 = CARTESIAN_POINT ( 'NONE',  ( -63.70768058868311812, 44.39675795731059793, -1.000000000000000000 ) ) ;
#36411 = CARTESIAN_POINT ( 'NONE',  ( 16.03358042430196306, -3.427093395206350479, -2.707976865299952518 ) ) ;
#36412 = CARTESIAN_POINT ( 'NONE',  ( 27.40617277722898493, 0.9610190317717227648, -4.483794101316670222 ) ) ;
#36413 = DIRECTION ( 'NONE',  ( -0.000000000000000000, -1.000000000000000000, -0.000000000000000000 ) ) ;
#36414 = CARTESIAN_POINT ( 'NONE',  ( 27.16624160081412853, 1.269200517689503593, -4.441067823234377876 ) ) ;
#36415 = CARTESIAN_POINT ( 'NONE',  ( -0.3487487021806359722, -26.64985754041175525, 6.800000000000000711 ) ) ;
#36416 = ORIENTED_EDGE ( 'NONE', *, *, #29943, .F. ) ;
#36417 = CARTESIAN_POINT ( 'NONE',  ( 36.89667292320353198, -3.000775245577192329, 5.965016177709391521 ) ) ;
#36418 = VECTOR ( 'NONE', #30872, 1000.000000000000000 ) ;
#36419 = CIRCLE ( 'NONE', #40431, 2.999999999999998668 ) ;
#36420 = CARTESIAN_POINT ( 'NONE',  ( 4.995180358529765385, -28.43394519631405970, 7.785593909369613819 ) ) ;
#36421 = ORIENTED_EDGE ( 'NONE', *, *, #13628, .T. ) ;
#36422 = VERTEX_POINT ( 'NONE', #37914 ) ;
#36423 = CARTESIAN_POINT ( 'NONE',  ( 37.00899628427189469, -3.246980710513998947, 5.946852153544761599 ) ) ;
#36424 = DIRECTION ( 'NONE',  ( -0.000000000000000000, -0.000000000000000000, 1.000000000000000000 ) ) ;
#36425 = CARTESIAN_POINT ( 'NONE',  ( 17.66378170928452818, -3.205320407151504902, -2.924525624963761672 ) ) ;
#36426 = DIRECTION ( 'NONE',  ( 0.000000000000000000, 0.000000000000000000, 1.000000000000000000 ) ) ;
#36427 = ORIENTED_EDGE ( 'NONE', *, *, #3853, .T. ) ;
#36428 = PLANE ( 'NONE',  #33890 ) ;
#36430 = EDGE_CURVE ( 'NONE', #5985, #12935, #32232, .T. ) ;
#36429 = VECTOR ( 'NONE', #38345, 1000.000000000000000 ) ;
#36431 = ORIENTED_EDGE ( 'NONE', *, *, #3264, .T. ) ;
#36432 = ORIENTED_EDGE ( 'NONE', *, *, #34848, .F. ) ;
#36433 = DIRECTION ( 'NONE',  ( 0.4826092789263634053, -0.5751513419797926741, 0.6605219282605379050 ) ) ;
#36434 = ORIENTED_EDGE ( 'NONE', *, *, #19424, .F. ) ;
#36435 = CARTESIAN_POINT ( 'NONE',  ( 14.77222197358542033, -4.491748702149269690, 2.511961485181798626 ) ) ;
#36436 = ORIENTED_EDGE ( 'NONE', *, *, #20437, .T. ) ;
#36438 = CARTESIAN_POINT ( 'NONE',  ( 4.337010013012764453, -27.42322653021406964, 7.785868773668302545 ) ) ;
#36437 = DIRECTION ( 'NONE',  ( -0.06975647374412530244, -0.9975640502598241977, 0.000000000000000000 ) ) ;
#36439 = CARTESIAN_POINT ( 'NONE',  ( 81.07719038108439236, 65.78599662769312317, -2.192618372227129520 ) ) ;
#36440 = ADVANCED_FACE ( 'NONE', ( #5618 ), #18158, .F. ) ;
#36441 = DIRECTION ( 'NONE',  ( -0.000000000000000000, -0.000000000000000000, -1.000000000000000000 ) ) ;
#36442 = ORIENTED_EDGE ( 'NONE', *, *, #39719, .T. ) ;
#36444 = CARTESIAN_POINT ( 'NONE',  ( 2.908949165453299734, -26.39197723079101010, 6.894806418505348589 ) ) ;
#36443 = CARTESIAN_POINT ( 'NONE',  ( -36.24874870218063450, -25.49307895267003587, 6.700000000000000178 ) ) ;
#36445 = CARTESIAN_POINT ( 'NONE',  ( -1.795422484021812926, -29.39876237255725400, 7.011627023500182965 ) ) ;
#36446 = CARTESIAN_POINT ( 'NONE',  ( 75.12771622566773999, 62.30414178837923345, 3.756674307852014394 ) ) ;
#36447 = CARTESIAN_POINT ( 'NONE',  ( 24.83382150147336986, 2.575822499426965617, -3.953843410308002237 ) ) ;
#36448 = DIRECTION ( 'NONE',  ( 0.8660254037844380415, 0.5000000000000009992, -0.000000000000000000 ) ) ;
#36449 = DIRECTION ( 'NONE',  ( -0.000000000000000000, -0.000000000000000000, -1.000000000000000000 ) ) ;
#36451 = ADVANCED_FACE ( 'NONE', ( #28245 ), #2966, .T. ) ;
#36450 = FACE_OUTER_BOUND ( 'NONE', #38301, .T. ) ;
#36452 = CARTESIAN_POINT ( 'NONE',  ( 1.090397816225957550, -0.5999999999999994227, -4.012069227840649788 ) ) ;
#36453 = CARTESIAN_POINT ( 'NONE',  ( -64.95171866297671670, 36.28765213650432031, 6.629387290673630417 ) ) ;
#36454 = CARTESIAN_POINT ( 'NONE',  ( 81.36794360107712976, 64.82106189941464436, 2.952528780688829624 ) ) ;
#36455 = CARTESIAN_POINT ( 'NONE',  ( 87.97568001472090771, -0.4607347734944167716, -3.153239710520575390 ) ) ;
#36456 = CARTESIAN_POINT ( 'NONE',  ( 29.20850709934801159, 2.242166301403143880, -0.5075834600922535245 ) ) ;
#36457 = AXIS2_PLACEMENT_3D ( 'NONE', #33654, #15301, #37326 ) ;
#36458 = CARTESIAN_POINT ( 'NONE',  ( -72.87804133339554369, 1.626223713339684629, -10.95881965187203377 ) ) ;
#36459 = CARTESIAN_POINT ( 'NONE',  ( 33.12434724996504798, -3.753162291981519516, 5.124365322589720328 ) ) ;
#36460 = DIRECTION ( 'NONE',  ( 0.000000000000000000, 0.000000000000000000, 1.000000000000000000 ) ) ;
#36461 = CARTESIAN_POINT ( 'NONE',  ( 33.68123845448776166, -3.186000923572973154, -5.463169863251220448 ) ) ;
#36462 = CARTESIAN_POINT ( 'NONE',  ( -42.44874870218064444, -26.64985754041175525, 6.700000000000000178 ) ) ;
#36463 = CARTESIAN_POINT ( 'NONE',  ( 4.672147420734682477, -31.41889161793999463, 6.865482280155366546 ) ) ;
#36464 = CYLINDRICAL_SURFACE ( 'NONE', #35552, 0.1000000000000028644 ) ;
#36465 =( BOUNDED_CURVE ( )  B_SPLINE_CURVE ( 3, ( #40317, #18084, #2482, #24058 ),
 .UNSPECIFIED., .F., .T. ) 
 B_SPLINE_CURVE_WITH_KNOTS ( ( 4, 4 ),
 ( 4.748221474220558846, 4.941946782021393147 ),
 .UNSPECIFIED. ) 
 CURVE ( )  GEOMETRIC_REPRESENTATION_ITEM ( )  RATIONAL_B_SPLINE_CURVE ( ( 1.000000000000000000, 0.9968749865767494445, 0.9968749865767494445, 1.000000000000000000 ) ) 
 REPRESENTATION_ITEM ( '' )  );
#36466 = CARTESIAN_POINT ( 'NONE',  ( 4.310691338497240288, -31.89452001513661727, 7.771081512783700518 ) ) ;
#36467 = CARTESIAN_POINT ( 'NONE',  ( 1.736346942945644400, -33.06974547922812491, 7.695279973900954751 ) ) ;
#36468 = VERTEX_POINT ( 'NONE', #5824 ) ;
#36469 = CARTESIAN_POINT ( 'NONE',  ( 23.34994303252841163, 3.524623506009445961, 3.233127816796116605 ) ) ;
#36470 = B_SPLINE_CURVE_WITH_KNOTS ( 'NONE', 3,
 ( #8943, #24815, #21528, #22143, #28507, #34104, #34506, #15747, #28299, #18210, #6281, #30801, #31003, #31606, #18830, #27885, #31403, #34308, #12241, #3228, #18613, #9152, #119, #12650, #25225 ),
 .UNSPECIFIED., .F., .F.,
 ( 4, 3, 3, 3, 3, 3, 3, 3, 4 ),
 ( 6.468151674593503617E-05, 9.076621574721972265E-05, 0.0001210204262067955813, 0.0001512763324577427520, 0.0001815301820994167140, 0.0002117781465860681307, 0.0002420274594459719550, 0.0002722905548971150838, 0.0002816827545175578664 ),
 .UNSPECIFIED. ) ;
#36471 = CARTESIAN_POINT ( 'NONE',  ( -22.24874870218063450, -25.49307895267003587, 6.800000000000000711 ) ) ;
#36472 = EDGE_CURVE ( 'NONE', #169, #30629, #29986, .T. ) ;
#36473 = CARTESIAN_POINT ( 'NONE',  ( 66.73816075044196339, 57.82680446425992926, -3.998864354716218816 ) ) ;
#36474 = CARTESIAN_POINT ( 'NONE',  ( -71.92837670882107659, -0.6507271787433660526, 9.949874371066202983 ) ) ;
#36475 = CARTESIAN_POINT ( 'NONE',  ( -1.338463389079526777, -27.83344699523806298, 7.638132480492515697 ) ) ;
#36476 = VECTOR ( 'NONE', #6247, 1000.000000000000000 ) ;
#36477 = ORIENTED_EDGE ( 'NONE', *, *, #7679, .T. ) ;
#36478 = AXIS2_PLACEMENT_3D ( 'NONE', #37513, #270, #9727 ) ;
#36479 = DIRECTION ( 'NONE',  ( 0.6427876096865481337, -0.7660444431189706860, -0.000000000000000000 ) ) ;
#36480 = CARTESIAN_POINT ( 'NONE',  ( 3.877316292843988155, -32.18164630026152651, 7.775108481317165143 ) ) ;
#36481 = CARTESIAN_POINT ( 'NONE',  ( 84.98973554254388318, 1.887807287779055709, -4.881612716162457843 ) ) ;
#36482 = CARTESIAN_POINT ( 'NONE',  ( -77.50518483875032416, 11.08526101523151475, 7.544008514241666852 ) ) ;
#36483 = AXIS2_PLACEMENT_3D ( 'NONE', #24365, #36928, #15095 ) ;
#36484 = EDGE_CURVE ( 'NONE', #13345, #6019, #21426, .T. ) ;
#36485 = DIRECTION ( 'NONE',  ( 1.000000000000000000, 0.000000000000000000, 0.000000000000000000 ) ) ;
#36486 = LINE ( 'NONE', #7874, #39606 ) ;
#36487 = VERTEX_POINT ( 'NONE', #4168 ) ;
#36488 = CARTESIAN_POINT ( 'NONE',  ( 24.75344691226916893, 3.017249892964377622, 3.359965021756160741 ) ) ;
#36489 = CARTESIAN_POINT ( 'NONE',  ( 82.58199242721477162, 63.55547749749366915, -1.287552078898777541 ) ) ;
#36490 = AXIS2_PLACEMENT_3D ( 'NONE', #20567, #19972, #23855 ) ;
#36491 = EDGE_CURVE ( 'NONE', #14346, #23464, #10113, .T. ) ;
#36492 = CARTESIAN_POINT ( 'NONE',  ( 81.17805228937325523, 61.98952396227124950, 2.700485128497479792 ) ) ;
#36493 = CARTESIAN_POINT ( 'NONE',  ( -0.1694320636984359418, -32.40961275103795458, 6.911401339314954484 ) ) ;
#36494 = EDGE_LOOP ( 'NONE', ( #30262, #33099, #24622, #5013 ) ) ;
#36495 = CARTESIAN_POINT ( 'NONE',  ( 78.33250027093576762, 62.86460196216434326, -3.816136337383043475 ) ) ;
#36497 = CARTESIAN_POINT ( 'NONE',  ( 2.255382727820350652, -26.21553259517144951, 7.692469944509197965 ) ) ;
#36496 = CARTESIAN_POINT ( 'NONE',  ( 22.60277826478245800, 0.2789680342660347256, 6.515017021779732964 ) ) ;
#36498 = CARTESIAN_POINT ( 'NONE',  ( 81.43301797337205983, 62.09285590259236898, -2.578835243349320461 ) ) ;
#36499 = CARTESIAN_POINT ( 'NONE',  ( 79.06939945841558881, 62.09164075111542758, 3.616565173810706746 ) ) ;
#36500 = CARTESIAN_POINT ( 'NONE',  ( -0.9199683733837696886, -27.40342225418419631, 7.740055089680393685 ) ) ;
#36501 = ADVANCED_FACE ( 'NONE', ( #22503 ), #28867, .T. ) ;
#36502 = CARTESIAN_POINT ( 'NONE',  ( 78.69012442119817763, 66.05840891509440382, 1.017094602978567242 ) ) ;
#36504 = CARTESIAN_POINT ( 'NONE',  ( 63.05383694556373797, -7.271989087314214117, -6.000000000000000000 ) ) ;
#36503 = DIRECTION ( 'NONE',  ( 1.000000000000000000, 0.000000000000000000, 0.000000000000000000 ) ) ;
#36505 = CARTESIAN_POINT ( 'NONE',  ( 27.77988552260176291, -0.3358138158918914651, -6.029166980063449088 ) ) ;
#36506 = CARTESIAN_POINT ( 'NONE',  ( -1.773773684162445852, -29.99442361894472953, 6.989977667959445640 ) ) ;
#36507 = CARTESIAN_POINT ( 'NONE',  ( -75.45330471031414277, 33.71485196875532608, 15.50000000000000000 ) ) ;
#36508 = EDGE_LOOP ( 'NONE', ( #34867, #39357 ) ) ;
#36509 = CARTESIAN_POINT ( 'NONE',  ( -14.87867591359218977, -24.55319635012989110, 6.700000000000000178 ) ) ;
#36510 = CARTESIAN_POINT ( 'NONE',  ( 21.78348496727135952, 0.2136468579297728376, -8.398162227918549050 ) ) ;
#36511 = CARTESIAN_POINT ( 'NONE',  ( -68.92837670882107659, -42.87473357531881391, 0.000000000000000000 ) ) ;
#36512 = AXIS2_PLACEMENT_3D ( 'NONE', #23646, #36213, #33133 ) ;
#36513 = CARTESIAN_POINT ( 'NONE',  ( 4.882868366733327470, -28.37333834040810032, 7.695279973900954751 ) ) ;
#36514 = VECTOR ( 'NONE', #1611, 1000.000000000000000 ) ;
#36515 = FACE_OUTER_BOUND ( 'NONE', #40637, .T. ) ;
#36516 = CARTESIAN_POINT ( 'NONE',  ( -70.92837670882107659, -48.61702805680358352, 10.00000000000000888 ) ) ;
#36517 = CARTESIAN_POINT ( 'NONE',  ( 37.17584199213645491, -2.565478455631990951, -5.981118737177594014 ) ) ;
#36518 = CARTESIAN_POINT ( 'NONE',  ( 1.129853303793442620, -32.92172554530420570, 7.643333865083955736 ) ) ;
#36519 = DIRECTION ( 'NONE',  ( 0.000000000000000000, 0.000000000000000000, 1.000000000000000000 ) ) ;
#36520 = CARTESIAN_POINT ( 'NONE',  ( 4.997854627175230213, -30.74328504515684912, 7.651421919295145813 ) ) ;
#36521 = CARTESIAN_POINT ( 'NONE',  ( 2.725517943428533929, -32.81170637720346406, 6.868387053540520704 ) ) ;
#36522 = CARTESIAN_POINT ( 'NONE',  ( 5.095993465723490878, -29.74278196016128462, 6.882085323592687764 ) ) ;
#36523 = AXIS2_PLACEMENT_3D ( 'NONE', #11030, #11434, #21139 ) ;
#36524 = EDGE_CURVE ( 'NONE', #20068, #37067, #38720, .T. ) ;
#36525 = DIRECTION ( 'NONE',  ( 1.000000000000000000, 0.000000000000000000, 0.000000000000000000 ) ) ;
#36526 = EDGE_CURVE ( 'NONE', #9395, #25044, #8284, .T. ) ;
#36527 = ORIENTED_EDGE ( 'NONE', *, *, #35359, .T. ) ;
#36528 = CARTESIAN_POINT ( 'NONE',  ( 66.57374945270225908, 57.82325632336715415, 3.999874661881728688 ) ) ;
#36529 = CARTESIAN_POINT ( 'NONE',  ( 72.85835069609119330, 61.31913755009141909, -3.785151435630688788 ) ) ;
#36530 = VERTEX_POINT ( 'NONE', #32371 ) ;
#36531 = FACE_OUTER_BOUND ( 'NONE', #35596, .T. ) ;
#36532 = CARTESIAN_POINT ( 'NONE',  ( -0.6763298692248193023, -32.13921067023287037, 7.013842709614101167 ) ) ;
#36533 = CARTESIAN_POINT ( 'NONE',  ( 3.058269330830037713, -26.45285399309853602, 6.959317978105167057 ) ) ;
#36534 = EDGE_CURVE ( 'NONE', #38171, #4832, #40527, .T. ) ;
#36535 = ADVANCED_FACE ( 'NONE', ( #19398 ), #13408, .F. ) ;
#36536 = DIRECTION ( 'NONE',  ( -0.9267318687906771491, 0.3757233601570964532, 0.000000000000000000 ) ) ;
#36537 = FACE_BOUND ( 'NONE', #12800, .T. ) ;
#36538 = ORIENTED_EDGE ( 'NONE', *, *, #18206, .T. ) ;
#36539 = ADVANCED_FACE ( 'NONE', ( #9922 ), #7035, .F. ) ;
#36540 = DIRECTION ( 'NONE',  ( -0.000000000000000000, 0.000000000000000000, 1.000000000000000000 ) ) ;
#36541 = AXIS2_PLACEMENT_3D ( 'NONE', #2248, #14988, #36813 ) ;
#36542 = VECTOR ( 'NONE', #31130, 1000.000000000000000 ) ;
#36543 = CARTESIAN_POINT ( 'NONE',  ( 80.61353453797053703, 61.63497835834534300, -2.716276829189519404 ) ) ;
#36544 =( BOUNDED_CURVE ( )  B_SPLINE_CURVE ( 3, ( #21976, #28756, #12493, #157 ),
 .UNSPECIFIED., .F., .T. ) 
 B_SPLINE_CURVE_WITH_KNOTS ( ( 4, 4 ),
 ( 1.347909859412853129, 1.534781240595298968 ),
 .UNSPECIFIED. ) 
 CURVE ( )  GEOMETRIC_REPRESENTATION_ITEM ( )  RATIONAL_B_SPLINE_CURVE ( ( 1.000000000000000000, 0.9970920404276225613, 0.9970920404276225613, 1.000000000000000000 ) ) 
 REPRESENTATION_ITEM ( '' )  );
#36545 = CARTESIAN_POINT ( 'NONE',  ( 78.38646849266343963, 65.84297019793960715, 1.584170212883424300 ) ) ;
#36546 = AXIS2_PLACEMENT_3D ( 'NONE', #28043, #18994, #8891 ) ;
#36547 = CARTESIAN_POINT ( 'NONE',  ( 22.14454166288778580, 4.578504518513106802, 3.662589312894346083 ) ) ;
#36548 = DIRECTION ( 'NONE',  ( -0.8831583674550994578, 0.4690749385695672791, 0.000000000000000000 ) ) ;
#36549 = CARTESIAN_POINT ( 'NONE',  ( 20.40287464734031531, 10.75613383782063970, 2.500000000000000000 ) ) ;
#36550 = CARTESIAN_POINT ( 'NONE',  ( 21.85643539959780313, 0.4758835581198413989, -14.20546615820951963 ) ) ;
#36551 = ORIENTED_EDGE ( 'NONE', *, *, #345, .F. ) ;
#36552 = CARTESIAN_POINT ( 'NONE',  ( -77.86968774964118722, 9.956382404624021021, 7.211963008493430749 ) ) ;
#36553 = DIRECTION ( 'NONE',  ( 0.000000000000000000, 0.000000000000000000, 1.000000000000000000 ) ) ;
#36554 = CARTESIAN_POINT ( 'NONE',  ( -80.20198641814972973, 10.53012318711579454, -3.762333814409368760 ) ) ;
#36555 = CARTESIAN_POINT ( 'NONE',  ( 1.491073016268174678, -32.96348093246033528, 6.969307238440506147 ) ) ;
#36556 = CARTESIAN_POINT ( 'NONE',  ( -28.34874870218063947, -26.64985754041175525, 6.700000000000000178 ) ) ;
#36557 = CARTESIAN_POINT ( 'NONE',  ( 4.906539508589050413, -30.70157509802881890, 7.670860738520331346 ) ) ;
#36558 = CARTESIAN_POINT ( 'NONE',  ( 14.76778848929227372, 12.79472506199442172, 2.506269218290250400 ) ) ;
#36559 = CARTESIAN_POINT ( 'NONE',  ( -70.92837670882107659, -60.53509472482660669, 7.538952224936807056 ) ) ;
#36560 = CARTESIAN_POINT ( 'NONE',  ( 0.6790634579381706892, -26.22225927169515458, 6.989977667959444751 ) ) ;
#36561 = EDGE_CURVE ( 'NONE', #1980, #30840, #876, .T. ) ;
#36562 = CARTESIAN_POINT ( 'NONE',  ( 4.494975343341260476, -27.46272638530924226, 6.912143950357350519 ) ) ;
#36563 = DIRECTION ( 'NONE',  ( 1.000000000000000000, 0.000000000000000000, 0.000000000000000000 ) ) ;
#36564 = CARTESIAN_POINT ( 'NONE',  ( 4.244032359733176385, -31.82602863437616136, 6.866852738645441434 ) ) ;
#36565 = ORIENTED_EDGE ( 'NONE', *, *, #7725, .T. ) ;
#36566 = MECHANICAL_DESIGN_GEOMETRIC_PRESENTATION_REPRESENTATION (  '', ( #31327 ), #9627 ) ;
#36567 = CARTESIAN_POINT ( 'NONE',  ( 68.07944445521805221, 58.24657026194513776, 3.992939643064506328 ) ) ;
#36568 = CARTESIAN_POINT ( 'NONE',  ( 36.89767088514894056, -3.003071912148901568, 5.965171933806773019 ) ) ;
#36569 = ADVANCED_FACE ( 'NONE', ( #7237 ), #19800, .T. ) ;
#36570 = VECTOR ( 'NONE', #16100, 1000.000000000000000 ) ;
#36571 = CARTESIAN_POINT ( 'NONE',  ( 81.16957891225059996, 61.30398062001309256, -1.000000000000000000 ) ) ;
#36573 = ADVANCED_FACE ( 'NONE', ( #13615 ), #4370, .T. ) ;
#36572 = CARTESIAN_POINT ( 'NONE',  ( 86.63338141420044280, 0.5786414684654883622, -5.958757720264261870 ) ) ;
#36576 = CARTESIAN_POINT ( 'NONE',  ( 31.50304906168603125, -0.4789496544865932681, -5.123210728833553773 ) ) ;
#36575 = VECTOR ( 'NONE', #29865, 1000.000000000000227 ) ;
#36574 = CARTESIAN_POINT ( 'NONE',  ( -22.97867591359219119, -24.55319635012989110, 6.700000000000000178 ) ) ;
#36577 = CARTESIAN_POINT ( 'NONE',  ( 4.984179672459081445, -25.57221830738312107, 7.695279973900954751 ) ) ;
#36578 = CARTESIAN_POINT ( 'NONE',  ( -1.634384595334445578, -28.90707823045441671, 6.874555630061440326 ) ) ;
#36579 = CARTESIAN_POINT ( 'NONE',  ( -58.64967482348268391, 27.97946873212458030, 5.671478272894446171 ) ) ;
#36580 = DIRECTION ( 'NONE',  ( 1.000000000000000000, 0.000000000000000000, 0.000000000000000000 ) ) ;
#36581 = EDGE_CURVE ( 'NONE', #23038, #14737, #38920, .T. ) ;
#36582 = VERTEX_POINT ( 'NONE', #28667 ) ;
#36583 = CARTESIAN_POINT ( 'NONE',  ( -69.93073207689441517, -20.86216845902604078, 3.916479336966924407 ) ) ;
#36584 = PRODUCT_DEFINITION_CONTEXT ( 'detailed design', #6089, 'design' ) ;
#36585 = ADVANCED_FACE ( 'NONE', ( #25574 ), #17696, .F. ) ;
#36586 = ORIENTED_EDGE ( 'NONE', *, *, #32509, .T. ) ;
#36587 = ORIENTED_EDGE ( 'NONE', *, *, #37520, .T. ) ;
#36588 = CARTESIAN_POINT ( 'NONE',  ( 78.64443580140851964, 65.97314938607593149, -1.660510093083306105 ) ) ;
#36589 = CARTESIAN_POINT ( 'NONE',  ( -1.573542698591475997, -28.33242721227279759, 6.883108633650831365 ) ) ;
#36590 = CARTESIAN_POINT ( 'NONE',  ( 80.69932603693817441, 62.65430898200613541, 3.392181771880192098 ) ) ;
#36591 = CARTESIAN_POINT ( 'NONE',  ( 22.41436559212412760, 0.3887359917284659017, 6.830184646630694800 ) ) ;
#36593 = EDGE_LOOP ( 'NONE', ( #28891, #4940, #37474, #31592 ) ) ;
#36592 = CARTESIAN_POINT ( 'NONE',  ( 4.735674590641913539, -27.84972924505143510, 7.781480525794718162 ) ) ;
#36594 = CARTESIAN_POINT ( 'NONE',  ( 73.28665133690081745, 61.87344754340890063, -3.624554307483654814 ) ) ;
#36595 = CARTESIAN_POINT ( 'NONE',  ( 3.220794542350093881, -32.61104474200681835, 6.920489980334479263 ) ) ;
#36597 = FACE_OUTER_BOUND ( 'NONE', #29245, .T. ) ;
#36596 = LINE ( 'NONE', #14153, #23895 ) ;
#36598 = CARTESIAN_POINT ( 'NONE',  ( -62.92837670882107659, -49.49506129533733656, 6.000000000000000000 ) ) ;
#36599 = LINE ( 'NONE', #38869, #23843 ) ;
#36600 = CARTESIAN_POINT ( 'NONE',  ( 22.42542530853210181, 4.782089792738570821, -3.164282654266882933 ) ) ;
#36601 = ORIENTED_EDGE ( 'NONE', *, *, #5633, .T. ) ;
#36602 = CARTESIAN_POINT ( 'NONE',  ( 1.826415646469069731, -26.07219983930859897, 7.750000000000000888 ) ) ;
#36603 = AXIS2_PLACEMENT_3D ( 'NONE', #5526, #24670, #15608 ) ;
#36604 = CARTESIAN_POINT ( 'NONE',  ( 22.31703049540045924, 6.264542857755036387, 0.009563241200241559548 ) ) ;
#36605 = CARTESIAN_POINT ( 'NONE',  ( 0.3442295505392951038, -32.69542910597172636, 7.386948897581449458 ) ) ;
#36606 = CARTESIAN_POINT ( 'NONE',  ( 1.052472996047527642, -32.99480600882493775, 7.785096263473212375 ) ) ;
#36607 = CARTESIAN_POINT ( 'NONE',  ( 81.47197553453356988, 61.72158698297663193, 1.969816429103234290 ) ) ;
#36608 = CARTESIAN_POINT ( 'NONE',  ( 84.43092178082896737, 2.949567725576020649, 1.921192885956162444 ) ) ;
#36609 = CARTESIAN_POINT ( 'NONE',  ( -19.07867591359219972, -26.64985754041175525, 6.700000000000000178 ) ) ;
#36610 = ORIENTED_EDGE ( 'NONE', *, *, #36082, .T. ) ;
#36611 = CARTESIAN_POINT ( 'NONE',  ( 23.03318261145397017, 4.443153149067368801, -2.273821518518992502 ) ) ;
#36612 = CARTESIAN_POINT ( 'NONE',  ( 16.07587011183210635, -3.522579363632067917, -2.698830145762970645 ) ) ;
#36613 = CARTESIAN_POINT ( 'NONE',  ( 36.19300506522036187, -2.234529143593806388, -5.855191790199620883 ) ) ;
#36614 = CARTESIAN_POINT ( 'NONE',  ( 1.682951012397970292, -26.06997362959739206, 7.750000000000000888 ) ) ;
#36615 = CARTESIAN_POINT ( 'NONE',  ( 27.07499125159621300, 1.335026952719597926, -4.423825550918643934 ) ) ;
#36616 = CARTESIAN_POINT ( 'NONE',  ( -0.4828924690311028889, -26.96353856790022974, 7.769368695748486431 ) ) ;
#36617 = ORIENTED_EDGE ( 'NONE', *, *, #27926, .T. ) ;
#36618 = CARTESIAN_POINT ( 'NONE',  ( 33.68750564893161936, -3.098785954741594573, 5.464148010559176427 ) ) ;
#36619 = CARTESIAN_POINT ( 'NONE',  ( 85.39749695915146788, 2.435202802470831873, -2.633776547657810774 ) ) ;
#36620 = ORIENTED_EDGE ( 'NONE', *, *, #17362, .T. ) ;
#36621 = ORIENTED_EDGE ( 'NONE', *, *, #20437, .F. ) ;
#36623 = CARTESIAN_POINT ( 'NONE',  ( 32.07039327229519898, 0.2549240838516523278, 4.723724623685981783 ) ) ;
#36622 = CARTESIAN_POINT ( 'NONE',  ( 80.80706632665068412, 63.75484916101672894, -3.549391953833849644 ) ) ;
#36624 = CARTESIAN_POINT ( 'NONE',  ( -69.42837670882107659, -47.31299788476771084, 9.886859966642605357 ) ) ;
#36625 = CARTESIAN_POINT ( 'NONE',  ( 21.09191007886703062, -3.054293775446101478, -3.415671279545484218 ) ) ;
#36626 = FACE_OUTER_BOUND ( 'NONE', #28195, .T. ) ;
#36627 = CIRCLE ( 'NONE', #39920, 5.329987104167474676 ) ;
#36628 = ADVANCED_FACE ( 'NONE', ( #20387 ), #5364, .F. ) ;
#36629 = ORIENTED_EDGE ( 'NONE', *, *, #40163, .T. ) ;
#36630 = CARTESIAN_POINT ( 'NONE',  ( 1.513399906207050449, -32.96478432900200062, 7.013842709614101167 ) ) ;
#36631 = EDGE_CURVE ( 'NONE', #35842, #22149, #17484, .T. ) ;
#36632 = VERTEX_POINT ( 'NONE', #36060 ) ;
#36633 = EDGE_CURVE ( 'NONE', #17865, #31330, #6353, .T. ) ;
#36634 = ORIENTED_EDGE ( 'NONE', *, *, #386, .F. ) ;
#36635 = LINE ( 'NONE', #11905, #23329 ) ;
#36636 = CARTESIAN_POINT ( 'NONE',  ( 81.15397050155254988, 61.44050475792813160, -1.896863055073852111 ) ) ;
#36637 = FACE_OUTER_BOUND ( 'NONE', #17168, .T. ) ;
#36638 = ORIENTED_EDGE ( 'NONE', *, *, #3152, .T. ) ;
#36640 = DIRECTION ( 'NONE',  ( -0.000000000000000000, 1.000000000000000000, -0.000000000000000000 ) ) ;
#36639 = CARTESIAN_POINT ( 'NONE',  ( 4.815892087276667510, -27.97503390834088677, 6.903112506833889661 ) ) ;
#36641 = ORIENTED_EDGE ( 'NONE', *, *, #4069, .F. ) ;
#36642 = CARTESIAN_POINT ( 'NONE',  ( 21.83430649484399311, 4.714758532028221261, 3.915150708602226359 ) ) ;
#36643 = CARTESIAN_POINT ( 'NONE',  ( 78.95874065903551298, 66.19121013986814717, -1.203271478923241933 ) ) ;
#36644 = CARTESIAN_POINT ( 'NONE',  ( 4.739426510580063479, -28.04537359934935736, 6.997764925645181933 ) ) ;
#36645 = ORIENTED_EDGE ( 'NONE', *, *, #18112, .F. ) ;
#36647 = CARTESIAN_POINT ( 'NONE',  ( 22.13428935428179400, -2.652497287587405772, -3.660989192183361052 ) ) ;
#36646 = CARTESIAN_POINT ( 'NONE',  ( -0.03065438358791758300, -26.64358689880297248, 7.695279973900954751 ) ) ;
#36648 = CARTESIAN_POINT ( 'NONE',  ( -1.794351914757954303, -29.37815317404309923, 6.941203072598476354 ) ) ;
#36649 = CARTESIAN_POINT ( 'NONE',  ( 75.72894860151858154, 61.00966332974834927, 3.846775394605490561 ) ) ;
#36650 = CARTESIAN_POINT ( 'NONE',  ( 24.31786857884458541, 2.722531517372515975, -3.914669340711137036 ) ) ;
#36651 = CARTESIAN_POINT ( 'NONE',  ( 0.5248424762351729944, -26.37961863118246697, 7.635761828346577573 ) ) ;
#36652 = CARTESIAN_POINT ( 'NONE',  ( -4.444218661349752963, -35.94265729135299381, 6.000000000000000000 ) ) ;
#36653 = LINE ( 'NONE', #5567, #34180 ) ;
#36654 = CARTESIAN_POINT ( 'NONE',  ( -4.348748702180639469, -26.64985754041175525, 6.800000000000000711 ) ) ;
#36655 = CARTESIAN_POINT ( 'NONE',  ( -67.80647484265466574, 37.44505118619654382, 9.800414904977209574 ) ) ;
#36656 = CARTESIAN_POINT ( 'NONE',  ( 81.38476203741942072, 61.42515712988158327, 1.285939662725141597 ) ) ;
#36657 = CARTESIAN_POINT ( 'NONE',  ( 87.36631219772915813, 0.2237360808920199895, 4.554730944530843040 ) ) ;
#36658 = CARTESIAN_POINT ( 'NONE',  ( 29.43591252028664584, 1.494051637964393553, 3.776330930280134002 ) ) ;
#36659 = PRESENTATION_LAYER_ASSIGNMENT (  '', '', ( #39862 ) ) ;
#36660 = CARTESIAN_POINT ( 'NONE',  ( -89.20959394718985891, -29.55642757665872722, 7.635761828346577573 ) ) ;
#36661 = CARTESIAN_POINT ( 'NONE',  ( 16.28057921272570496, -3.484615921975166231, 2.724815388562823681 ) ) ;
#36662 = CARTESIAN_POINT ( 'NONE',  ( -75.45330471031414277, 33.71485196875532608, 9.800414904976365804 ) ) ;
#36663 = CARTESIAN_POINT ( 'NONE',  ( 36.90757751090616523, -3.026075607118911215, -5.966718102348832709 ) ) ;
#36664 = CARTESIAN_POINT ( 'NONE',  ( 4.642268686586925597, -31.46607214451510615, 7.011627023500183853 ) ) ;
#36665 = CARTESIAN_POINT ( 'NONE',  ( -40.97867591359219119, -24.55319635012989110, 6.700000000000000178 ) ) ;
#36666 = CARTESIAN_POINT ( 'NONE',  ( -66.52162472956945294, 28.72470171467712063, 0.000000000000000000 ) ) ;
#36667 = DIRECTION ( 'NONE',  ( -1.000000000000000000, 0.000000000000000000, 0.000000000000000000 ) ) ;
#36668 = ORIENTED_EDGE ( 'NONE', *, *, #38624, .T. ) ;
#36669 = CARTESIAN_POINT ( 'NONE',  ( 36.39216306811729851, -1.827485476554924437, 5.788500282070289771 ) ) ;
#36670 = AXIS2_PLACEMENT_3D ( 'NONE', #25471, #6332, #34562 ) ;
#36671 = CARTESIAN_POINT ( 'NONE',  ( -71.03752578197757828, 0.2110339550563472832, 3.999007124502271804 ) ) ;
#36672 = CARTESIAN_POINT ( 'NONE',  ( 67.02270721038308920, 57.95726884087558517, -3.999016414675010900 ) ) ;
#36673 = CARTESIAN_POINT ( 'NONE',  ( -0.5531492059869442812, -26.89374777234154124, 7.762796336881263137 ) ) ;
#36674 = AXIS2_PLACEMENT_3D ( 'NONE', #17959, #14267, #33228 ) ;
#36675 = ORIENTED_EDGE ( 'NONE', *, *, #29942, .F. ) ;
#36676 = CARTESIAN_POINT ( 'NONE',  ( -0.5754365072339435727, -32.09591863859081684, 7.757178535559534183 ) ) ;
#36678 = EDGE_CURVE ( 'NONE', #36582, #36858, #26811, .T. ) ;
#36677 = CARTESIAN_POINT ( 'NONE',  ( 3.855084250238081101, -32.20002288419953373, 7.784838882742139532 ) ) ;
#36679 = CARTESIAN_POINT ( 'NONE',  ( 73.32807694493881456, 62.33902570990260017, 3.356114863723819397 ) ) ;
#36680 = CARTESIAN_POINT ( 'NONE',  ( -74.39026271145056057, 9.085113976877558173, 9.386028689943199055 ) ) ;
#36681 = FACE_OUTER_BOUND ( 'NONE', #4308, .T. ) ;
#36682 = ORIENTED_EDGE ( 'NONE', *, *, #12742, .F. ) ;
#36683 = DIRECTION ( 'NONE',  ( 1.000000000000000000, 0.000000000000000000, 0.000000000000000000 ) ) ;
#36684 = EDGE_CURVE ( 'NONE', #23873, #1854, #5694, .T. ) ;
#36685 = VECTOR ( 'NONE', #35799, 999.9999999999998863 ) ;
#36686 = CYLINDRICAL_SURFACE ( 'NONE', #192, 0.1000000000000028644 ) ;
#36687 = ORIENTED_EDGE ( 'NONE', *, *, #33958, .F. ) ;
#36688 = CARTESIAN_POINT ( 'NONE',  ( 21.99269358992065193, 5.592676286834311838, 3.104126389907300165 ) ) ;
#36689 = CARTESIAN_POINT ( 'NONE',  ( 82.56222392620334460, 63.90769089702597228, -1.153249692834613427 ) ) ;
#36690 = CARTESIAN_POINT ( 'NONE',  ( 78.96442931663766274, 65.90663607296401949, 2.147349935851028846 ) ) ;
#36691 = CARTESIAN_POINT ( 'NONE',  ( 23.40522682912259000, 3.763699709236936641, -3.087242233077766684 ) ) ;
#36692 = ORIENTED_EDGE ( 'NONE', *, *, #27216, .T. ) ;
#36693 = CARTESIAN_POINT ( 'NONE',  ( 78.95981124517786043, 62.31610944509169769, -3.691425412862293420 ) ) ;
#36695 = CARTESIAN_POINT ( 'NONE',  ( 14.74076604532273294, -4.695325025251882778, -2.506186015952889701 ) ) ;
#36694 = CARTESIAN_POINT ( 'NONE',  ( 24.74480270654332514, 0.5641214079007167426, 4.778945666302679030 ) ) ;
#36696 = CARTESIAN_POINT ( 'NONE',  ( 81.36421798834938102, 61.51166984027132401, -1.726519205788531242 ) ) ;
#36697 = CARTESIAN_POINT ( 'NONE',  ( 79.79883522896109582, 62.08831372790999126, 3.424416364708440241 ) ) ;
#36698 = CARTESIAN_POINT ( 'NONE',  ( 36.27994091153181699, -3.621545396486653967, -5.740730168913134257 ) ) ;
#36699 = ORIENTED_EDGE ( 'NONE', *, *, #12365, .T. ) ;
#36700 = CARTESIAN_POINT ( 'NONE',  ( 78.69027363540493525, 66.05851491966868139, 1.011532654301222633 ) ) ;
#36702 = CARTESIAN_POINT ( 'NONE',  ( 59.69572451838116933, -0.8894979772356270686, -6.000000000000000000 ) ) ;
#36701 = CARTESIAN_POINT ( 'NONE',  ( 3.374961858174662765, -26.61090707544855150, 7.730758795053814580 ) ) ;
#36703 = CIRCLE ( 'NONE', #39997, 5.950000000000010836 ) ;
#36704 = CARTESIAN_POINT ( 'NONE',  ( 29.67594332454466866, -2.985454744488035494, -5.114964129314456542 ) ) ;
#36705 = ADVANCED_FACE ( 'NONE', ( #23685 ), #17288, .T. ) ;
#36706 = CARTESIAN_POINT ( 'NONE',  ( 14.77500326541903952, -5.175625724643098557, -2.499997102511863911 ) ) ;
#36707 = FACE_OUTER_BOUND ( 'NONE', #14273, .T. ) ;
#36708 = ORIENTED_EDGE ( 'NONE', *, *, #10039, .T. ) ;
#36709 = CYLINDRICAL_SURFACE ( 'NONE', #32100, 0.09010775117052761962 ) ;
#36710 = FACE_OUTER_BOUND ( 'NONE', #32720, .T. ) ;
#36711 = DIRECTION ( 'NONE',  ( -1.000000000000000000, 0.000000000000000000, 0.000000000000000000 ) ) ;
#36712 = CARTESIAN_POINT ( 'NONE',  ( 0.5371711504799139281, -32.87097875789517332, 7.695279973900954751 ) ) ;
#36713 = CARTESIAN_POINT ( 'NONE',  ( -71.72694006223731833, -0.1672829062043898751, 3.947339383436517135 ) ) ;
#36714 = CARTESIAN_POINT ( 'NONE',  ( 33.68467625662385956, -3.836896542393491316, -5.141322647849833061 ) ) ;
#36715 = CARTESIAN_POINT ( 'NONE',  ( 3.374874343695283940, -26.61085896171689669, 7.661510568013103928 ) ) ;
#36716 = LINE ( 'NONE', #17762, #9776 ) ;
#36717 = LINE ( 'NONE', #24781, #37741 ) ;
#36718 = LINE ( 'NONE', #8501, #38355 ) ;
#36719 = DIRECTION ( 'NONE',  ( 0.000000000000000000, 0.000000000000000000, 1.000000000000000000 ) ) ;
#36720 = CARTESIAN_POINT ( 'NONE',  ( 4.628153510667976533, -27.84128456964326759, 7.670860738520332234 ) ) ;
#36721 = CARTESIAN_POINT ( 'NONE',  ( 4.932896964134850570, -28.51593809159530934, 7.761597726988850532 ) ) ;
#36722 = VECTOR ( 'NONE', #14317, 1000.000000000000227 ) ;
#36723 = ADVANCED_FACE ( 'NONE', ( #32969 ), #26982, .F. ) ;
#36724 = LINE ( 'NONE', #27250, #24374 ) ;
#36725 = ORIENTED_EDGE ( 'NONE', *, *, #26787, .T. ) ;
#36726 = ORIENTED_EDGE ( 'NONE', *, *, #21847, .T. ) ;
#36727 = CARTESIAN_POINT ( 'NONE',  ( 66.27376694608996388, 57.73522568913447373, 4.000000000000000000 ) ) ;
#36728 = CARTESIAN_POINT ( 'NONE',  ( 69.09457860630368486, 59.08023000801873081, -3.976370928559271878 ) ) ;
#36729 = EDGE_LOOP ( 'NONE', ( #26179, #11561, #5352, #7598 ) ) ;
#36730 = CARTESIAN_POINT ( 'NONE',  ( -0.9836270791399484015, -27.32572798912499934, 7.762796336881262249 ) ) ;
#36731 = AXIS2_PLACEMENT_3D ( 'NONE', #20653, #23942, #39808 ) ;
#36733 = EDGE_CURVE ( 'NONE', #22987, #13150, #17974, .T. ) ;
#36732 = CARTESIAN_POINT ( 'NONE',  ( -2.749201978999709084, -28.00803730016500737, 7.695279973900954751 ) ) ;
#36734 = DIRECTION ( 'NONE',  ( 0.000000000000000000, 0.7541618601367546804, 0.6566885781822843215 ) ) ;
#36735 = CARTESIAN_POINT ( 'NONE',  ( 2.950452266830542403, -26.40805720008219382, 6.866852738645442322 ) ) ;
#36736 = DIRECTION ( 'NONE',  ( -0.000000000000000000, -0.000000000000000000, 1.000000000000000000 ) ) ;
#36737 = CONTEXT_DEPENDENT_SHAPE_REPRESENTATION ( #39190, #27246 ) ;
#36738 = DIRECTION ( 'NONE',  ( 0.000000000000000000, 0.000000000000000000, 1.000000000000000000 ) ) ;
#36739 = ORIENTED_EDGE ( 'NONE', *, *, #39881, .F. ) ;
#36740 = CYLINDRICAL_SURFACE ( 'NONE', #26654, 0.1000000000000028644 ) ;
#36741 = VERTEX_POINT ( 'NONE', #17902 ) ;
#36742 = CARTESIAN_POINT ( 'NONE',  ( 78.65807594933866653, 65.42150623161261080, -2.716276829189491426 ) ) ;
#36743 = CARTESIAN_POINT ( 'NONE',  ( 16.70600443586730677, 9.848044269046425825, -2.499999999999896083 ) ) ;
#36744 = CARTESIAN_POINT ( 'NONE',  ( 79.14825301983924533, 66.20254961713403929, -1.551099981298400099 ) ) ;
#36745 = CARTESIAN_POINT ( 'NONE',  ( 79.65304550238739978, 63.88563316389422653, 3.730195463674649936 ) ) ;
#36746 = EDGE_LOOP ( 'NONE', ( #20993, #9382, #25269, #40115 ) ) ;
#36747 = AXIS2_PLACEMENT_3D ( 'NONE', #30919, #11943, #14428 ) ;
#36748 = EDGE_CURVE ( 'NONE', #9255, #8555, #1311, .T. ) ;
#36749 = DIRECTION ( 'NONE',  ( 1.000000000000000000, 0.000000000000000000, -0.000000000000000000 ) ) ;
#36751 = VERTEX_POINT ( 'NONE', #11114 ) ;
#36750 = CARTESIAN_POINT ( 'NONE',  ( -20.87867591359218977, -26.64985754041175525, 6.700000000000000178 ) ) ;
#36752 = CARTESIAN_POINT ( 'NONE',  ( 21.85643539959777115, -1.469530054879572223, 14.38030055974112464 ) ) ;
#36753 = ORIENTED_EDGE ( 'NONE', *, *, #19932, .F. ) ;
#36754 = CARTESIAN_POINT ( 'NONE',  ( -78.60822725968512259, 10.22187107137118289, 6.417182048864131794 ) ) ;
#36755 = CARTESIAN_POINT ( 'NONE',  ( 14.70646227107939907, -5.038312110033563052, 2.499999999999891198 ) ) ;
#36756 = CARTESIAN_POINT ( 'NONE',  ( -75.81783553891371241, 10.25601890356784907, -8.731154437199055707 ) ) ;
#36757 = AXIS2_PLACEMENT_3D ( 'NONE', #14974, #33728, #8781 ) ;
#36758 = CARTESIAN_POINT ( 'NONE',  ( -68.98442902999595105, 21.93515443114010210, -9.800414904976365804 ) ) ;
#36759 = CARTESIAN_POINT ( 'NONE',  ( 33.45683418328554382, -3.835186817697033845, -5.087345507474531736 ) ) ;
#36760 = CARTESIAN_POINT ( 'NONE',  ( 4.904015517545673220, -30.70870076041410002, 7.652160403243385645 ) ) ;
#36761 = CARTESIAN_POINT ( 'NONE',  ( 14.76957396737453365, 12.55251976517217116, 2.511547239741789284 ) ) ;
#36762 = CARTESIAN_POINT ( 'NONE',  ( -1.389564992689783951, -31.21326896663422090, 7.754798119455333705 ) ) ;
#36763 = CARTESIAN_POINT ( 'NONE',  ( 0.6818738419495123937, -26.22140444123891356, 6.980586498568968068 ) ) ;
#36764 = EDGE_CURVE ( 'NONE', #32722, #29003, #36251, .T. ) ;
#36765 = ADVANCED_FACE ( 'NONE', ( #1890 ), #11516, .F. ) ;
#36766 = DIRECTION ( 'NONE',  ( -0.000000000000000000, -0.000000000000000000, 1.000000000000000000 ) ) ;
#36767 = EDGE_CURVE ( 'NONE', #36032, #18940, #26912, .T. ) ;
#36768 = CARTESIAN_POINT ( 'NONE',  ( 3.913290293412392096, -32.15122301917286762, 7.693875151218754205 ) ) ;
#36769 = CARTESIAN_POINT ( 'NONE',  ( 87.03857031557907931, 0.5918713184910167069, 4.894172095624758079 ) ) ;
#36770 = CARTESIAN_POINT ( 'NONE',  ( 4.215805345278602623, -31.85745850766918252, 6.865312560952603782 ) ) ;
#36771 = ORIENTED_EDGE ( 'NONE', *, *, #33408, .T. ) ;
#36772 = CARTESIAN_POINT ( 'NONE',  ( 67.74957807481123950, 58.23899230517488235, 3.997461085607396214 ) ) ;
#36773 = CARTESIAN_POINT ( 'NONE',  ( 36.92993436146343811, -2.615930867933358162, 5.970207429580749903 ) ) ;
#36774 = AXIS2_PLACEMENT_3D ( 'NONE', #37164, #28516, #5884 ) ;
#36775 = CARTESIAN_POINT ( 'NONE',  ( -36.34874870218064302, -26.64985754041175525, 6.700000000000000178 ) ) ;
#36776 = CARTESIAN_POINT ( 'NONE',  ( 84.80723110164849743, 2.854080505324299466, 2.680610459220619912 ) ) ;
#36778 = CARTESIAN_POINT ( 'NONE',  ( -8.978675913592192970, -26.64985754041175525, 6.800000000000000711 ) ) ;
#36777 = CARTESIAN_POINT ( 'NONE',  ( -71.90214061647091626, -21.04549931135898078, 5.920672442023850124 ) ) ;
#36779 =( BOUNDED_CURVE ( )  B_SPLINE_CURVE ( 3, ( #29267, #36055, #19986, #39319 ),
 .UNSPECIFIED., .F., .T. ) 
 B_SPLINE_CURVE_WITH_KNOTS ( ( 4, 4 ),
 ( 1.381924640371166912, 1.574767692156074483 ),
 .UNSPECIFIED. ) 
 CURVE ( )  GEOMETRIC_REPRESENTATION_ITEM ( )  RATIONAL_B_SPLINE_CURVE ( ( 1.000000000000000000, 0.9969033633783033199, 0.9969033633783033199, 1.000000000000000000 ) ) 
 REPRESENTATION_ITEM ( '' )  );
#36780 = CARTESIAN_POINT ( 'NONE',  ( -42.34874870218063592, -25.49307895267003587, 6.800000000000000711 ) ) ;
#36781 = CARTESIAN_POINT ( 'NONE',  ( 86.46043323462474461, 1.241262327860113590, 4.894917242394325463 ) ) ;
#36782 = CARTESIAN_POINT ( 'NONE',  ( -70.31369189463936209, -21.58244653382578448, 5.969151678864092148 ) ) ;
#36783 = ORIENTED_EDGE ( 'NONE', *, *, #19932, .T. ) ;
#36784 = CARTESIAN_POINT ( 'NONE',  ( -69.98161893566610559, -21.12393755324485412, 3.925045345733725988 ) ) ;
#36785 = CIRCLE ( 'NONE', #35493, 1.000000000000000000 ) ;
#36786 = ORIENTED_EDGE ( 'NONE', *, *, #3623, .F. ) ;
#36787 = CARTESIAN_POINT ( 'NONE',  ( 78.69071029820845808, 65.87362605733925136, -2.012706562768929786 ) ) ;
#36788 = LINE ( 'NONE', #27113, #1670 ) ;
#36789 = CARTESIAN_POINT ( 'NONE',  ( 79.79930721375697544, 64.34646279424478621, 3.632888195267895970 ) ) ;
#36790 = CARTESIAN_POINT ( 'NONE',  ( 22.39383066815476298, 0.3445199978907897975, 6.891788138977129385 ) ) ;
#36792 = ORIENTED_EDGE ( 'NONE', *, *, #5758, .T. ) ;
#36791 = CARTESIAN_POINT ( 'NONE',  ( 4.725321061085611341, -27.80929984067426375, 7.756742906098588186 ) ) ;
#36793 = EDGE_CURVE ( 'NONE', #12012, #37904, #24070, .T. ) ;
#36794 = CARTESIAN_POINT ( 'NONE',  ( 73.74018914705078487, 60.85874216252894087, -3.935025356190109402 ) ) ;
#36795 = CARTESIAN_POINT ( 'NONE',  ( 3.214877922168270619, -32.61399439622474716, 6.949473656533219135 ) ) ;
#36797 = CARTESIAN_POINT ( 'NONE',  ( -5.078675913592192614, -26.64985754041175525, 6.700000000000000178 ) ) ;
#36796 = CARTESIAN_POINT ( 'NONE',  ( 4.933350524036014484, -30.91084454984529373, 6.880828092187094569 ) ) ;
#36798 = DIRECTION ( 'NONE',  ( -0.000000000000000000, -0.000000000000000000, 1.000000000000000000 ) ) ;
#36799 = CARTESIAN_POINT ( 'NONE',  ( 78.69038500580381879, 66.05859403932473128, 1.000000000000000000 ) ) ;
#36800 = CARTESIAN_POINT ( 'NONE',  ( 24.02597498973994306, 3.319991383958946329, -3.315850951064452268 ) ) ;
#36801 = ORIENTED_EDGE ( 'NONE', *, *, #15777, .T. ) ;
#36802 = FACE_OUTER_BOUND ( 'NONE', #25699, .T. ) ;
#36803 = ADVANCED_FACE ( 'NONE', ( #14010 ), #22183, .T. ) ;
#36804 = AXIS2_PLACEMENT_3D ( 'NONE', #21435, #21843, #40349 ) ;
#36805 = CARTESIAN_POINT ( 'NONE',  ( 25.51884215448320958, -4.718317418738882552, 0.4603789867971156413 ) ) ;
#36806 = ADVANCED_FACE ( 'NONE', ( #12915 ), #21019, .T. ) ;
#36807 = CARTESIAN_POINT ( 'NONE',  ( -71.92837670882107659, -20.78299143688747819, 3.916079783099621014 ) ) ;
#36808 = CARTESIAN_POINT ( 'NONE',  ( 1.104723037367069338, -33.01887311167336492, 7.756742906098588186 ) ) ;
#36809 = CARTESIAN_POINT ( 'NONE',  ( 78.68070521837705655, 66.05171761244719164, 1.104694797982982646 ) ) ;
#36810 = CARTESIAN_POINT ( 'NONE',  ( 85.73014479007146349, 1.298542115207370173, 5.666065989068760800 ) ) ;
#36811 = CARTESIAN_POINT ( 'NONE',  ( 16.14955235345561846, 10.48078119528741681, 2.684236915963923220 ) ) ;
#36812 = VERTEX_POINT ( 'NONE', #30490 ) ;
#36813 = DIRECTION ( 'NONE',  ( 1.000000000000000000, 0.000000000000000000, -0.000000000000000000 ) ) ;
#36814 = EDGE_CURVE ( 'NONE', #22023, #24696, #20900, .T. ) ;
#36815 = DIRECTION ( 'NONE',  ( -0.1303762246624229071, 0.7394003126383915658, -0.6605219282605403475 ) ) ;
#36816 = VECTOR ( 'NONE', #36766, 1000.000000000000000 ) ;
#36817 = CARTESIAN_POINT ( 'NONE',  ( 28.89703635215781574, -3.425538172464888564, -4.559836211139066009 ) ) ;
#36818 = CARTESIAN_POINT ( 'NONE',  ( -67.80647484265035985, 37.44505118619480299, -9.800414904974669383 ) ) ;
#36819 = CARTESIAN_POINT ( 'NONE',  ( -69.92837670882107659, -20.78299143688747819, 38.00000000000000711 ) ) ;
#36820 = CARTESIAN_POINT ( 'NONE',  ( -0.4384946125261977024, -26.92698254572272631, 7.785172627573962778 ) ) ;
#36821 = ORIENTED_EDGE ( 'NONE', *, *, #21307, .F. ) ;
#36822 = CARTESIAN_POINT ( 'NONE',  ( 25.29476808408737654, 1.731675346697265860, 4.154258334436543798 ) ) ;
#36823 = ADVANCED_FACE ( 'NONE', ( #33596 ), #27184, .F. ) ;
#36824 = DIRECTION ( 'NONE',  ( 1.000000000000000000, 0.000000000000000000, 0.000000000000000000 ) ) ;
#36825 = CARTESIAN_POINT ( 'NONE',  ( 85.27007178914716690, 2.578332801382848594, -1.917248250713118773 ) ) ;
#36826 = ORIENTED_EDGE ( 'NONE', *, *, #12641, .T. ) ;
#36827 = ORIENTED_EDGE ( 'NONE', *, *, #15484, .F. ) ;
#36829 = CARTESIAN_POINT ( 'NONE',  ( 29.48942925047375141, 1.221239797401782567, 4.218574441359598914 ) ) ;
#36828 = CARTESIAN_POINT ( 'NONE',  ( 79.76270496343316552, 65.40180735727545880, -3.071811904357681478 ) ) ;
#36830 = CARTESIAN_POINT ( 'NONE',  ( 17.26834050228787731, -3.265917822029717144, -2.867547815643560760 ) ) ;
#36831 = CARTESIAN_POINT ( 'NONE',  ( 14.77315594796473874, 13.19392823276514015, -2.499999999999998668 ) ) ;
#36832 = VERTEX_POINT ( 'NONE', #21221 ) ;
#36833 = AXIS2_PLACEMENT_3D ( 'NONE', #12092, #6758, #13531 ) ;
#36834 = CARTESIAN_POINT ( 'NONE',  ( -61.24591834330252027, 10.37661300689600097, 2.500000000000000000 ) ) ;
#36835 = ORIENTED_EDGE ( 'NONE', *, *, #2596, .T. ) ;
#36836 = ORIENTED_EDGE ( 'NONE', *, *, #22375, .T. ) ;
#36837 = CARTESIAN_POINT ( 'NONE',  ( 0.03162470699431464694, -32.53223031769636009, 7.695279973900954751 ) ) ;
#36838 = B_SPLINE_CURVE_WITH_KNOTS ( 'NONE', 3,
 ( #7065, #4594, #10946, #36094, #26017, #32605, #38949, #32805, #7266, #35694 ),
 .UNSPECIFIED., .F., .F.,
 ( 4, 3, 3, 4 ),
 ( 9.697399036122160616E-19, 3.025570593003103526E-05, 6.051145698344126547E-05, 6.468151674593655405E-05 ),
 .UNSPECIFIED. ) ;
#36839 = CARTESIAN_POINT ( 'NONE',  ( 80.15412116699830847, 64.17350884197745131, -3.654032574946330936 ) ) ;
#36840 = CARTESIAN_POINT ( 'NONE',  ( -2.878675913592191993, -26.64985754041175525, 6.800000000000000711 ) ) ;
#36841 = VERTEX_POINT ( 'NONE', #9058 ) ;
#36843 = CARTESIAN_POINT ( 'NONE',  ( 5.076139281392760161, -29.16456933348392511, 7.013842709614101167 ) ) ;
#36842 = CARTESIAN_POINT ( 'NONE',  ( 21.85777359310080570, 3.445828482919746527, 4.744213995278264484 ) ) ;
#36844 = CARTESIAN_POINT ( 'NONE',  ( 81.97757951650689279, 62.12693032551443650, -1.780213741554919071 ) ) ;
#36845 = EDGE_CURVE ( 'NONE', #2129, #11044, #5043, .T. ) ;
#36846 = AXIS2_PLACEMENT_3D ( 'NONE', #11732, #24307, #15043 ) ;
#36847 = CARTESIAN_POINT ( 'NONE',  ( -71.72837670882105954, -31.30579396504363388, 1.385640646055090519 ) ) ;
#36848 = VERTEX_POINT ( 'NONE', #39949 ) ;
#36850 = CARTESIAN_POINT ( 'NONE',  ( 22.15490704303159930, -2.652577471374245377, -3.664207081153456169 ) ) ;
#36849 = CYLINDRICAL_SURFACE ( 'NONE', #18675, 6.000000000000002665 ) ;
#36851 = CARTESIAN_POINT ( 'NONE',  ( -1.794870900927445057, -29.38781717045270270, 6.912143950357346966 ) ) ;
#36852 = CARTESIAN_POINT ( 'NONE',  ( 74.30428547378053850, 61.12304205247700395, 3.924711207976832927 ) ) ;
#36853 = CARTESIAN_POINT ( 'NONE',  ( 22.03798447844329189, 3.618149687637631562, -4.432112028060099185 ) ) ;
#36854 = ORIENTED_EDGE ( 'NONE', *, *, #5099, .T. ) ;
#36855 = CARTESIAN_POINT ( 'NONE',  ( 0.5064072726788814149, -26.38646991025836286, 7.670860738520330457 ) ) ;
#36856 = CARTESIAN_POINT ( 'NONE',  ( 21.85643539959779247, -15.31483402087699197, 0.9306824932977513232 ) ) ;
#36857 = LINE ( 'NONE', #8433, #9161 ) ;
#36858 = VERTEX_POINT ( 'NONE', #27791 ) ;
#36859 = CARTESIAN_POINT ( 'NONE',  ( 80.51660522894113114, 65.82269567859336235, 2.502189764415794659 ) ) ;
#36860 = CARTESIAN_POINT ( 'NONE',  ( 86.31714526353648864, 1.402210177843808081, 5.108895447378689170 ) ) ;
#36861 = CARTESIAN_POINT ( 'NONE',  ( -62.92837670882107659, -49.49506129533733656, -6.000000000000000000 ) ) ;
#36862 = CARTESIAN_POINT ( 'NONE',  ( -40.44874870218063734, -26.64985754041175525, 6.700000000000000178 ) ) ;
#36863 = EDGE_CURVE ( 'NONE', #33979, #28588, #1103, .T. ) ;
#36864 = VECTOR ( 'NONE', #16966, 1000.000000000000000 ) ;
#36865 = EDGE_CURVE ( 'NONE', #24116, #26557, #4390, .T. ) ;
#36866 = PLANE ( 'NONE',  #8366 ) ;
#36867 = CARTESIAN_POINT ( 'NONE',  ( 21.53366635609027213, -3.014980951220062266, 3.494836103679133998 ) ) ;
#36868 = CARTESIAN_POINT ( 'NONE',  ( 1.067812944203182068, -26.12756469803955994, 7.651421919295144924 ) ) ;
#36869 = ADVANCED_FACE ( 'NONE', ( #16007 ), #34975, .T. ) ;
#36870 = CARTESIAN_POINT ( 'NONE',  ( 36.19480630455252168, -2.230552841105437611, -5.855472917160542856 ) ) ;
#36871 = LINE ( 'NONE', #17303, #25298 ) ;
#36872 = CARTESIAN_POINT ( 'NONE',  ( 4.683157593253919337, -31.40110544287195182, 6.863805608295730387 ) ) ;
#36873 = DIRECTION ( 'NONE',  ( -0.000000000000000000, -0.000000000000000000, 1.000000000000000000 ) ) ;
#36874 = CARTESIAN_POINT ( 'NONE',  ( -28.87867591359218977, -24.55319635012989110, 6.800000000000000711 ) ) ;
#36875 = CARTESIAN_POINT ( 'NONE',  ( -70.53399048836877228, -45.65663887815897937, 5.989775712723940160 ) ) ;
#36876 = CIRCLE ( 'NONE', #26369, 2.999999999999998668 ) ;
#36877 = ORIENTED_EDGE ( 'NONE', *, *, #31498, .T. ) ;
#36878 = CARTESIAN_POINT ( 'NONE',  ( 36.07741663790258002, -1.633014503204270218, 5.715722609253349518 ) ) ;
#36879 = CARTESIAN_POINT ( 'NONE',  ( -71.92837670882107659, -0.7829914368874768549, 5.928123921495646265 ) ) ;
#36880 = DIRECTION ( 'NONE',  ( -1.000000000000000000, 5.204170427930426016E-15, 0.000000000000000000 ) ) ;
#36881 = CARTESIAN_POINT ( 'NONE',  ( -0.6411629333918610341, -32.17099039281331585, 7.754798119455333705 ) ) ;
#36882 = EDGE_LOOP ( 'NONE', ( #10515, #34497, #3917, #18831, #20150 ) ) ;
#36883 = B_SPLINE_CURVE_WITH_KNOTS ( 'NONE', 3,
 ( #19711, #32286, #13528, #39022, #35577, #7346, #4087, #26099, #32679, #38636 ),
 .UNSPECIFIED., .F., .F.,
 ( 4, 3, 3, 4 ),
 ( 0.0001585009270395771057, 0.0001815657551981834624, 0.0002118214035944139149, 0.0002170292169044812859 ),
 .UNSPECIFIED. ) ;
#36884 = LINE ( 'NONE', #21454, #39046 ) ;
#36885 = CARTESIAN_POINT ( 'NONE',  ( -72.37610296055093784, -1.106069955589489284, -9.901772949365062360 ) ) ;
#36886 = CARTESIAN_POINT ( 'NONE',  ( -71.80155306977633245, -21.28742820676846037, 5.936342406970499752 ) ) ;
#36887 = DIRECTION ( 'NONE',  ( 1.000000000000000000, 0.000000000000000000, 0.000000000000000000 ) ) ;
#36888 = CARTESIAN_POINT ( 'NONE',  ( -1.476689534549258553, -28.35907466968827251, 6.892063359921935195 ) ) ;
#36889 = ORIENTED_EDGE ( 'NONE', *, *, #34161, .T. ) ;
#36890 = DIRECTION ( 'NONE',  ( -0.000000000000000000, -1.000000000000000000, -0.000000000000000000 ) ) ;
#36891 = CARTESIAN_POINT ( 'NONE',  ( -1.650274565467498622, -28.99282850696639713, 7.635761828346577573 ) ) ;
#36892 = ORIENTED_EDGE ( 'NONE', *, *, #628, .F. ) ;
#36893 = CARTESIAN_POINT ( 'NONE',  ( 23.14097115081952438, 4.021047326275176026, 3.125729442354085119 ) ) ;
#36894 = AXIS2_PLACEMENT_3D ( 'NONE', #6104, #30823, #4921 ) ;
#36895 = CARTESIAN_POINT ( 'NONE',  ( 81.34501148009302085, 65.92776879248947353, -1.287552078898777541 ) ) ;
#36896 = CARTESIAN_POINT ( 'NONE',  ( 79.95371652093496095, 64.44169929929478258, 3.600689860192761493 ) ) ;
#36897 = DIRECTION ( 'NONE',  ( 0.000000000000000000, 0.000000000000000000, 1.000000000000000000 ) ) ;
#36898 = ORIENTED_EDGE ( 'NONE', *, *, #35312, .T. ) ;
#36899 = CARTESIAN_POINT ( 'NONE',  ( 77.99575034756949776, 63.53025565730433044, -3.710351296122899711 ) ) ;
#36900 =( BOUNDED_CURVE ( )  B_SPLINE_CURVE ( 3, ( #34513, #6290, #33900, #5674 ),
 .UNSPECIFIED., .F., .T. ) 
 B_SPLINE_CURVE_WITH_KNOTS ( ( 4, 4 ),
 ( 4.708531083176466403, 4.895802057644187855 ),
 .UNSPECIFIED. ) 
 CURVE ( )  GEOMETRIC_REPRESENTATION_ITEM ( )  RATIONAL_B_SPLINE_CURVE ( ( 1.000000000000000000, 0.9970795998553221295, 0.9970795998553221295, 1.000000000000000000 ) ) 
 REPRESENTATION_ITEM ( '' )  );
#36902 = CARTESIAN_POINT ( 'NONE',  ( -53.21549048184568420, -30.38627270959228710, -4.152976064860135708 ) ) ;
#36901 = CARTESIAN_POINT ( 'NONE',  ( 24.12183659247549627, 0.4863356266236299463, 5.096531192340497896 ) ) ;
#36903 = CARTESIAN_POINT ( 'NONE',  ( 81.51669253446031860, 62.40826230823314091, -2.731335034813053841 ) ) ;
#36904 = CARTESIAN_POINT ( 'NONE',  ( 77.93772202372291247, 64.31926776197541074, 3.361664161258280270 ) ) ;
#36905 = ORIENTED_EDGE ( 'NONE', *, *, #39641, .F. ) ;
#36906 = VERTEX_POINT ( 'NONE', #8848 ) ;
#36907 = CARTESIAN_POINT ( 'NONE',  ( 35.35377756119452641, -3.785667184757509407, -5.510616941430652282 ) ) ;
#36908 = CARTESIAN_POINT ( 'NONE',  ( 82.56043351944062181, 63.54438683934786525, 1.421283058690022916 ) ) ;
#36910 = CARTESIAN_POINT ( 'NONE',  ( -1.693162313832979882, -29.36062282964724446, 6.939395833800440450 ) ) ;
#36909 = PLANE ( 'NONE',  #24403 ) ;
#36911 = B_SPLINE_CURVE_WITH_KNOTS ( 'NONE', 3,
 ( #4429, #13268, #20057, #4034, #10382, #38783, #38176, #25838, #16955, #38577 ),
 .UNSPECIFIED., .F., .F.,
 ( 4, 2, 2, 2, 4 ),
 ( 0.000000000000000000, 0.2500000000000000000, 0.5000000000000000000, 0.7500000000000000000, 1.000000000000000000 ),
 .UNSPECIFIED. ) ;
#36912 = CARTESIAN_POINT ( 'NONE',  ( 30.36459403182758265, -1.672762201151555939, 6.017704416797944766 ) ) ;
#36913 = CARTESIAN_POINT ( 'NONE',  ( 14.67669714044831153, -4.948475139782464893, -2.499999999999940492 ) ) ;
#36914 = LINE ( 'NONE', #27039, #12790 ) ;
#36915 = CARTESIAN_POINT ( 'NONE',  ( 1.564461960465584056, -33.06730180939113950, 6.870724624169668004 ) ) ;
#36916 = CARTESIAN_POINT ( 'NONE',  ( 26.00522225989622171, 0.8586799828388421707, -4.425729458961279228 ) ) ;
#36917 = ADVANCED_FACE ( 'NONE', ( #6750 ), #31666, .F. ) ;
#36918 = ORIENTED_EDGE ( 'NONE', *, *, #13069, .T. ) ;
#36919 = CARTESIAN_POINT ( 'NONE',  ( 11.65737507970504439, -23.60493063168009442, 6.000000000000000000 ) ) ;
#36920 = CARTESIAN_POINT ( 'NONE',  ( -1.697894189101925688, -29.44521499630638317, 7.082877429276022596 ) ) ;
#36921 = EDGE_CURVE ( 'NONE', #11301, #12509, #14036, .T. ) ;
#36922 = LINE ( 'NONE', #37117, #36101 ) ;
#36923 = CARTESIAN_POINT ( 'NONE',  ( 36.82367268480642508, -2.161198714638147056, -5.895793440235796545 ) ) ;
#36924 = CARTESIAN_POINT ( 'NONE',  ( -26.97867591359219475, -26.64985754041175525, 6.800000000000000711 ) ) ;
#36925 = CARTESIAN_POINT ( 'NONE',  ( 1.142679410947742502, -32.92387906214399607, 7.670860738520326905 ) ) ;
#36926 = CARTESIAN_POINT ( 'NONE',  ( -30.24874870218063450, -25.49307895267003587, 6.700000000000000178 ) ) ;
#36927 = LINE ( 'NONE', #5846, #914 ) ;
#36928 = DIRECTION ( 'NONE',  ( -0.000000000000000000, -0.000000000000000000, 1.000000000000000000 ) ) ;
#36929 = CARTESIAN_POINT ( 'NONE',  ( -75.12005306888337941, 8.050441697125293672, 10.43857059077842564 ) ) ;
#36930 = CARTESIAN_POINT ( 'NONE',  ( 4.905573833743076761, -28.43555934915513816, 7.782167645815905033 ) ) ;
#36931 = DIRECTION ( 'NONE',  ( 0.000000000000000000, 0.000000000000000000, 1.000000000000000000 ) ) ;
#36932 = ORIENTED_EDGE ( 'NONE', *, *, #11134, .F. ) ;
#36933 = CARTESIAN_POINT ( 'NONE',  ( 69.62738871241069205, 59.42086865771531023, -3.954846139149833739 ) ) ;
#36934 = ORIENTED_EDGE ( 'NONE', *, *, #3313, .F. ) ;
#36935 = DIRECTION ( 'NONE',  ( 0.000000000000000000, 1.000000000000000000, 0.000000000000000000 ) ) ;
#36936 = VECTOR ( 'NONE', #8427, 1000.000000000000000 ) ;
#36937 = CARTESIAN_POINT ( 'NONE',  ( 0.1096350232455502172, -26.56499967738685442, 6.863904403958575706 ) ) ;
#36938 = CARTESIAN_POINT ( 'NONE',  ( 2.970096061415592903, -26.41590945512262323, 6.864276522220859711 ) ) ;
#36940 = LINE ( 'NONE', #27671, #9590 ) ;
#36939 = LINE ( 'NONE', #23959, #32071 ) ;
#36941 = EDGE_CURVE ( 'NONE', #7215, #26593, #11931, .T. ) ;
#36942 = ITEM_DEFINED_TRANSFORMATION ( 'NONE', 'NONE', #24168,  #30744 ) ;
#36943 = B_SPLINE_CURVE_WITH_KNOTS ( 'NONE', 3,
 ( #29608, #13959, #10263, #10857, #29216, #1025, #26133, #23436, #36003, #4701, #11253, #30217, #24237, #39887, #20528, #11057, #26923, #2034, #23629, #27536, #40088, #5716, #18256, #23818, #39266 ),
 .UNSPECIFIED., .F., .F.,
 ( 4, 3, 3, 3, 3, 3, 3, 3, 4 ),
 ( 6.468151674593992863E-05, 9.076621574722235184E-05, 0.0001210204262068006228, 0.0001512763324577468178, 0.0001815301820994240866, 0.0002117781465860793522, 0.0002420274594459826344, 0.0002722905548971214806, 0.0002816827545175697926 ),
 .UNSPECIFIED. ) ;
#36944 = CARTESIAN_POINT ( 'NONE',  ( 5.909439403370450705, -28.84147213309200808, 7.635761828346577573 ) ) ;
#36945 = EDGE_LOOP ( 'NONE', ( #13050, #37396, #20989, #11293 ) ) ;
#36946 = CARTESIAN_POINT ( 'NONE',  ( 22.61730376708971235, 4.636646153475214582, 3.020898913531409935 ) ) ;
#36947 = DIRECTION ( 'NONE',  ( 0.000000000000000000, -0.7541618601367544583, 0.6566885781822845436 ) ) ;
#36948 = EDGE_CURVE ( 'NONE', #24169, #12496, #5780, .T. ) ;
#36949 = EDGE_LOOP ( 'NONE', ( #1561, #30937, #23148, #30198, #10942, #4110, #9187, #20422 ) ) ;
#36950 = CARTESIAN_POINT ( 'NONE',  ( 78.96152850399714396, 65.10675657659959370, -3.115013800517339781 ) ) ;
#36951 = CARTESIAN_POINT ( 'NONE',  ( 16.54830220824161913, 9.917958018445570900, -2.500000000000029754 ) ) ;
#36952 = CARTESIAN_POINT ( 'NONE',  ( 81.16644189562721579, 61.30283181452514185, -1.054034669008006908 ) ) ;
#36953 = CARTESIAN_POINT ( 'NONE',  ( 80.07543224467224263, 63.05907417235837187, 3.676305632669317536 ) ) ;
#36954 = VERTEX_POINT ( 'NONE', #38827 ) ;
#36955 = CARTESIAN_POINT ( 'NONE',  ( -8.978675913592192970, -26.64985754041175525, 6.700000000000000178 ) ) ;
#36956 = PLANE ( 'NONE',  #35412 ) ;
#36957 = CARTESIAN_POINT ( 'NONE',  ( 21.85643539959780313, 0.1435845899245215551, -12.62009698158557747 ) ) ;
#36958 = EDGE_LOOP ( 'NONE', ( #22471, #17482, #11633, #37188 ) ) ;
#36959 = CARTESIAN_POINT ( 'NONE',  ( -80.19290758530635799, 10.52933779828717853, 3.784726273488611348 ) ) ;
#36960 = CARTESIAN_POINT ( 'NONE',  ( 36.75962662137767722, -3.428235495735559635, 5.873601727554911278 ) ) ;
#36961 = DIRECTION ( 'NONE',  ( -0.000000000000000000, -0.000000000000000000, 1.000000000000000000 ) ) ;
#36962 = CARTESIAN_POINT ( 'NONE',  ( -76.84822446654321482, 9.441555170962290688, -8.079216459568250741 ) ) ;
#36963 = ADVANCED_FACE ( 'NONE', ( #35572 ), #29573, .F. ) ;
#36964 = CARTESIAN_POINT ( 'NONE',  ( 1.506707068943643479, -32.96441568433041880, 7.006423389747790331 ) ) ;
#36965 = CARTESIAN_POINT ( 'NONE',  ( 36.20134656968558318, -3.653170093647291949, -5.716499845661110690 ) ) ;
#36966 = DIRECTION ( 'NONE',  ( 1.000000000000000000, 0.000000000000000000, 0.000000000000000000 ) ) ;
#36967 = CARTESIAN_POINT ( 'NONE',  ( 14.80429365997629176, 12.91757655414798300, 2.502880492504405030 ) ) ;
#36968 = DIRECTION ( 'NONE',  ( 0.000000000000000000, 0.000000000000000000, 1.000000000000000000 ) ) ;
#36969 = CARTESIAN_POINT ( 'NONE',  ( -1.477562859369297987, -28.36137111117319520, 6.894806418505348589 ) ) ;
#36970 = CARTESIAN_POINT ( 'NONE',  ( 5.046487440160131399, -28.96688155391847630, 7.756377446753163873 ) ) ;
#36971 = TOROIDAL_SURFACE ( 'NONE', #10654, 80.68529983683480111, 3.000000000000000000 ) ;
#36972 = CARTESIAN_POINT ( 'NONE',  ( 17.06903337278474808, 14.51719371156824501, -2.500000000000000444 ) ) ;
#36973 = CARTESIAN_POINT ( 'NONE',  ( -6.248748702180631831, -26.64985754041175525, 6.800000000000000711 ) ) ;
#36974 = CARTESIAN_POINT ( 'NONE',  ( 25.83720352597168102, 2.054051280725787354, -4.175065982317311963 ) ) ;
#36975 = VERTEX_POINT ( 'NONE', #25884 ) ;
#36976 = CARTESIAN_POINT ( 'NONE',  ( 67.21949607617069944, 57.87245792367627928, 3.992323350375291291 ) ) ;
#36977 = CARTESIAN_POINT ( 'NONE',  ( 36.49083949649433833, -2.266323086343007276, 5.901676056353022837 ) ) ;
#36978 = CARTESIAN_POINT ( 'NONE',  ( -1.659482627397846022, -30.09084907119505914, 7.784476445165072533 ) ) ;
#36979 = CARTESIAN_POINT ( 'NONE',  ( 5.401390093233090717, -28.79627056164295595, 7.013842709614101167 ) ) ;
#36980 = CARTESIAN_POINT ( 'NONE',  ( 87.43313723349395161, -0.009410480739497543642, 5.495402557179364322 ) ) ;
#36981 = CARTESIAN_POINT ( 'NONE',  ( 33.55312825858863590, -1.200935527647059020, -5.443175168862945057 ) ) ;
#36982 = ORIENTED_EDGE ( 'NONE', *, *, #20574, .T. ) ;
#36983 = CARTESIAN_POINT ( 'NONE',  ( -37.07867591359219261, -24.55319635012989110, 6.800000000000000711 ) ) ;
#36984 = CARTESIAN_POINT ( 'NONE',  ( -0.5845629148083903992, -32.22116963437284198, 6.880608371227951992 ) ) ;
#36985 = VERTEX_POINT ( 'NONE', #22605 ) ;
#36986 = CARTESIAN_POINT ( 'NONE',  ( -69.94873531773163222, -21.01309677555362398, 3.919500413570160102 ) ) ;
#36987 = ORIENTED_EDGE ( 'NONE', *, *, #28391, .F. ) ;
#36988 = ORIENTED_EDGE ( 'NONE', *, *, #2345, .F. ) ;
#36989 = CARTESIAN_POINT ( 'NONE',  ( 80.86726794284579967, 61.90233618827342355, -2.830664096605172819 ) ) ;
#36990 = B_SPLINE_CURVE_WITH_KNOTS ( 'NONE', 3,
 ( #30662, #21799, #37020, #34376, #33963, #27348 ),
 .UNSPECIFIED., .F., .F.,
 ( 4, 2, 4 ),
 ( 7.235985768044570246E-16, 0.0008525552902386053511, 0.001705110580476487106 ),
 .UNSPECIFIED. ) ;
#36991 = ADVANCED_FACE ( 'NONE', ( #7542 ), #23005, .T. ) ;
#36992 = DIRECTION ( 'NONE',  ( -0.000000000000000000, -1.000000000000000000, -0.000000000000000000 ) ) ;
#36993 = CARTESIAN_POINT ( 'NONE',  ( 78.74908976354480217, 65.92676629176590097, 1.950029235564084029 ) ) ;
#36996 = ORIENTED_EDGE ( 'NONE', *, *, #39984, .T. ) ;
#36995 = CARTESIAN_POINT ( 'NONE',  ( -1.779986342064762805, -29.14226580803136812, 7.134293011406500185 ) ) ;
#36994 = AXIS2_PLACEMENT_3D ( 'NONE', #30990, #22335, #31387 ) ;
#36997 = EDGE_CURVE ( 'NONE', #25969, #8273, #29375, .T. ) ;
#36998 = CARTESIAN_POINT ( 'NONE',  ( 73.68135292868622344, 60.99150118422435440, -3.923277237825057551 ) ) ;
#36999 = CARTESIAN_POINT ( 'NONE',  ( 3.357996495870312792, -32.53848892694827555, 6.894806418505347700 ) ) ;
#37001 = DIRECTION ( 'NONE',  ( -0.000000000000000000, -0.000000000000000000, 1.000000000000000000 ) ) ;
#37000 = CARTESIAN_POINT ( 'NONE',  ( 4.948068533112945921, -30.87476149476646015, 6.865482280155367434 ) ) ;
#37002 = PLANE ( 'NONE',  #4726 ) ;
#37003 = CARTESIAN_POINT ( 'NONE',  ( 22.89069174712559374, 4.265217579236236567, -3.147968593956119054 ) ) ;
#37004 = ORIENTED_EDGE ( 'NONE', *, *, #877, .F. ) ;
#37005 = CARTESIAN_POINT ( 'NONE',  ( 3.939786388318850641, -26.88011527646091992, 7.635761828346575797 ) ) ;
#37006 = CARTESIAN_POINT ( 'NONE',  ( -0.9595137531180226720, -31.84477669336278893, 7.720710062488890912 ) ) ;
#37007 = EDGE_CURVE ( 'NONE', #9806, #908, #35961, .T. ) ;
#37008 = CARTESIAN_POINT ( 'NONE',  ( 4.978066369605828712, -28.34239679187065164, 7.670465701733752972 ) ) ;
#37009 = CARTESIAN_POINT ( 'NONE',  ( 81.34308989085656094, 63.28542802927127298, 3.228380831072418466 ) ) ;
#37010 = CARTESIAN_POINT ( 'NONE',  ( 84.65562454054800412, 2.508334066475362167, -3.654169056841765517 ) ) ;
#37011 = CARTESIAN_POINT ( 'NONE',  ( -32.44874870218063734, -26.64985754041175525, 6.700000000000000178 ) ) ;
#37012 = ORIENTED_EDGE ( 'NONE', *, *, #7066, .F. ) ;
#37013 = DIRECTION ( 'NONE',  ( 0.8660254037844404840, -0.4999999999999968359, 0.000000000000000000 ) ) ;
#37014 = B_SPLINE_CURVE_WITH_KNOTS ( 'NONE', 3,
 ( #6295, #3841, #330, #16358, #12870, #34929, #733, #13270, #25841, #16752, #17555, #33238, #1538, #38977, #14276, #23155, #29928, #13883, #20252, #7903, #7298, #14071, #23559, #11177, #17349, #29333, #8089, #29727, #17155, #10386, #13686 ),
 .UNSPECIFIED., .F., .F.,
 ( 4, 3, 3, 3, 3, 3, 3, 3, 3, 3, 4 ),
 ( 2.453269466693398698E-18, 3.077658087705472024E-05, 6.152638666998585908E-05, 9.267501192706446866E-05, 0.0001241882240135159729, 0.0001556618703051619753, 0.0001866161554452215447, 0.0002167966385860964937, 0.0002463805737537774895, 0.0002758761370306528696, 0.0002847094172290100906 ),
 .UNSPECIFIED. ) ;
#37015 = CARTESIAN_POINT ( 'NONE',  ( 4.643443039977110942, -31.27241053648453928, 7.769368695748485543 ) ) ;
#37016 = CARTESIAN_POINT ( 'NONE',  ( 4.085542087826527613, -27.00846887205345936, 6.998987538705435441 ) ) ;
#37017 = CARTESIAN_POINT ( 'NONE',  ( 14.81281001777914064, -4.468420226103234860, -2.515823251450710174 ) ) ;
#37018 = CARTESIAN_POINT ( 'NONE',  ( 4.790345179149528398, -27.92659140015631891, 7.754798119455333705 ) ) ;
#37019 = FACE_OUTER_BOUND ( 'NONE', #6139, .T. ) ;
#37020 = CARTESIAN_POINT ( 'NONE',  ( -62.96427906878896152, 37.71115934643970036, 4.137654479799069307 ) ) ;
#37021 = CARTESIAN_POINT ( 'NONE',  ( -10.24874870218063450, -25.49307895267003587, 6.800000000000000711 ) ) ;
#37022 = CARTESIAN_POINT ( 'NONE',  ( 88.37152744968734908, -0.9053694005015545665, 0.1944390934057901588 ) ) ;
#37023 = ORIENTED_EDGE ( 'NONE', *, *, #8570, .T. ) ;
#37024 = VERTEX_POINT ( 'NONE', #22807 ) ;
#37026 = CARTESIAN_POINT ( 'NONE',  ( 37.21265578649057204, -2.743522425390099162, 6.000894410541715907 ) ) ;
#37025 = CARTESIAN_POINT ( 'NONE',  ( 78.90480995596030311, 66.05426212177786738, -1.786209778413372362 ) ) ;
#37027 = CARTESIAN_POINT ( 'NONE',  ( 17.69217577633630967, -2.919086151025220843, 2.967689935422107794 ) ) ;
#37028 = CARTESIAN_POINT ( 'NONE',  ( -40.34874870218063592, -26.64985754041175525, 6.700000000000000178 ) ) ;
#37029 = FACE_OUTER_BOUND ( 'NONE', #15209, .T. ) ;
#37030 = ORIENTED_EDGE ( 'NONE', *, *, #15251, .F. ) ;
#37031 = CARTESIAN_POINT ( 'NONE',  ( -1.741157480058983076, -30.20692156021776142, 7.660770905198784675 ) ) ;
#37032 = ORIENTED_EDGE ( 'NONE', *, *, #29249, .F. ) ;
#37033 = VECTOR ( 'NONE', #24669, 1000.000000000000000 ) ;
#37034 = ORIENTED_EDGE ( 'NONE', *, *, #31175, .F. ) ;
#37035 = CARTESIAN_POINT ( 'NONE',  ( -52.01549048184568846, -30.38627270959228710, 6.800000000000000711 ) ) ;
#37036 = CARTESIAN_POINT ( 'NONE',  ( 81.11661571137584303, 61.75122346557050435, -2.482170738714639668 ) ) ;
#37037 = CARTESIAN_POINT ( 'NONE',  ( -59.64698295252583193, 26.74637988513382325, -7.056669117542212710 ) ) ;
#37038 = EDGE_CURVE ( 'NONE', #10273, #26136, #15536, .T. ) ;
#37039 = ORIENTED_EDGE ( 'NONE', *, *, #40073, .F. ) ;
#37041 = CARTESIAN_POINT ( 'NONE',  ( 14.74978830686079156, 12.47633826711515681, 2.508459208900589044 ) ) ;
#37040 = CARTESIAN_POINT ( 'NONE',  ( 22.47157634915228996, 2.831433730378157154, 4.675524411331370089 ) ) ;
#37042 = VERTEX_POINT ( 'NONE', #13920 ) ;
#37043 = ADVANCED_FACE ( 'NONE', ( #23396 ), #26491, .F. ) ;
#37044 = CARTESIAN_POINT ( 'NONE',  ( 82.12703758395426235, 64.04502942998703929, -2.474249079299298604 ) ) ;
#37045 = DIRECTION ( 'NONE',  ( -0.000000000000000000, -1.000000000000000000, -0.000000000000000000 ) ) ;
#37046 = ORIENTED_EDGE ( 'NONE', *, *, #32114, .F. ) ;
#37048 = CARTESIAN_POINT ( 'NONE',  ( 85.17069404690863621, 2.689958598217443875, -0.9157604595814767823 ) ) ;
#37047 = CARTESIAN_POINT ( 'NONE',  ( 3.340113934647170435, -32.66206629357650115, 7.750000000000000888 ) ) ;
#37049 = CARTESIAN_POINT ( 'NONE',  ( -1.799411162598936187, -29.53200968670955007, 6.887161170156905321 ) ) ;
#37050 = CARTESIAN_POINT ( 'NONE',  ( 72.75889805100318597, 61.54370698478812329, 3.677837812371882897 ) ) ;
#37051 = CARTESIAN_POINT ( 'NONE',  ( 24.38698540644270807, 2.853369664508251358, -3.808177377505154837 ) ) ;
#37052 = CARTESIAN_POINT ( 'NONE',  ( 0.5038290195879405742, -26.38744034030630914, 7.692469944509198854 ) ) ;
#37053 = CARTESIAN_POINT ( 'NONE',  ( 21.85643539959778892, 9.726370091839324772, -5.619754257929120200 ) ) ;
#37054 = DIRECTION ( 'NONE',  ( -0.1303762246624131926, -0.7394003126383953406, 0.6605219282605379050 ) ) ;
#37055 = EDGE_LOOP ( 'NONE', ( #22449, #16456, #13548, #15953, #6988 ) ) ;
#37056 = CARTESIAN_POINT ( 'NONE',  ( -64.55204904897829010, 36.12561474966002351, 8.218049716822161344 ) ) ;
#37057 = CARTESIAN_POINT ( 'NONE',  ( 81.35720881915661096, 61.41209416231797036, 1.323744132979554511 ) ) ;
#37058 = CARTESIAN_POINT ( 'NONE',  ( 85.75411537215676105, 2.034632074852215311, 4.270953678727185121 ) ) ;
#37059 = CARTESIAN_POINT ( 'NONE',  ( -53.21549048184568420, -30.38627270959228710, 4.000000000000000000 ) ) ;
#37060 = LINE ( 'NONE', #8850, #35397 ) ;
#37061 = CARTESIAN_POINT ( 'NONE',  ( -81.07947155388369254, 30.81399289130168384, -12.49999999999999645 ) ) ;
#37062 = VECTOR ( 'NONE', #9540, 1000.000000000000000 ) ;
#37063 = CARTESIAN_POINT ( 'NONE',  ( -70.92837670882107659, -65.19654454972992141, 6.000000000000002665 ) ) ;
#37064 = CARTESIAN_POINT ( 'NONE',  ( 37.04632708303561373, -2.800829925423356404, -5.988373328750657087 ) ) ;
#37065 = CARTESIAN_POINT ( 'NONE',  ( -0.6769021000928485687, -27.12926683874087530, 7.505001789837627335 ) ) ;
#37066 = CARTESIAN_POINT ( 'NONE',  ( 25.01091298175105848, 3.329590532566609529, -1.936828115965013142 ) ) ;
#37067 = VERTEX_POINT ( 'NONE', #35377 ) ;
#37068 = CARTESIAN_POINT ( 'NONE',  ( -18.34874870218063947, -25.49307895267003587, 6.800000000000000711 ) ) ;
#37069 = CARTESIAN_POINT ( 'NONE',  ( 4.384407265606144577, -31.81413237766177815, 7.762796336881259585 ) ) ;
#37070 = VECTOR ( 'NONE', #37588, 1000.000000000000000 ) ;
#37071 = ORIENTED_EDGE ( 'NONE', *, *, #16621, .T. ) ;
#37072 = CARTESIAN_POINT ( 'NONE',  ( 35.16091957826717618, -1.161011098338289749, 5.517918506450993910 ) ) ;
#37073 = DIRECTION ( 'NONE',  ( 1.047444401652940007E-14, -1.000000000000000000, -0.000000000000000000 ) ) ;
#37074 = CARTESIAN_POINT ( 'NONE',  ( 66.89278707744533392, 57.85779714042387667, -3.998112125421894980 ) ) ;
#37075 = EDGE_CURVE ( 'NONE', #18960, #14346, #30020, .T. ) ;
#37076 = CARTESIAN_POINT ( 'NONE',  ( -71.80181757295153488, -0.2787158081064600723, 9.961909801952202770 ) ) ;
#37077 = CARTESIAN_POINT ( 'NONE',  ( -24.34874870218063592, -26.64985754041175525, 6.700000000000000178 ) ) ;
#37078 = ORIENTED_EDGE ( 'NONE', *, *, #34391, .T. ) ;
#37079 = CARTESIAN_POINT ( 'NONE',  ( 4.417933383020717031, -31.78637517338679075, 7.255881584735162981 ) ) ;
#37080 = EDGE_CURVE ( 'NONE', #4406, #26593, #4271, .T. ) ;
#37081 = DIRECTION ( 'NONE',  ( -0.000000000000000000, -0.000000000000000000, 1.000000000000000000 ) ) ;
#37082 = CARTESIAN_POINT ( 'NONE',  ( 20.58590956074638711, 5.855084980973656705, 3.419327077695344386 ) ) ;
#37083 = DIRECTION ( 'NONE',  ( 1.000000000000000000, 0.000000000000000000, -0.000000000000000000 ) ) ;
#37084 = B_SPLINE_CURVE_WITH_KNOTS ( 'NONE', 3,
 ( #17768, #40409, #12215, #30355, #31174, #24787, #9129, #21704, #2160, #15512 ),
 .UNSPECIFIED., .F., .F.,
 ( 4, 3, 3, 4 ),
 ( 0.000000000000000000, 3.025570593003203137E-05, 6.051145698344047942E-05, 6.468151674593313881E-05 ),
 .UNSPECIFIED. ) ;
#37085 = VERTEX_POINT ( 'NONE', #7742 ) ;
#37086 = CARTESIAN_POINT ( 'NONE',  ( 6.921324086407803833, -26.64985754041175525, 6.700000000000000178 ) ) ;
#37087 = CARTESIAN_POINT ( 'NONE',  ( 5.028764603308605530, -28.48812247857538438, 7.754798119455333705 ) ) ;
#37088 = ORIENTED_EDGE ( 'NONE', *, *, #30204, .T. ) ;
#37089 = CARTESIAN_POINT ( 'NONE',  ( 22.02370413983413044, 5.453436713694586935, 3.173045162501021643 ) ) ;
#37090 = EDGE_CURVE ( 'NONE', #20369, #13284, #4475, .T. ) ;
#37091 = CARTESIAN_POINT ( 'NONE',  ( 82.55792188592127445, 63.20960171500892955, -1.133121492189030244 ) ) ;
#37092 = CARTESIAN_POINT ( 'NONE',  ( 79.62856576210180037, 64.96968976106111882, 3.364061116559610820 ) ) ;
#37093 = CIRCLE ( 'NONE', #971, 3.000000000000002665 ) ;
#37094 = ADVANCED_FACE ( 'NONE', ( #35768 ), #35173, .F. ) ;
#37095 = CARTESIAN_POINT ( 'NONE',  ( -0.1776591873979048719, -32.40417280263461208, 6.969307238440504371 ) ) ;
#37096 = EDGE_LOOP ( 'NONE', ( #12456, #32926, #17385, #12978 ) ) ;
#37097 = CARTESIAN_POINT ( 'NONE',  ( 75.74534653887742763, 63.84344576921726144, -2.970791854430509193 ) ) ;
#37099 = CARTESIAN_POINT ( 'NONE',  ( 14.72162123416106638, -5.034119505677589146, -2.499999999996632916 ) ) ;
#37098 = CARTESIAN_POINT ( 'NONE',  ( 2.325436196043557224, -33.01366662812485941, 7.640616322432100205 ) ) ;
#37100 = DIRECTION ( 'NONE',  ( 0.7541618601367571229, 0.000000000000000000, -0.6566885781822815460 ) ) ;
#37101 = CARTESIAN_POINT ( 'NONE',  ( 80.00444560210259226, 65.54189868874054525, -2.943961322783052559 ) ) ;
#37102 = CARTESIAN_POINT ( 'NONE',  ( 77.32551012344487162, 64.79183443757982275, 2.725046208697037287 ) ) ;
#37103 = VERTEX_POINT ( 'NONE', #10621 ) ;
#37104 = VECTOR ( 'NONE', #16510, 1000.000000000000000 ) ;
#37105 = VERTEX_POINT ( 'NONE', #23196 ) ;
#37106 = CARTESIAN_POINT ( 'NONE',  ( 82.39441792515161467, 64.18328374515915868, 1.882325606868446854 ) ) ;
#37109 = ORIENTED_EDGE ( 'NONE', *, *, #14915, .T. ) ;
#37108 = DIRECTION ( 'NONE',  ( 1.000000000000000000, 0.000000000000000000, -0.000000000000000000 ) ) ;
#37107 = DIRECTION ( 'NONE',  ( -0.000000000000000000, -0.000000000000000000, -1.000000000000000000 ) ) ;
#37110 = CARTESIAN_POINT ( 'NONE',  ( 31.06145916124171436, -2.509195271462365540, -5.777646538787225339 ) ) ;
#37111 = FACE_OUTER_BOUND ( 'NONE', #5772, .T. ) ;
#37112 = CARTESIAN_POINT ( 'NONE',  ( -70.92837670882107659, -60.53509472482660669, 0.000000000000000000 ) ) ;
#37113 = CARTESIAN_POINT ( 'NONE',  ( -62.96789184025029584, 35.54107112332057028, 6.131023528871422101 ) ) ;
#37114 = DIRECTION ( 'NONE',  ( 1.165409145176969993E-16, -1.000000000000000000, 0.000000000000000000 ) ) ;
#37115 = CARTESIAN_POINT ( 'NONE',  ( -2.448748702180640446, -25.49307895267003587, 6.700000000000000178 ) ) ;
#37116 = CARTESIAN_POINT ( 'NONE',  ( 5.200390093233090205, -29.56993018339339940, 7.202408869016171167 ) ) ;
#37117 = CARTESIAN_POINT ( 'NONE',  ( -69.32837670882108227, -34.30579396504363388, 1.870248747537495149E-15 ) ) ;
#37118 = CARTESIAN_POINT ( 'NONE',  ( 2.135230303526129081, -33.04281284647206007, 7.006908160621413195 ) ) ;
#37119 = CARTESIAN_POINT ( 'NONE',  ( 37.06799344668426954, -2.451880675787394992, -5.964061398877268161 ) ) ;
#37120 = CARTESIAN_POINT ( 'NONE',  ( 30.88954940396924087, -3.454941690857903591, -4.920487672143777580 ) ) ;
#37121 = DIRECTION ( 'NONE',  ( 0.4690749385695654472, 0.8831583674551005680, -0.000000000000000000 ) ) ;
#37122 = CARTESIAN_POINT ( 'NONE',  ( -0.08001846698760761711, -26.55660217189416272, 7.710604733652626663 ) ) ;
#37123 = CARTESIAN_POINT ( 'NONE',  ( 0.4174405697466118670, -32.81861354646682827, 7.776484688137385248 ) ) ;
#37124 = CARTESIAN_POINT ( 'NONE',  ( 4.221612433196463066, -25.23005020686840183, 7.635761828346577573 ) ) ;
#37125 = CARTESIAN_POINT ( 'NONE',  ( 4.626733377823518012, -27.83888570657239470, 7.693875151218754205 ) ) ;
#37126 = DIRECTION ( 'NONE',  ( 0.000000000000000000, 0.000000000000000000, 1.000000000000000000 ) ) ;
#37127 =( GEOMETRIC_REPRESENTATION_CONTEXT ( 3 ) GLOBAL_UNCERTAINTY_ASSIGNED_CONTEXT ( ( #30410 ) ) GLOBAL_UNIT_ASSIGNED_CONTEXT ( ( #21229, #14228, #30712 ) ) REPRESENTATION_CONTEXT ( 'NONE', 'WORKASPACE' ) );
#37128 = CARTESIAN_POINT ( 'NONE',  ( 21.33769325710290943, 8.396068077058080448, 2.669439336573398158 ) ) ;
#37129 = CARTESIAN_POINT ( 'NONE',  ( 23.09544648813622914, 1.703250674360487382, -5.094339560058331884 ) ) ;
#37130 = EDGE_LOOP ( 'NONE', ( #38671, #15283, #5961, #35943 ) ) ;
#37131 =( NAMED_UNIT ( * ) SI_UNIT ( $, .STERADIAN. ) SOLID_ANGLE_UNIT ( ) );
#37132 = CARTESIAN_POINT ( 'NONE',  ( 70.57032280423491954, 60.39816359117256184, -3.808711916423200616 ) ) ;
#37133 = VECTOR ( 'NONE', #28337, 1000.000000000000114 ) ;
#37134 = ORIENTED_EDGE ( 'NONE', *, *, #3654, .T. ) ;
#37135 = CARTESIAN_POINT ( 'NONE',  ( -0.7996099067669091287, -29.56993018339339940, -6.000000000000000000 ) ) ;
#37136 = CYLINDRICAL_SURFACE ( 'NONE', #10121, 0.09010775117053149152 ) ;
#37137 = DIRECTION ( 'NONE',  ( -0.3420201433256725987, 0.9396926207859068736, -0.000000000000000000 ) ) ;
#37138 = CARTESIAN_POINT ( 'NONE',  ( -1.416918730809773042, -28.21258232695399926, 6.939395833800441338 ) ) ;
#37139 =( BOUNDED_CURVE ( )  B_SPLINE_CURVE ( 3, ( #28359, #171, #22402, #10019 ),
 .UNSPECIFIED., .F., .T. ) 
 B_SPLINE_CURVE_WITH_KNOTS ( ( 4, 4 ),
 ( 1.381924640371167579, 1.574767692156076260 ),
 .UNSPECIFIED. ) 
 CURVE ( )  GEOMETRIC_REPRESENTATION_ITEM ( )  RATIONAL_B_SPLINE_CURVE ( ( 1.000000000000000000, 0.9969033633783032089, 0.9969033633783032089, 1.000000000000000000 ) ) 
 REPRESENTATION_ITEM ( '' )  );
#37140 = CARTESIAN_POINT ( 'NONE',  ( 1.295029243323604806, -26.19418099523372945, 7.013842709614101167 ) ) ;
#37141 = CONTEXT_DEPENDENT_SHAPE_REPRESENTATION ( #29238, #35209 ) ;
#37142 = CARTESIAN_POINT ( 'NONE',  ( -26.97867591359219475, -24.55319635012989110, 6.800000000000000711 ) ) ;
#37143 = ORIENTED_EDGE ( 'NONE', *, *, #26058, .F. ) ;
#37144 = CARTESIAN_POINT ( 'NONE',  ( 23.14717476177426647, 4.059201937619430822, 3.048413602859032512 ) ) ;
#37145 = EDGE_CURVE ( 'NONE', #6781, #30761, #20290, .T. ) ;
#37146 = SURFACE_SIDE_STYLE ('',( #24387 ) ) ;
#37147 = ADVANCED_FACE ( 'NONE', ( #29177 ), #19900, .T. ) ;
#37148 = ORIENTED_EDGE ( 'NONE', *, *, #24214, .T. ) ;
#37149 = CARTESIAN_POINT ( 'NONE',  ( 78.46701299008461206, 65.82614401021746176, -1.855758959884432402 ) ) ;
#37150 = CARTESIAN_POINT ( 'NONE',  ( 81.77617677873419666, 62.02699640077094045, -2.046910133536480991 ) ) ;
#37151 = CARTESIAN_POINT ( 'NONE',  ( 80.79577214038279465, 61.23497056275884631, 1.884339924308601644 ) ) ;
#37152 = VECTOR ( 'NONE', #26546, 1000.000000000000000 ) ;
#37153 = CIRCLE ( 'NONE', #16122, 12.38600677260393113 ) ;
#37154 = LINE ( 'NONE', #40645, #15570 ) ;
#37155 = VECTOR ( 'NONE', #40012, 1000.000000000000000 ) ;
#37157 = ORIENTED_EDGE ( 'NONE', *, *, #15616, .T. ) ;
#37156 = CARTESIAN_POINT ( 'NONE',  ( -42.83131703149249603, -29.56993018339339940, 6.800000000000000711 ) ) ;
#37158 = CARTESIAN_POINT ( 'NONE',  ( 21.85643539959778892, -9.157157878381195104, -8.039778668638760450 ) ) ;
#37159 = ORIENTED_EDGE ( 'NONE', *, *, #36491, .T. ) ;
#37160 = CARTESIAN_POINT ( 'NONE',  ( -77.38833691583745633, 11.04400030039685277, 7.643251527845681181 ) ) ;
#37161 = CARTESIAN_POINT ( 'NONE',  ( -40.87867591359218977, -26.64985754041175525, 6.700000000000000178 ) ) ;
#37162 = AXIS2_PLACEMENT_3D ( 'NONE', #8315, #35941, #11398 ) ;
#37163 = DIRECTION ( 'NONE',  ( -0.000000000000000000, 0.000000000000000000, 1.000000000000000000 ) ) ;
#37164 = CARTESIAN_POINT ( 'NONE',  ( 1.578585683582352850, -25.86893018339335981, 7.754798119455333705 ) ) ;
#37165 = CARTESIAN_POINT ( 'NONE',  ( 3.419804421016331641, -26.52138713537738468, 7.710604733652623999 ) ) ;
#37166 = CARTESIAN_POINT ( 'NONE',  ( 23.38716521561124750, 3.561324528878642592, -3.087505459527394081 ) ) ;
#37167 = CARTESIAN_POINT ( 'NONE',  ( 4.902191478375081068, -30.71383239352053707, 7.643333865083957512 ) ) ;
#37168 = CARTESIAN_POINT ( 'NONE',  ( 14.78431785254804431, 13.03024247939681679, 2.500601908585387001 ) ) ;
#37169 = CYLINDRICAL_SURFACE ( 'NONE', #29174, 0.1000000000000028644 ) ;
#37170 = DIRECTION ( 'NONE',  ( -0.7126435865141291792, 0.000000000000000000, 0.7015262779114398439 ) ) ;
#37171 = CARTESIAN_POINT ( 'NONE',  ( 5.067139036913483885, -29.09558115474426998, 7.759451378593096749 ) ) ;
#37172 = CARTESIAN_POINT ( 'NONE',  ( 17.27696687802587050, 14.34575037107839890, -2.499999999999999556 ) ) ;
#37173 = CARTESIAN_POINT ( 'NONE',  ( 31.94853774039595251, -3.766211141015790353, -4.792495538025669077 ) ) ;
#37174 = CARTESIAN_POINT ( 'NONE',  ( 24.56779495282315651, 2.976875296945072691, -3.585541128247576648 ) ) ;
#37175 = ORIENTED_EDGE ( 'NONE', *, *, #3392, .T. ) ;
#37176 = CARTESIAN_POINT ( 'NONE',  ( 67.11883677231543288, 58.14904800069622581, 3.997022163556061436 ) ) ;
#37177 = CARTESIAN_POINT ( 'NONE',  ( 36.15903063279257879, -3.359981914139457793, 5.843280261744577153 ) ) ;
#37178 = CARTESIAN_POINT ( 'NONE',  ( 4.949602693582518143, -30.84314527041428278, 7.780491323090173772 ) ) ;
#37179 = CARTESIAN_POINT ( 'NONE',  ( 2.193195751821546580, -33.03421897962276432, 7.761113333117550361 ) ) ;
#37180 = VECTOR ( 'NONE', #5395, 1000.000000000000000 ) ;
#37181 = CARTESIAN_POINT ( 'NONE',  ( 87.54376689718995408, -0.1385995495200708916, -5.388168202639758597 ) ) ;
#37182 = CARTESIAN_POINT ( 'NONE',  ( 29.20850709934801159, 2.242166301403143880, -0.5075834600922535245 ) ) ;
#37183 = CARTESIAN_POINT ( 'NONE',  ( -1.557289549629824466, -30.54335471976638416, 6.911401339314958925 ) ) ;
#37184 = ORIENTED_EDGE ( 'NONE', *, *, #35408, .F. ) ;
#37185 = CARTESIAN_POINT ( 'NONE',  ( 24.50840889722684324, 2.969483997251146867, 3.629079860099836186 ) ) ;
#37186 = AXIS2_PLACEMENT_3D ( 'NONE', #5486, #33086, #39441 ) ;
#37187 = CARTESIAN_POINT ( 'NONE',  ( 0.5834512725888432172, -26.35863018636138122, 6.894806418505347700 ) ) ;
#37188 = ORIENTED_EDGE ( 'NONE', *, *, #17840, .T. ) ;
#37189 = DIRECTION ( 'NONE',  ( -0.000000000000000000, -1.000000000000000000, -0.000000000000000000 ) ) ;
#37190 = ADVANCED_FACE ( 'NONE', ( #584 ), #26093, .F. ) ;
#37191 = VERTEX_POINT ( 'NONE', #6946 ) ;
#37192 = CARTESIAN_POINT ( 'NONE',  ( 78.58771539371637971, 65.98568759316003707, -1.340350474428867678 ) ) ;
#37193 = CARTESIAN_POINT ( 'NONE',  ( -1.521281195261787733, -28.20213550263213165, 6.993830769476428344 ) ) ;
#37194 = CARTESIAN_POINT ( 'NONE',  ( 78.91366476310541600, 65.65666373793331445, 2.561782662428539581 ) ) ;
#37196 = ORIENTED_EDGE ( 'NONE', *, *, #24072, .T. ) ;
#37195 = CARTESIAN_POINT ( 'NONE',  ( 14.61802081865033820, 12.33286846116140190, 2.500000000000000000 ) ) ;
#37197 = DIRECTION ( 'NONE',  ( -0.000000000000000000, -0.000000000000000000, -1.000000000000000000 ) ) ;
#37198 = CARTESIAN_POINT ( 'NONE',  ( 73.64914076101801754, 62.55656703988326939, -3.294766324886513775 ) ) ;
#37199 = DIRECTION ( 'NONE',  ( 1.000000000000000000, 0.000000000000000000, 0.000000000000000000 ) ) ;
#37201 = CARTESIAN_POINT ( 'NONE',  ( -41.07867591359219972, -26.64985754041175525, 6.800000000000000711 ) ) ;
#37200 = CARTESIAN_POINT ( 'NONE',  ( 4.920199257240864377, -30.94209232664453779, 6.980586498568960963 ) ) ;
#37202 = DIRECTION ( 'NONE',  ( 1.000000000000000000, 0.000000000000000000, 0.000000000000000000 ) ) ;
#37203 = DIRECTION ( 'NONE',  ( 1.000000000000000000, 0.000000000000000000, 0.000000000000000000 ) ) ;
#37204 = CARTESIAN_POINT ( 'NONE',  ( 21.73142018617180682, 6.152679399380986069, -3.256810401554945056 ) ) ;
#37205 = ORIENTED_EDGE ( 'NONE', *, *, #18491, .T. ) ;
#37206 = CARTESIAN_POINT ( 'NONE',  ( 2.429106749998194648, -26.14670993789270526, 7.753200566781576875 ) ) ;
#37207 = AXIS2_PLACEMENT_3D ( 'NONE', #4667, #20295, #5268 ) ;
#37208 = AXIS2_PLACEMENT_3D ( 'NONE', #14394, #1663, #32952 ) ;
#37209 = CARTESIAN_POINT ( 'NONE',  ( -40.44874870218063734, -26.64985754041175525, 6.800000000000000711 ) ) ;
#37210 = CARTESIAN_POINT ( 'NONE',  ( 3.504784550580148483, -26.68823612567400971, 7.754798119455333705 ) ) ;
#37211 = CARTESIAN_POINT ( 'NONE',  ( 79.29849762269611801, 65.95036606079995067, 2.316472630215894224 ) ) ;
#37212 = CARTESIAN_POINT ( 'NONE',  ( 86.96369117609759769, -0.5876503451053297633, 5.665127693518188678 ) ) ;
#37213 = CARTESIAN_POINT ( 'NONE',  ( 20.34593195197777149, 6.625392312321536359, 3.270953163479469961 ) ) ;
#37214 = ORIENTED_EDGE ( 'NONE', *, *, #27330, .F. ) ;
#37215 = CARTESIAN_POINT ( 'NONE',  ( 2.880952512028528645, -26.27504388691242454, 7.640616322432101093 ) ) ;
#37216 = CARTESIAN_POINT ( 'NONE',  ( 4.614225597785307720, -31.32194692201518293, 7.785172627573962778 ) ) ;
#37217 = EDGE_CURVE ( 'NONE', #8986, #22388, #35970, .T. ) ;
#37218 = CIRCLE ( 'NONE', #24735, 2.000000000000000000 ) ;
#37219 = ORIENTED_EDGE ( 'NONE', *, *, #30549, .F. ) ;
#37220 = CARTESIAN_POINT ( 'NONE',  ( -70.92837670882107659, -56.35932253828836025, 10.00000000000000888 ) ) ;
#37221 = CARTESIAN_POINT ( 'NONE',  ( 14.91073189335287807, -5.916690698649474278, -2.519298049349560475 ) ) ;
#37222 = CARTESIAN_POINT ( 'NONE',  ( -68.71186372058384961, 37.81212149306785619, -8.800414904976365804 ) ) ;
#37223 = DIRECTION ( 'NONE',  ( 1.000000000000000000, 0.000000000000000000, 0.000000000000000000 ) ) ;
#37224 = DIRECTION ( 'NONE',  ( -0.000000000000000000, -0.000000000000000000, 1.000000000000000000 ) ) ;
#37225 = CARTESIAN_POINT ( 'NONE',  ( 36.64525587059520717, -2.463007710373897652, 5.925776466105311613 ) ) ;
#37226 = EDGE_CURVE ( 'NONE', #14186, #32722, #9601, .T. ) ;
#37227 = ORIENTED_EDGE ( 'NONE', *, *, #4212, .T. ) ;
#37229 = DIRECTION ( 'NONE',  ( -0.000000000000000000, -1.000000000000000000, -0.000000000000000000 ) ) ;
#37228 = CARTESIAN_POINT ( 'NONE',  ( 81.34759249528946157, 61.83023590116508217, -2.361823859647550261 ) ) ;
#37230 = CARTESIAN_POINT ( 'NONE',  ( 35.94200923520244828, 151.3264224549853907, -4.000000000000000000 ) ) ;
#37231 = CARTESIAN_POINT ( 'NONE',  ( 3.481437286441587897, -32.58288071328335178, 7.695279973900954751 ) ) ;
#37232 = CARTESIAN_POINT ( 'NONE',  ( 14.69558838330741857, 12.33286846116280699, -2.500000000000005773 ) ) ;
#37233 = VERTEX_POINT ( 'NONE', #18014 ) ;
#37234 = CYLINDRICAL_SURFACE ( 'NONE', #29951, 0.1000000000000028644 ) ;
#37235 = CARTESIAN_POINT ( 'NONE',  ( -0.4715774662971216613, -26.83452162274424424, 7.776484688137385248 ) ) ;
#37236 = EDGE_LOOP ( 'NONE', ( #37286, #19234, #3251, #13893 ) ) ;
#37237 = VERTEX_POINT ( 'NONE', #7939 ) ;
#37238 = EDGE_CURVE ( 'NONE', #6366, #20740, #16242, .T. ) ;
#37239 = EDGE_CURVE ( 'NONE', #11841, #13011, #13596, .T. ) ;
#37240 = CARTESIAN_POINT ( 'NONE',  ( 79.49612969957790654, 65.22981380272332785, -3.178394274514608320 ) ) ;
#37241 = VECTOR ( 'NONE', #29840, 1000.000000000000000 ) ;
#37242 = CARTESIAN_POINT ( 'NONE',  ( 2.294856720451861953, -26.12078399496891734, 7.635761828346576685 ) ) ;
#37243 = ORIENTED_EDGE ( 'NONE', *, *, #21718, .T. ) ;
#37245 = CARTESIAN_POINT ( 'NONE',  ( 31.44497614105462446, 0.4838685039436804169, 4.609055630922440194 ) ) ;
#37244 = CARTESIAN_POINT ( 'NONE',  ( 24.06991255396462392, 2.373183232073612370, 4.210890719218481237 ) ) ;
#37246 = ORIENTED_EDGE ( 'NONE', *, *, #6289, .F. ) ;
#37247 = AXIS2_PLACEMENT_3D ( 'NONE', #36652, #36449, #7838 ) ;
#37248 = CARTESIAN_POINT ( 'NONE',  ( 81.60288604192454898, 64.55353989381943336, -2.864610283900680621 ) ) ;
#37249 = CARTESIAN_POINT ( 'NONE',  ( -71.92830466161952074, -20.91387172644695980, 3.916091961299410951 ) ) ;
#37250 = VERTEX_POINT ( 'NONE', #11620 ) ;
#37252 = FACE_OUTER_BOUND ( 'NONE', #31739, .T. ) ;
#37251 = LINE ( 'NONE', #18509, #21993 ) ;
#37253 = DIRECTION ( 'NONE',  ( -0.000000000000000000, -0.000000000000000000, 1.000000000000000000 ) ) ;
#37254 = CYLINDRICAL_SURFACE ( 'NONE', #34018, 3.000000000000002665 ) ;
#37255 = CARTESIAN_POINT ( 'NONE',  ( 73.43932658456094487, 59.98824119151031198, 3.894134109119617104 ) ) ;
#37256 = CARTESIAN_POINT ( 'NONE',  ( 23.28996408820413322, 3.028860784884633173, -4.014842745608873997 ) ) ;
#37257 = ORIENTED_EDGE ( 'NONE', *, *, #19496, .T. ) ;
#37258 = ADVANCED_FACE ( 'NONE', ( #23986 ), #40051, .T. ) ;
#37259 = CARTESIAN_POINT ( 'NONE',  ( 21.85643539959773207, -2.491245572580281564, -14.29094192267194607 ) ) ;
#37260 = CARTESIAN_POINT ( 'NONE',  ( 3.501669127342749821, -26.58529237886445173, 7.784725160561910329 ) ) ;
#37261 = ORIENTED_EDGE ( 'NONE', *, *, #16374, .F. ) ;
#37262 = CARTESIAN_POINT ( 'NONE',  ( 78.68665600826857087, 66.05594492867547274, 1.065084354002954425 ) ) ;
#37263 = CARTESIAN_POINT ( 'NONE',  ( 87.56526962053540331, 0.0002576605070852033049, 4.866394609412610706 ) ) ;
#37264 = DIRECTION ( 'NONE',  ( -1.000000000000000000, 0.000000000000000000, 0.000000000000000000 ) ) ;
#37265 = CARTESIAN_POINT ( 'NONE',  ( -0.9267661122611743352, -27.41167846166631961, 7.680992449362110897 ) ) ;
#37266 = ORIENTED_EDGE ( 'NONE', *, *, #5966, .F. ) ;
#37267 = CARTESIAN_POINT ( 'NONE',  ( 33.11504244789421136, -3.652289920775848131, 5.213393308200740428 ) ) ;
#37268 = CARTESIAN_POINT ( 'NONE',  ( 1.079328522417935421, -26.12547340107537863, 7.635761828346579350 ) ) ;
#37269 = CARTESIAN_POINT ( 'NONE',  ( 30.51714320403715419, -0.1346950231246703544, -4.969336275524192104 ) ) ;
#37270 = CARTESIAN_POINT ( 'NONE',  ( 5.144118623760252085, -28.96327807028931289, 7.767720160662276108 ) ) ;
#37271 = PLANE ( 'NONE',  #24617 ) ;
#37272 = ADVANCED_FACE ( 'NONE', ( #8335 ), #22524, .T. ) ;
#37273 = VECTOR ( 'NONE', #27260, 1000.000000000000227 ) ;
#37274 = EDGE_CURVE ( 'NONE', #16705, #1634, #34174, .T. ) ;
#37275 = ORIENTED_EDGE ( 'NONE', *, *, #17140, .F. ) ;
#37276 = AXIS2_PLACEMENT_3D ( 'NONE', #28569, #16204, #6746 ) ;
#37277 = VECTOR ( 'NONE', #40212, 1000.000000000000000 ) ;
#37278 = ADVANCED_FACE ( 'NONE', ( #37422 ), #2876, .F. ) ;
#37279 = CARTESIAN_POINT ( 'NONE',  ( 21.78047233922835346, 5.616103166486084319, -3.473245622192032034 ) ) ;
#37280 = CARTESIAN_POINT ( 'NONE',  ( 5.043330201822981529, -28.53322799357174588, 7.013842709614101167 ) ) ;
#37281 = ORIENTED_EDGE ( 'NONE', *, *, #35411, .F. ) ;
#37282 = CARTESIAN_POINT ( 'NONE',  ( 21.67022320682240988, 4.173608297239179699, 3.080183978364538611 ) ) ;
#37283 = CARTESIAN_POINT ( 'NONE',  ( -71.92133747557326728, -0.6645477131579885510, 3.917265324091090406 ) ) ;
#37284 = CARTESIAN_POINT ( 'NONE',  ( 67.00793363329040631, 57.99808316372624972, -3.999354069328931782 ) ) ;
#37285 = ADVANCED_FACE ( 'NONE', ( #12093 ), #14993, .F. ) ;
#37286 = ORIENTED_EDGE ( 'NONE', *, *, #3997, .F. ) ;
#37287 = CARTESIAN_POINT ( 'NONE',  ( 88.29941837874866906, -0.8243730695201928471, 1.365802595430977151 ) ) ;
#37288 = CARTESIAN_POINT ( 'NONE',  ( -78.41777952335573332, -6.504124592832953411, -6.677813406577614685 ) ) ;
#37289 = FACE_OUTER_BOUND ( 'NONE', #8977, .T. ) ;
#37290 = ORIENTED_EDGE ( 'NONE', *, *, #35035, .F. ) ;
#37291 = DIRECTION ( 'NONE',  ( 1.000000000000000000, -0.000000000000000000, -0.000000000000000000 ) ) ;
#37292 = CARTESIAN_POINT ( 'NONE',  ( -32.97867591359219119, -26.64985754041175525, 6.700000000000000178 ) ) ;
#37293 = ORIENTED_EDGE ( 'NONE', *, *, #35850, .T. ) ;
#37294 = CARTESIAN_POINT ( 'NONE',  ( 24.70642277111918617, 3.001709267698361661, 3.438663434477700065 ) ) ;
#37295 = CARTESIAN_POINT ( 'NONE',  ( 82.52664026313777867, 63.88931701666344765, -1.444831904610020645 ) ) ;
#37296 = CARTESIAN_POINT ( 'NONE',  ( 78.71191388991731230, 66.03048852543453506, 1.560659576774504398 ) ) ;
#37297 = CARTESIAN_POINT ( 'NONE',  ( -0.1776515958430064102, -32.40417910011337455, 6.939395833800439561 ) ) ;
#37298 = ORIENTED_EDGE ( 'NONE', *, *, #25209, .T. ) ;
#37299 = CARTESIAN_POINT ( 'NONE',  ( 77.00710955723606332, 62.69977232050459293, -3.829716617887276353 ) ) ;
#37301 = PLANE ( 'NONE',  #697 ) ;
#37300 = CARTESIAN_POINT ( 'NONE',  ( -12.99139449055068241, 13.37661300689600097, -6.000000000000000000 ) ) ;
#37302 = CARTESIAN_POINT ( 'NONE',  ( 0.6463980014349960390, -26.33742331249164081, 7.761597726988850532 ) ) ;
#37303 = CARTESIAN_POINT ( 'NONE',  ( 80.21610222778852517, 65.32174013293554538, -3.113722587672208331 ) ) ;
#37304 = CARTESIAN_POINT ( 'NONE',  ( 79.04999676712186840, 61.38304106620129375, 3.266768353517085721 ) ) ;
#37305 = AXIS2_PLACEMENT_3D ( 'NONE', #8038, #29483, #16903 ) ;
#37306 = ORIENTED_EDGE ( 'NONE', *, *, #23021, .F. ) ;
#37307 = DIRECTION ( 'NONE',  ( -1.000000000000000000, 0.000000000000000000, 0.000000000000000000 ) ) ;
#37308 = CARTESIAN_POINT ( 'NONE',  ( -58.49108653198740626, 30.52987238301787443, 5.010559264471326379 ) ) ;
#37309 = CARTESIAN_POINT ( 'NONE',  ( 81.45638069295017658, 61.46019730367517298, 1.134074597586613109 ) ) ;
#37311 = CARTESIAN_POINT ( 'NONE',  ( -2.293238129880355913, -32.69087815247542039, 6.954324564059724878 ) ) ;
#37310 = CARTESIAN_POINT ( 'NONE',  ( -64.08758708074094557, 42.98467135106749737, 2.320054399416036084 ) ) ;
#37312 = CARTESIAN_POINT ( 'NONE',  ( 31.90185279284946773, -4.312872639525808793, -3.838359570106229413 ) ) ;
#37313 = CARTESIAN_POINT ( 'NONE',  ( 0.000000000000000000, 10.37661300689600097, 6.000000000000000000 ) ) ;
#37314 = DIRECTION ( 'NONE',  ( 0.000000000000000000, 0.000000000000000000, 1.000000000000000000 ) ) ;
#37315 = CARTESIAN_POINT ( 'NONE',  ( -64.12639773666754195, 35.29406715003009509, 4.430479139283200141 ) ) ;
#37316 = CARTESIAN_POINT ( 'NONE',  ( 21.78989781213234167, 0.2240611524379590713, -8.363397281163468477 ) ) ;
#37317 = ADVANCED_FACE ( 'NONE', ( #18479 ), #37979, .T. ) ;
#37318 = FACE_OUTER_BOUND ( 'NONE', #2454, .T. ) ;
#37319 = DIRECTION ( 'NONE',  ( 0.6662082868431814520, 0.000000000000000000, 0.7457657263118715463 ) ) ;
#37320 = CARTESIAN_POINT ( 'NONE',  ( 79.42168399090624575, 60.69064003064117685, 2.270986553420443421 ) ) ;
#37321 = EDGE_CURVE ( 'NONE', #3549, #16760, #11601, .T. ) ;
#37322 = DIRECTION ( 'NONE',  ( 1.000000000000000000, 0.000000000000000000, -0.000000000000000000 ) ) ;
#37323 = CARTESIAN_POINT ( 'NONE',  ( 36.69958409632433671, -3.382823349610835972, -5.888586716072319760 ) ) ;
#37324 = DIRECTION ( 'NONE',  ( 1.000000000000000000, 0.000000000000000000, 0.000000000000000000 ) ) ;
#37325 = LINE ( 'NONE', #5637, #27523 ) ;
#37326 = DIRECTION ( 'NONE',  ( -1.000000000000000000, 0.000000000000000000, 0.000000000000000000 ) ) ;
#37327 = CARTESIAN_POINT ( 'NONE',  ( -68.98442902999595105, 21.93515443114010210, 9.800414904976365804 ) ) ;
#37328 = LINE ( 'NONE', #34686, #2995 ) ;
#37329 = DIRECTION ( 'NONE',  ( 0.000000000000000000, 0.000000000000000000, 1.000000000000000000 ) ) ;
#37330 = EDGE_CURVE ( 'NONE', #15980, #26363, #29722, .T. ) ;
#37331 = CARTESIAN_POINT ( 'NONE',  ( -64.08758708074091714, 38.27681294191128103, -4.090925416971892936 ) ) ;
#37332 = VECTOR ( 'NONE', #35671, 1000.000000000000000 ) ;
#37333 = CARTESIAN_POINT ( 'NONE',  ( 14.77094618574839302, -5.164039144567283302, -2.500001188512491090 ) ) ;
#37334 = ORIENTED_EDGE ( 'NONE', *, *, #29394, .F. ) ;
#37335 = ORIENTED_EDGE ( 'NONE', *, *, #14362, .T. ) ;
#37336 = DIRECTION ( 'NONE',  ( 0.9848077530122080203, 0.1736481776669307198, -0.000000000000000000 ) ) ;
#37337 = AXIS2_PLACEMENT_3D ( 'NONE', #15788, #28340, #1560 ) ;
#37338 = CARTESIAN_POINT ( 'NONE',  ( 69.01369661159887414, 59.28919897632942337, -3.943722715026729109 ) ) ;
#37339 = ORIENTED_EDGE ( 'NONE', *, *, #2208, .F. ) ;
#37340 = DIRECTION ( 'NONE',  ( -1.000000000000000000, -0.000000000000000000, -0.000000000000000000 ) ) ;
#37341 = CARTESIAN_POINT ( 'NONE',  ( 0.04722595069169110288, -26.59889400027656592, 6.889465824494255486 ) ) ;
#37342 = CARTESIAN_POINT ( 'NONE',  ( -1.420842525589276928, -28.22162052951723155, 6.911401339314954484 ) ) ;
#37343 = CARTESIAN_POINT ( 'NONE',  ( 1.301827788660890217, -26.19337156708387226, 6.903372536218456368 ) ) ;
#37344 = CARTESIAN_POINT ( 'NONE',  ( 5.039647113661429145, -30.20982371162487468, 7.785868773668302545 ) ) ;
#37345 = VERTEX_POINT ( 'NONE', #31271 ) ;
#37346 = CARTESIAN_POINT ( 'NONE',  ( 22.88200939092931208, 4.346293566238504269, 3.037513980216376641 ) ) ;
#37347 = SURFACE_STYLE_FILL_AREA ( #40422 ) ;
#37348 = VERTEX_POINT ( 'NONE', #24460 ) ;
#37349 = ORIENTED_EDGE ( 'NONE', *, *, #19347, .F. ) ;
#37350 = CARTESIAN_POINT ( 'NONE',  ( 79.63188232868596117, 63.19436791590091218, -3.756013696796379531 ) ) ;
#37351 = CARTESIAN_POINT ( 'NONE',  ( -1.677952523657942008, -29.95307700655620664, 6.969307238440509700 ) ) ;
#37352 = CARTESIAN_POINT ( 'NONE',  ( 81.68586513309662678, 63.81782706255989268, -3.019849704269077506 ) ) ;
#37353 = CARTESIAN_POINT ( 'NONE',  ( 79.80332398823145468, 63.27387486779120707, 3.741985197832889742 ) ) ;
#37354 = VERTEX_POINT ( 'NONE', #3091 ) ;
#37355 = CARTESIAN_POINT ( 'NONE',  ( -64.08758708074093136, 38.27681294190824701, 4.090925416972713613 ) ) ;
#37357 = ORIENTED_EDGE ( 'NONE', *, *, #3300, .T. ) ;
#37356 = CARTESIAN_POINT ( 'NONE',  ( 4.620198719170100610, -31.31197426661971761, 6.894806418505346812 ) ) ;
#37358 = CARTESIAN_POINT ( 'NONE',  ( 22.36058758039612471, 3.933412737179332375, -7.046732538784932665 ) ) ;
#37359 = ORIENTED_EDGE ( 'NONE', *, *, #37729, .F. ) ;
#37360 = CARTESIAN_POINT ( 'NONE',  ( -72.84075015605040448, 2.241838945666980720, 9.875564344321709598 ) ) ;
#37361 = CARTESIAN_POINT ( 'NONE',  ( 36.39055874488383324, -3.588954754978076256, 5.770159689808049386 ) ) ;
#37362 = AXIS2_PLACEMENT_3D ( 'NONE', #16554, #37978, #31618 ) ;
#37363 = CARTESIAN_POINT ( 'NONE',  ( -74.03402466285142225, 19.33157623370700406, 8.800414904976364028 ) ) ;
#37364 = ORIENTED_EDGE ( 'NONE', *, *, #36133, .T. ) ;
#37365 = CARTESIAN_POINT ( 'NONE',  ( 1.689233551583659620, -32.96992199003639712, 7.775108481317161591 ) ) ;
#37366 = CARTESIAN_POINT ( 'NONE',  ( 29.51386328998167485, -3.424974278474657297, -4.784120810196317741 ) ) ;
#37367 = CARTESIAN_POINT ( 'NONE',  ( 37.17696383940524640, -2.564559183315724855, -5.980961330593222769 ) ) ;
#37368 = DIRECTION ( 'NONE',  ( -0.000000000000000000, -1.000000000000000000, -0.000000000000000000 ) ) ;
#37369 = CARTESIAN_POINT ( 'NONE',  ( 3.974563734633631995, -27.04245323997484007, 7.759451378593098525 ) ) ;
#37370 = CARTESIAN_POINT ( 'NONE',  ( 4.724705146729046845, -27.80824960587721506, 7.635761828346577573 ) ) ;
#37371 = CARTESIAN_POINT ( 'NONE',  ( 1.021324086407808585, -26.64985754041175525, 6.700000000000000178 ) ) ;
#37372 = CARTESIAN_POINT ( 'NONE',  ( 5.060262813864030207, -29.04901129559175743, 7.784476445165073422 ) ) ;
#37373 = EDGE_CURVE ( 'NONE', #32955, #35192, #9001, .T. ) ;
#37374 = EDGE_CURVE ( 'NONE', #5035, #2507, #22415, .T. ) ;
#37375 = CARTESIAN_POINT ( 'NONE',  ( 16.74143876458001401, 14.78209838809407017, -2.499999999999999556 ) ) ;
#37376 = CARTESIAN_POINT ( 'NONE',  ( 21.83244621861719637, 0.3031599029397021305, -8.132627632833301590 ) ) ;
#37377 = CARTESIAN_POINT ( 'NONE',  ( 36.68199778546589584, -1.920130161400638302, -5.804599519094802318 ) ) ;
#37378 = EDGE_CURVE ( 'NONE', #20345, #15467, #28582, .T. ) ;
#37379 = CIRCLE ( 'NONE', #40024, 1.000000000000000888 ) ;
#37380 = CARTESIAN_POINT ( 'NONE',  ( 26.72282919489819264, 1.562893068380316830, -4.355115922428256070 ) ) ;
#37381 = ORIENTED_EDGE ( 'NONE', *, *, #10372, .F. ) ;
#37382 =( BOUNDED_CURVE ( )  B_SPLINE_CURVE ( 3, ( #9672, #31921, #28408, #631 ),
 .UNSPECIFIED., .F., .F. ) 
 B_SPLINE_CURVE_WITH_KNOTS ( ( 4, 4 ),
 ( 4.708531083176467291, 4.895802057644188743 ),
 .UNSPECIFIED. ) 
 CURVE ( )  GEOMETRIC_REPRESENTATION_ITEM ( )  RATIONAL_B_SPLINE_CURVE ( ( 1.000000000000000000, 0.9970795998553221295, 0.9970795998553221295, 1.000000000000000000 ) ) 
 REPRESENTATION_ITEM ( '' )  );
#37383 = CARTESIAN_POINT ( 'NONE',  ( 67.52644525400921793, 57.94193659033309274, 3.989212576213369221 ) ) ;
#37384 = CARTESIAN_POINT ( 'NONE',  ( 36.66477430105471313, -3.237310495223860496, 5.925263590695005966 ) ) ;
#37385 = CARTESIAN_POINT ( 'NONE',  ( -1.666031540912286335, -30.04659083958180688, 7.761597726988851420 ) ) ;
#37386 = DIRECTION ( 'NONE',  ( 0.000000000000000000, 0.000000000000000000, -1.000000000000000000 ) ) ;
#37387 = CARTESIAN_POINT ( 'NONE',  ( 88.87549651282381546, -1.666836616135117799, 1.222388837546040330 ) ) ;
#37389 = CARTESIAN_POINT ( 'NONE',  ( 22.37955706836635983, 4.044372726829571718, 2.563398534706760046 ) ) ;
#37388 = FACE_OUTER_BOUND ( 'NONE', #25412, .T. ) ;
#37390 = ORIENTED_EDGE ( 'NONE', *, *, #25406, .T. ) ;
#37391 = CARTESIAN_POINT ( 'NONE',  ( 24.49274287821404172, 2.967433299905803512, 3.639746199902306412 ) ) ;
#37392 = CIRCLE ( 'NONE', #24920, 0.1000000000000028644 ) ;
#37393 = ORIENTED_EDGE ( 'NONE', *, *, #34021, .T. ) ;
#37394 = CARTESIAN_POINT ( 'NONE',  ( -70.81922763566456069, -21.77701682883130019, 3.999007124502270916 ) ) ;
#37395 = UNCERTAINTY_MEASURE_WITH_UNIT (LENGTH_MEASURE( 1.000000000000000082E-05 ), #23354, 'distance_accuracy_value', 'NONE');
#37396 = ORIENTED_EDGE ( 'NONE', *, *, #1104, .F. ) ;
#37397 = CARTESIAN_POINT ( 'NONE',  ( 80.95177907874115419, 61.22464621339461388, -1.448968528258131716 ) ) ;
#37398 = CARTESIAN_POINT ( 'NONE',  ( 80.54480326438822146, 62.60292565479354465, 3.426353657592656976 ) ) ;
#37400 = EDGE_LOOP ( 'NONE', ( #5172, #23813, #18604, #28210 ) ) ;
#37399 = CARTESIAN_POINT ( 'NONE',  ( 21.58863023475808873, 7.202558683720228672, -2.923977588977705544 ) ) ;
#37401 = CARTESIAN_POINT ( 'NONE',  ( -58.05693936349092610, 29.90851024391614388, 4.510341912063071668 ) ) ;
#37403 = CARTESIAN_POINT ( 'NONE',  ( -22.44874870218064089, -25.49307895267003587, 6.700000000000000178 ) ) ;
#37402 = CARTESIAN_POINT ( 'NONE',  ( 0.9719320429316903320, -25.36088087325603624, 7.635761828346577573 ) ) ;
#37404 = CARTESIAN_POINT ( 'NONE',  ( -37.07867591359219261, -24.55319635012989110, 6.700000000000000178 ) ) ;
#37405 = CARTESIAN_POINT ( 'NONE',  ( -55.02840665537740961, 31.32676418781088401, 1.332930532353302278 ) ) ;
#37406 = CARTESIAN_POINT ( 'NONE',  ( 21.74132580300875617, 6.055672829483719433, -3.293574973715298615 ) ) ;
#37407 = ORIENTED_EDGE ( 'NONE', *, *, #28772, .T. ) ;
#37408 = CARTESIAN_POINT ( 'NONE',  ( 4.913015741384740842, -30.70456324267604131, 7.257242401810564125 ) ) ;
#37409 = CARTESIAN_POINT ( 'NONE',  ( 24.83717141299267794, -2.182840666565796006, 6.391756413845674167 ) ) ;
#37410 = CARTESIAN_POINT ( 'NONE',  ( -80.78522550881831421, -5.650799850798457591, -4.938740386049992104 ) ) ;
#37411 = CARTESIAN_POINT ( 'NONE',  ( 5.009633645164218052, -30.35025518876119222, 6.903372536218457256 ) ) ;
#37412 = CARTESIAN_POINT ( 'NONE',  ( 81.36421798834848573, 61.51166984027109663, 1.726519205789175171 ) ) ;
#37413 = CARTESIAN_POINT ( 'NONE',  ( 87.52176134051316581, -1.326109120332903846, -4.764847963194966063 ) ) ;
#37414 = LINE ( 'NONE', #2667, #31888 ) ;
#37415 = VERTEX_POINT ( 'NONE', #28987 ) ;
#37416 = CARTESIAN_POINT ( 'NONE',  ( -64.71588209753996068, 34.74121984326603041, -6.231007222294328685 ) ) ;
#37417 = CARTESIAN_POINT ( 'NONE',  ( 3.480514495105446748, -26.67316417380424554, 6.866852738645443210 ) ) ;
#37418 = AXIS2_PLACEMENT_3D ( 'NONE', #36119, #5425, #11376 ) ;
#37419 = CARTESIAN_POINT ( 'NONE',  ( 4.014016674530351381, -26.94369103923406783, 6.865554069792297653 ) ) ;
#37420 = DIRECTION ( 'NONE',  ( -0.000000000000000000, -1.000000000000000000, -0.000000000000000000 ) ) ;
#37421 = EDGE_CURVE ( 'NONE', #18087, #27958, #31882, .T. ) ;
#37422 = FACE_OUTER_BOUND ( 'NONE', #26288, .T. ) ;
#37423 = CARTESIAN_POINT ( 'NONE',  ( -71.72837670882105954, -34.30579396504363388, 1.385640646055090519 ) ) ;
#37424 = CARTESIAN_POINT ( 'NONE',  ( 1.873241870000961873, -26.17432681090300051, 6.882085323592685100 ) ) ;
#37425 = CARTESIAN_POINT ( 'NONE',  ( 36.64566332290064565, -2.462282481428397674, 5.925840058891846063 ) ) ;
#37426 = CARTESIAN_POINT ( 'NONE',  ( 4.790345179149528398, -27.92659140015631891, 7.754798119455333705 ) ) ;
#37427 = CIRCLE ( 'NONE', #21012, 31.65266504832700534 ) ;
#37428 = ORIENTED_EDGE ( 'NONE', *, *, #6846, .T. ) ;
#37430 = CARTESIAN_POINT ( 'NONE',  ( -77.92837670882107659, 2.429809908903242999, 15.50000000000000000 ) ) ;
#37429 = CARTESIAN_POINT ( 'NONE',  ( 79.58096101840204994, 65.58481148403340910, -2.850064543546721119 ) ) ;
#37431 = CARTESIAN_POINT ( 'NONE',  ( 21.91440216420213360, -2.652013307545402654, 3.626670478179643275 ) ) ;
#37432 = CARTESIAN_POINT ( 'NONE',  ( -8.978675913592192970, -24.55319635012989110, 6.800000000000000711 ) ) ;
#37433 = ORIENTED_EDGE ( 'NONE', *, *, #9276, .F. ) ;
#37434 = DIRECTION ( 'NONE',  ( 1.000000000000000000, 0.000000000000000000, 0.000000000000000000 ) ) ;
#37435 = EDGE_LOOP ( 'NONE', ( #36836, #17358, #31257, #7139 ) ) ;
#37436 = ORIENTED_EDGE ( 'NONE', *, *, #8216, .F. ) ;
#37437 = CARTESIAN_POINT ( 'NONE',  ( 80.65725571609037559, 62.96675706018874052, -3.489836119548947568 ) ) ;
#37438 = CARTESIAN_POINT ( 'NONE',  ( -1.506684114051581647, -28.44091511309124343, 7.695279973900954751 ) ) ;
#37439 = EDGE_LOOP ( 'NONE', ( #16270, #1756, #36538, #15838 ) ) ;
#37440 = ADVANCED_FACE ( 'NONE', ( #16603 ), #3784, .T. ) ;
#37442 = CARTESIAN_POINT ( 'NONE',  ( 36.06837000820846839, -1.500464606615067753, 5.629282289834582009 ) ) ;
#37441 = CARTESIAN_POINT ( 'NONE',  ( 22.04383411009131422, 3.353668517320957498, 4.622206337531012288 ) ) ;
#37443 = ORIENTED_EDGE ( 'NONE', *, *, #22707, .F. ) ;
#37444 = CARTESIAN_POINT ( 'NONE',  ( 81.76431320972366734, 64.63772642544184066, -2.665107514501070085 ) ) ;
#37445 = AXIS2_PLACEMENT_3D ( 'NONE', #27138, #11477, #14370 ) ;
#37446 = CARTESIAN_POINT ( 'NONE',  ( 4.749272330503722550, -31.28874288805750936, 7.698786668945012401 ) ) ;
#37447 = PRODUCT_DEFINITION_SHAPE ( 'NONE', 'NONE',  #40725 ) ;
#37449 = CARTESIAN_POINT ( 'NONE',  ( 85.59581148158818564, 2.212446518294743480, -3.358098885934541755 ) ) ;
#37448 = LINE ( 'NONE', #12, #25283 ) ;
#37450 = CARTESIAN_POINT ( 'NONE',  ( -14.24874870218063450, -26.64985754041175525, 6.700000000000000178 ) ) ;
#37451 = CARTESIAN_POINT ( 'NONE',  ( 5.144146178010085890, -28.94499496390147186, 7.750000000000002665 ) ) ;
#37452 = CARTESIAN_POINT ( 'NONE',  ( 74.49653936242856389, 60.69398666642196360, 3.911020515999844793 ) ) ;
#37453 = CARTESIAN_POINT ( 'NONE',  ( 24.40178566874492816, 2.839217219712215634, -3.817826656981023081 ) ) ;
#37454 = ORIENTED_EDGE ( 'NONE', *, *, #25205, .F. ) ;
#37455 = EDGE_CURVE ( 'NONE', #11405, #38807, #16925, .T. ) ;
#37456 = CARTESIAN_POINT ( 'NONE',  ( 21.85643539959774628, 6.760345589247273246, -10.71366635798555578 ) ) ;
#37457 = TOROIDAL_SURFACE ( 'NONE', #1986, 3.449999999999999289, 0.05000000000000000278 ) ;
#37458 = CARTESIAN_POINT ( 'NONE',  ( 3.461681733142665252, -26.55548550598080482, 7.778495531946297170 ) ) ;
#37459 = ORIENTED_EDGE ( 'NONE', *, *, #37504, .T. ) ;
#37460 = CARTESIAN_POINT ( 'NONE',  ( 28.84632484126239760, -3.982640415251879062, -4.149463024310225734 ) ) ;
#37461 = CARTESIAN_POINT ( 'NONE',  ( 81.10335266982619373, 65.07249684831462844, 2.967158453528945028 ) ) ;
#37462 = CARTESIAN_POINT ( 'NONE',  ( 87.05115134601746263, 0.5777397079708905814, 5.111878656935144427 ) ) ;
#37463 = ORIENTED_EDGE ( 'NONE', *, *, #793, .T. ) ;
#37464 = DIRECTION ( 'NONE',  ( 0.000000000000000000, 0.7508067542896625923, -0.6605219282605402364 ) ) ;
#37465 = CARTESIAN_POINT ( 'NONE',  ( 15.13412790246976058, -4.097024560658993231, 2.561171989064709997 ) ) ;
#37466 = DIRECTION ( 'NONE',  ( -0.000000000000000000, -1.000000000000000000, -0.000000000000000000 ) ) ;
#37467 = EDGE_CURVE ( 'NONE', #25920, #12896, #31710, .T. ) ;
#37468 = CARTESIAN_POINT ( 'NONE',  ( 34.77288883663810992, -3.165682983332114286, -5.633548307088366514 ) ) ;
#37469 = CARTESIAN_POINT ( 'NONE',  ( 5.147370308016914642, -29.03863631697392833, 7.782861076432729952 ) ) ;
#37470 = CARTESIAN_POINT ( 'NONE',  ( -1.348517286369409263, -27.85116208076715694, 7.695279973900954751 ) ) ;
#37471 = CARTESIAN_POINT ( 'NONE',  ( 3.875507134935765041, -26.95672030760948346, 7.635761828346577573 ) ) ;
#37472 = VECTOR ( 'NONE', #32040, 1000.000000000000000 ) ;
#37473 = CARTESIAN_POINT ( 'NONE',  ( -1.245527615359759421, -31.26744862341078601, 7.769368695748486431 ) ) ;
#37474 = ORIENTED_EDGE ( 'NONE', *, *, #16813, .F. ) ;
#37475 = EDGE_LOOP ( 'NONE', ( #40388, #24876, #20448, #4828 ) ) ;
#37476 = CARTESIAN_POINT ( 'NONE',  ( 32.06782253780797021, 0.2506623542119881254, 4.730668526418615905 ) ) ;
#37477 = DIRECTION ( 'NONE',  ( 0.000000000000000000, 0.000000000000000000, 1.000000000000000000 ) ) ;
#37478 = VERTEX_POINT ( 'NONE', #19516 ) ;
#37479 = CARTESIAN_POINT ( 'NONE',  ( 66.57570644833764106, 57.81776741001107922, -3.999845987728086083 ) ) ;
#37480 = B_SPLINE_CURVE_WITH_KNOTS ( 'NONE', 3,
 ( #53, #34240, #31132, #37684, #9489, #29457, #862, #38706, #13807, #16878, #29054, #16482, #22882, #19177, #23084, #32165, #13198, #35648, #16083, #25766, #1268, #4355, #35451, #6631, #38501, #7418, #9906, #13601, #13395, #25968, #12995 ),
 .UNSPECIFIED., .F., .F.,
 ( 4, 3, 3, 3, 3, 3, 3, 3, 3, 3, 4 ),
 ( 1.226634733346699349E-18, 3.077658087705221980E-05, 6.152638666998412435E-05, 9.267501192705790924E-05, 0.0001241882240135090069, 0.0001556618703051638184, 0.0001866161554452129795, 0.0002167966385860912895, 0.0002463805737537707674, 0.0002758761370306483701, 0.0002847094172289977307 ),
 .UNSPECIFIED. ) ;
#37481 = ADVANCED_FACE ( 'NONE', ( #15818 ), #24102, .T. ) ;
#37482 = ORIENTED_EDGE ( 'NONE', *, *, #20394, .F. ) ;
#37483 = CARTESIAN_POINT ( 'NONE',  ( -56.11355572853776863, 30.33753280151826104, 1.575778306538802465 ) ) ;
#37484 = AXIS2_PLACEMENT_3D ( 'NONE', #22864, #16860, #23265 ) ;
#37485 = DIRECTION ( 'NONE',  ( -0.1736481776669207000, -0.9848077530122097967, -0.000000000000000000 ) ) ;
#37486 = CARTESIAN_POINT ( 'NONE',  ( -68.98442902999595105, 21.93515443114010210, -46.17089178453873188 ) ) ;
#37487 = DIRECTION ( 'NONE',  ( 1.000000000000000000, -0.000000000000000000, 0.000000000000000000 ) ) ;
#37488 = CARTESIAN_POINT ( 'NONE',  ( -28.24874870218063805, -25.49307895267003587, 6.800000000000000711 ) ) ;
#37489 = ORIENTED_EDGE ( 'NONE', *, *, #24795, .F. ) ;
#37490 = CARTESIAN_POINT ( 'NONE',  ( 24.01385423370390626, 3.312006728691793800, 3.343613740752824803 ) ) ;
#37491 = CARTESIAN_POINT ( 'NONE',  ( 82.33093480182111534, 62.53300266214100134, -1.299258709309398352 ) ) ;
#37492 = CARTESIAN_POINT ( 'NONE',  ( 80.99158576241019603, 62.18982880056436358, 2.968223699503258484 ) ) ;
#37493 = CARTESIAN_POINT ( 'NONE',  ( -70.79671605999898532, -21.78301244779445511, 3.999999999923640193 ) ) ;
#37494 = EDGE_LOOP ( 'NONE', ( #32554, #13334, #8571, #36699 ) ) ;
#37495 = CARTESIAN_POINT ( 'NONE',  ( 76.90305707343897268, 64.27659990673319612, -3.054665556626403600 ) ) ;
#37497 = CARTESIAN_POINT ( 'NONE',  ( -78.45330471031414277, 33.71485196875532608, 15.50000000000000000 ) ) ;
#37496 = CARTESIAN_POINT ( 'NONE',  ( 2.357492685323943071, -26.13216693042389238, 6.878641987404677138 ) ) ;
#37498 = CARTESIAN_POINT ( 'NONE',  ( 14.76930820911141495, 12.55346518732212857, -2.511505761737421683 ) ) ;
#37499 = EDGE_CURVE ( 'NONE', #34454, #6217, #2456, .T. ) ;
#37500 = EDGE_CURVE ( 'NONE', #27940, #26477, #32050, .T. ) ;
#37501 = CARTESIAN_POINT ( 'NONE',  ( 79.10630237408686583, 66.00617110148429845, -2.043563575549270706 ) ) ;
#37502 = CARTESIAN_POINT ( 'NONE',  ( 76.90305707343897268, 64.27659990673319612, 3.054665556626398271 ) ) ;
#37503 = EDGE_LOOP ( 'NONE', ( #13589, #32826, #39269, #27720 ) ) ;
#37504 = EDGE_CURVE ( 'NONE', #33375, #18637, #40556, .T. ) ;
#37505 = CIRCLE ( 'NONE', #9921, 3.784187430299790211 ) ;
#37506 = CYLINDRICAL_SURFACE ( 'NONE', #3056, 12.80480339192541628 ) ;
#37507 = CARTESIAN_POINT ( 'NONE',  ( -80.92837670882107659, 2.429809908903242555, 12.50000000000000000 ) ) ;
#37508 = CARTESIAN_POINT ( 'NONE',  ( 82.35700292606965434, 63.80179554273364317, 2.078018481492982517 ) ) ;
#37510 = CARTESIAN_POINT ( 'NONE',  ( -1.693758227496673818, -29.37045797875395081, 6.911401339314954484 ) ) ;
#37509 = CARTESIAN_POINT ( 'NONE',  ( 4.264666792353081881, -31.95205776465687109, 6.903112506833895878 ) ) ;
#37511 = CARTESIAN_POINT ( 'NONE',  ( 29.23504802441905071, -0.3867851007456850065, 5.903809272860179647 ) ) ;
#37512 = CARTESIAN_POINT ( 'NONE',  ( -1.386736143452785397, -31.21906680561900771, 6.865482280155368322 ) ) ;
#37513 = CARTESIAN_POINT ( 'NONE',  ( 1.700390093233090871, -29.56993018339339940, 7.800000000000000711 ) ) ;
#37514 = CARTESIAN_POINT ( 'NONE',  ( -63.15778550246167811, 35.55392038829433687, 6.471101796986872934 ) ) ;
#37515 = CARTESIAN_POINT ( 'NONE',  ( 21.98512429705750648, 0.2333936388226412750, -7.692680552510582359 ) ) ;
#37516 = CARTESIAN_POINT ( 'NONE',  ( -71.92837670882107659, -0.7829914368874778541, 38.00000000000000711 ) ) ;
#37517 = FACE_OUTER_BOUND ( 'NONE', #17457, .T. ) ;
#37518 = CARTESIAN_POINT ( 'NONE',  ( 0.5270352314696233886, -32.86739471733553586, 7.651421919295140484 ) ) ;
#37519 = CARTESIAN_POINT ( 'NONE',  ( 33.45155509882757627, -3.250653912085893715, -5.427322220725915969 ) ) ;
#37520 = EDGE_CURVE ( 'NONE', #4296, #15988, #3712, .T. ) ;
#37521 = CARTESIAN_POINT ( 'NONE',  ( 36.19289006885171034, -3.601804653832907377, -5.745383553838919077 ) ) ;
#37522 = CARTESIAN_POINT ( 'NONE',  ( 79.11842553801511713, 60.58988033035119969, -2.372312511143319647 ) ) ;
#37523 = DIRECTION ( 'NONE',  ( 1.000000000000000000, 0.000000000000000000, 0.000000000000000000 ) ) ;
#37524 = CARTESIAN_POINT ( 'NONE',  ( -0.9362298265465702762, -31.71663383657275048, 7.785868773668303433 ) ) ;
#37525 = CARTESIAN_POINT ( 'NONE',  ( 1.700390093233090871, -29.56993018339339940, 7.800000000000000711 ) ) ;
#37526 = B_SPLINE_CURVE_WITH_KNOTS ( 'NONE', 3,
 ( #27288, #18015, #39853, #40660, #11621, #17806, #34116, #14933, #2817, #20911, #30603, #5888, #21126, #24200, #27897, #21538, #2412, #30812, #33693 ),
 .UNSPECIFIED., .F., .F.,
 ( 4, 3, 3, 3, 3, 3, 4 ),
 ( 0.000000000000000000, 2.546128104244658723E-05, 5.711050680483961836E-05, 8.113074941675755018E-05, 0.0001053129305727055061, 0.0001360598016347104686, 0.0001612931755713720725 ),
 .UNSPECIFIED. ) ;
#37527 = LINE ( 'NONE', #9321, #4916 ) ;
#37528 = CARTESIAN_POINT ( 'NONE',  ( -76.42881101814404587, 9.150640561982111620, 9.834217937602943493 ) ) ;
#37529 = CARTESIAN_POINT ( 'NONE',  ( 86.75210013534866960, -0.2795847087395720298, -5.842668109216860195 ) ) ;
#37530 = CARTESIAN_POINT ( 'NONE',  ( 21.25000211823397933, 8.711688037120479677, 2.624172062053642396 ) ) ;
#37531 = VERTEX_POINT ( 'NONE', #5434 ) ;
#37532 = SURFACE_STYLE_USAGE ( .BOTH. , #24997 ) ;
#37533 = CARTESIAN_POINT ( 'NONE',  ( 69.25747553239096987, 58.65839085985714974, -3.984982412582168010 ) ) ;
#37534 = EDGE_CURVE ( 'NONE', #357, #30063, #14283, .T. ) ;
#37535 = ORIENTED_EDGE ( 'NONE', *, *, #39600, .F. ) ;
#37536 = CARTESIAN_POINT ( 'NONE',  ( -32.87867591359218977, -26.64985754041175525, 6.700000000000000178 ) ) ;
#37537 = CARTESIAN_POINT ( 'NONE',  ( 33.45716606812183613, -3.829385970599605393, -5.093809925484540813 ) ) ;
#37538 = AXIS2_PLACEMENT_3D ( 'NONE', #19941, #36199, #36007 ) ;
#37539 = CARTESIAN_POINT ( 'NONE',  ( 4.888269927152609995, -30.75209629908899345, 7.779495906702014629 ) ) ;
#37540 = ADVANCED_FACE ( 'NONE', ( #27249 ), #21289, .T. ) ;
#37541 = DIRECTION ( 'NONE',  ( 0.8660254037844378194, 0.000000000000000000, -0.5000000000000015543 ) ) ;
#37542 = EDGE_LOOP ( 'NONE', ( #292, #26362, #23388, #10050 ) ) ;
#37543 = CARTESIAN_POINT ( 'NONE',  ( 22.38247687632654959, 4.949581816714125004, 3.033779412410520848 ) ) ;
#37544 = CARTESIAN_POINT ( 'NONE',  ( 3.427626883898521548, -33.95934199490189087, 7.754798119455333705 ) ) ;
#37545 = ADVANCED_FACE ( 'NONE', ( #32686 ), #7752, .T. ) ;
#37546 = AXIS2_PLACEMENT_3D ( 'NONE', #5592, #18132, #30723 ) ;
#37547 = ORIENTED_EDGE ( 'NONE', *, *, #21774, .T. ) ;
#37548 = CARTESIAN_POINT ( 'NONE',  ( 79.95886636011078963, 62.14075979114825543, -3.401284978681017535 ) ) ;
#37550 = CARTESIAN_POINT ( 'NONE',  ( -1.677952468049122681, -29.95308686996596492, 6.939395833800444002 ) ) ;
#37549 = CARTESIAN_POINT ( 'NONE',  ( 25.98038313832403290, 0.8809173887663540592, 4.427613202293294137 ) ) ;
#37551 = CARTESIAN_POINT ( 'NONE',  ( 80.35914242818640219, 65.73759417665644378, -2.670779692148392392 ) ) ;
#37552 = CARTESIAN_POINT ( 'NONE',  ( 78.56734957671525876, 65.55328818492539256, 2.456741006817813933 ) ) ;
#37553 = EDGE_CURVE ( 'NONE', #15769, #32660, #28079, .T. ) ;
#37554 = CARTESIAN_POINT ( 'NONE',  ( 4.412680168184114571, -27.51969055122301100, 6.882085323592682435 ) ) ;
#37555 = CARTESIAN_POINT ( 'NONE',  ( 82.53033050081238287, 64.25366301186838314, 1.000000000000000000 ) ) ;
#37556 = FACE_OUTER_BOUND ( 'NONE', #7673, .T. ) ;
#37557 = CARTESIAN_POINT ( 'NONE',  ( 22.53076953550388950, -1.409035359855524749, -9.122014670555362414 ) ) ;
#37558 = CARTESIAN_POINT ( 'NONE',  ( 21.85643539959776760, -15.11462368761991293, 2.500000000000000000 ) ) ;
#37559 = EDGE_LOOP ( 'NONE', ( #36278, #12752, #4243, #35901, #35307, #33522, #28851, #23490 ) ) ;
#37560 = CARTESIAN_POINT ( 'NONE',  ( -74.02963593684843602, 8.693065175645321219, 9.511771665882234217 ) ) ;
#37561 = CARTESIAN_POINT ( 'NONE',  ( 36.26322319698421381, -3.626588400798672396, 5.736275618128532372 ) ) ;
#37562 = LINE ( 'NONE', #2613, #22835 ) ;
#37563 = ORIENTED_EDGE ( 'NONE', *, *, #29288, .F. ) ;
#37564 = CARTESIAN_POINT ( 'NONE',  ( -72.95330471031414277, 33.71485196875532608, 8.800414904976364028 ) ) ;
#37565 = CARTESIAN_POINT ( 'NONE',  ( 1.626685898479098835, -32.96914518493439772, 6.874555630061442102 ) ) ;
#37566 = CARTESIAN_POINT ( 'NONE',  ( 34.14240489748642204, -3.849676338616116578, -5.233289980769661121 ) ) ;
#37567 = FACE_OUTER_BOUND ( 'NONE', #3629, .T. ) ;
#37568 = DIRECTION ( 'NONE',  ( 0.000000000000000000, 0.000000000000000000, -1.000000000000000000 ) ) ;
#37569 = CARTESIAN_POINT ( 'NONE',  ( -0.07139632246815744154, -26.55151886593404953, 7.651421919295142260 ) ) ;
#37570 = CARTESIAN_POINT ( 'NONE',  ( 4.327908163969745203, -31.72774129374396423, 7.693875151218750652 ) ) ;
#37571 = CARTESIAN_POINT ( 'NONE',  ( 3.481393211524530074, -32.58290676861527402, 7.698786668945011513 ) ) ;
#37572 = CARTESIAN_POINT ( 'NONE',  ( 5.054793046568992310, -30.12489038615697012, 7.695279973900954751 ) ) ;
#37573 = CARTESIAN_POINT ( 'NONE',  ( 27.24896854768403998, 1.198804712641063253, -4.456107267776617142 ) ) ;
#37574 = VECTOR ( 'NONE', #14582, 1000.000000000000000 ) ;
#37575 = CARTESIAN_POINT ( 'NONE',  ( -2.954197855305039422, -12.43481156997016157, 4.000000000000000000 ) ) ;
#37576 = CARTESIAN_POINT ( 'NONE',  ( 24.75839165839662925, 3.019244830385916956, -3.350409272483306111 ) ) ;
#37577 = ORIENTED_EDGE ( 'NONE', *, *, #11562, .F. ) ;
#37578 = CARTESIAN_POINT ( 'NONE',  ( 67.48690106321139126, 58.04989387035797677, 3.996173465816880377 ) ) ;
#37579 = CARTESIAN_POINT ( 'NONE',  ( 25.34282642491231030, 1.862868491491909362, 4.161759000817419007 ) ) ;
#37580 = CARTESIAN_POINT ( 'NONE',  ( -1.648452539126854077, -30.15751253820718603, 7.769368695748486431 ) ) ;
#37581 = EDGE_CURVE ( 'NONE', #35253, #16534, #22734, .T. ) ;
#37582 = CARTESIAN_POINT ( 'NONE',  ( -10.44874870218064089, -25.49307895267003587, 6.700000000000000178 ) ) ;
#37583 = CARTESIAN_POINT ( 'NONE',  ( 87.73660070961769009, -1.594395026316068220, -4.241058185374163791 ) ) ;
#37584 = CARTESIAN_POINT ( 'NONE',  ( 35.84098429011871900, -3.161360823169788059, -5.800250434590431325 ) ) ;
#37585 = ORIENTED_EDGE ( 'NONE', *, *, #30765, .F. ) ;
#37586 = CARTESIAN_POINT ( 'NONE',  ( 25.66089067728524142, 2.145916329718004167, 4.138078528123439348 ) ) ;
#37587 = EDGE_CURVE ( 'NONE', #38497, #24389, #13740, .T. ) ;
#37588 = DIRECTION ( 'NONE',  ( -0.000000000000000000, -0.000000000000000000, 1.000000000000000000 ) ) ;
#37589 = ORIENTED_EDGE ( 'NONE', *, *, #5381, .T. ) ;
#37590 = CARTESIAN_POINT ( 'NONE',  ( 4.037419903619875683, -26.96561723250201226, 7.761113333117551250 ) ) ;
#37591 = EDGE_CURVE ( 'NONE', #8738, #35146, #1135, .T. ) ;
#37592 = EDGE_LOOP ( 'NONE', ( #12489, #33269, #26715, #21201 ) ) ;
#37593 = CARTESIAN_POINT ( 'NONE',  ( 78.52594532581821341, 65.94185624388910583, -1.429680343939077281 ) ) ;
#37594 = CARTESIAN_POINT ( 'NONE',  ( -1.749422520758312505, -28.97934324792513294, 7.750000000000000000 ) ) ;
#37595 = CARTESIAN_POINT ( 'NONE',  ( 80.94504091708289195, 61.55080574620870948, 2.311104455577556394 ) ) ;
#37598 = ORIENTED_EDGE ( 'NONE', *, *, #40257, .F. ) ;
#37597 = ORIENTED_EDGE ( 'NONE', *, *, #14333, .T. ) ;
#37596 = CARTESIAN_POINT ( 'NONE',  ( -0.8497392533635172995, -27.32118824274597202, 6.870716933885663735 ) ) ;
#37599 = EDGE_CURVE ( 'NONE', #17308, #32259, #8545, .T. ) ;
#37601 = EDGE_CURVE ( 'NONE', #14683, #16613, #4419, .T. ) ;
#37600 = CARTESIAN_POINT ( 'NONE',  ( -0.004744360168457827966, -26.52985000677408678, 7.785096263473211486 ) ) ;
#37602 = CARTESIAN_POINT ( 'NONE',  ( -64.08758708074093136, 38.27681294191129524, -4.090925416971890272 ) ) ;
#37603 = CARTESIAN_POINT ( 'NONE',  ( -17.27251170661583402, -8.656638842136340273, 2.500000000000000000 ) ) ;
#37604 = DIRECTION ( 'NONE',  ( -1.385724075720358314E-16, 1.000000000000000000, 0.000000000000000000 ) ) ;
#37605 = CARTESIAN_POINT ( 'NONE',  ( 21.72407540026657102, 6.220878712065926130, -3.231759089253579909 ) ) ;
#37606 = ORIENTED_EDGE ( 'NONE', *, *, #32774, .T. ) ;
#37607 = CARTESIAN_POINT ( 'NONE',  ( -70.92837670882107659, -56.35932253828836025, 0.000000000000000000 ) ) ;
#37608 = CARTESIAN_POINT ( 'NONE',  ( 25.11223377877777807, -2.893972711065841086, 5.714375009671201155 ) ) ;
#37609 = CARTESIAN_POINT ( 'NONE',  ( -76.34937612267491147, -4.253321125015449233, -8.424943696077420441 ) ) ;
#37610 = DIRECTION ( 'NONE',  ( 1.000000000000000000, 0.000000000000000000, -0.000000000000000000 ) ) ;
#37611 = CARTESIAN_POINT ( 'NONE',  ( 80.13372729537762496, 65.27601544180656390, 3.162824939346259523 ) ) ;
#37612 = CARTESIAN_POINT ( 'NONE',  ( 88.23373314635465192, -2.194529332924425091, 2.156499936145213070 ) ) ;
#37613 =( BOUNDED_CURVE ( )  B_SPLINE_CURVE ( 3, ( #15607, #40715, #12514, #25491 ),
 .UNSPECIFIED., .F., .T. ) 
 B_SPLINE_CURVE_WITH_KNOTS ( ( 4, 4 ),
 ( 4.708531083176467291, 4.886921905584129533 ),
 .UNSPECIFIED. ) 
 CURVE ( )  GEOMETRIC_REPRESENTATION_ITEM ( )  RATIONAL_B_SPLINE_CURVE ( ( 1.000000000000000000, 0.9973498172709134302, 0.9973498172709134302, 1.000000000000000000 ) ) 
 REPRESENTATION_ITEM ( '' )  );
#37614 = CARTESIAN_POINT ( 'NONE',  ( -8.978675913592192970, -26.64985754041175525, 6.700000000000000178 ) ) ;
#37615 = ORIENTED_EDGE ( 'NONE', *, *, #23927, .T. ) ;
#37616 = DIRECTION ( 'NONE',  ( -0.000000000000000000, -1.000000000000000000, -0.000000000000000000 ) ) ;
#37617 = CARTESIAN_POINT ( 'NONE',  ( 0.6711941891205337463, 0.5999999999999995337, 3.974981096219152299 ) ) ;
#37618 = CARTESIAN_POINT ( 'NONE',  ( 4.626733377823518012, -27.83888570657239470, 7.703977250142849620 ) ) ;
#37619 = CARTESIAN_POINT ( 'NONE',  ( 85.73057283473386292, 0.7451135881651274051, 5.912605931588609920 ) ) ;
#37620 = ORIENTED_EDGE ( 'NONE', *, *, #10665, .T. ) ;
#37621 = CARTESIAN_POINT ( 'NONE',  ( 36.78910914328132264, -3.040808538379049519, 5.948228248412681829 ) ) ;
#37622 = CARTESIAN_POINT ( 'NONE',  ( 4.252472416081320539, -31.81647455533660107, 7.782034975670476307 ) ) ;
#37623 = CARTESIAN_POINT ( 'NONE',  ( 85.09836244081553502, 2.771204891246429547, 1.045684100250478643 ) ) ;
#37624 = ORIENTED_EDGE ( 'NONE', *, *, #21679, .F. ) ;
#37626 = CARTESIAN_POINT ( 'NONE',  ( 14.76394723472931325, -5.159572269938053068, 2.499999999999999556 ) ) ;
#37625 = CARTESIAN_POINT ( 'NONE',  ( 81.14373266700285114, 62.24431303712577090, -2.911438267503734689 ) ) ;
#37627 = CARTESIAN_POINT ( 'NONE',  ( -70.17231294992166113, -45.80665935166715741, 9.973038756526108273 ) ) ;
#37628 = VECTOR ( 'NONE', #17937, 1000.000000000000000 ) ;
#37629 = DIRECTION ( 'NONE',  ( 0.1303762246624182997, 0.7394003126383944524, 0.6605219282605379050 ) ) ;
#37630 = EDGE_LOOP ( 'NONE', ( #1364, #2894, #8614, #3531 ) ) ;
#37631 = CARTESIAN_POINT ( 'NONE',  ( -1.627575555862121215, -28.87372634162266039, 7.768425012602595991 ) ) ;
#37632 = ORIENTED_EDGE ( 'NONE', *, *, #7949, .F. ) ;
#37633 = CARTESIAN_POINT ( 'NONE',  ( -36.97867591359219119, -26.64985754041175525, 6.700000000000000178 ) ) ;
#37634 = ORIENTED_EDGE ( 'NONE', *, *, #29510, .F. ) ;
#37635 = CARTESIAN_POINT ( 'NONE',  ( 80.74944977059911366, 62.67191958473371471, -3.380189700376618589 ) ) ;
#37636 = CARTESIAN_POINT ( 'NONE',  ( -71.92837670882109080, -0.6506956803064269934, 5.916079783099621459 ) ) ;
#37637 = ORIENTED_EDGE ( 'NONE', *, *, #37834, .T. ) ;
#37639 = CARTESIAN_POINT ( 'NONE',  ( 4.380275065937200729, -27.47751031055269166, 7.757178535559531518 ) ) ;
#37638 = CARTESIAN_POINT ( 'NONE',  ( 23.73424597286967952, 2.447426312426829398, 4.258169151716980849 ) ) ;
#37640 = VERTEX_POINT ( 'NONE', #2575 ) ;
#37641 = ADVANCED_FACE ( 'NONE', ( #27657 ), #367, .T. ) ;
#37643 = EDGE_CURVE ( 'NONE', #14571, #25004, #18585, .T. ) ;
#37642 = CARTESIAN_POINT ( 'NONE',  ( 4.671426276349930795, -27.91676604085201063, 6.889465824494257262 ) ) ;
#37645 = CARTESIAN_POINT ( 'NONE',  ( 86.19938718321334647, 1.534481642798401380, -4.634396957419961716 ) ) ;
#37644 = DIRECTION ( 'NONE',  ( 1.000000000000000000, 0.000000000000000000, 0.000000000000000000 ) ) ;
#37646 = DIRECTION ( 'NONE',  ( -0.000000000000000000, -1.000000000000000000, -0.000000000000000000 ) ) ;
#37647 = CARTESIAN_POINT ( 'NONE',  ( 4.313599969017027469, -31.74504722509605159, 7.635761828346577573 ) ) ;
#37648 = CARTESIAN_POINT ( 'NONE',  ( 73.79885669521775071, 60.72590704978823339, 3.935025356184053802 ) ) ;
#37649 = ORIENTED_EDGE ( 'NONE', *, *, #34604, .T. ) ;
#37650 = AXIS2_PLACEMENT_3D ( 'NONE', #10806, #25872, #7732 ) ;
#37651 = CARTESIAN_POINT ( 'NONE',  ( 22.23015695420303928, 3.514796972574160794, -4.336854520634696009 ) ) ;
#37652 = VERTEX_POINT ( 'NONE', #31173 ) ;
#37653 = CARTESIAN_POINT ( 'NONE',  ( 21.85643539959778181, 2.657715471900086612, -15.25567151318962367 ) ) ;
#37654 = CARTESIAN_POINT ( 'NONE',  ( -58.88301977763249795, 29.11298994408642571, -6.074305062359572460 ) ) ;
#37655 = VERTEX_POINT ( 'NONE', #37721 ) ;
#37656 = CARTESIAN_POINT ( 'NONE',  ( -55.16612787639762416, 31.23053227951969646, -1.484562114140327793 ) ) ;
#37657 = CARTESIAN_POINT ( 'NONE',  ( 81.53193199008826753, 61.58838919619023500, 1.571309534768038141 ) ) ;
#37658 = CARTESIAN_POINT ( 'NONE',  ( 87.46579090913228072, 0.1119968706995537605, 4.710562776971725540 ) ) ;
#37659 = ORIENTED_EDGE ( 'NONE', *, *, #22165, .T. ) ;
#37660 = COLOUR_RGB ( '',0.7921568627450980005, 0.8196078431372548767, 0.9333333333333333481 ) ;
#37661 = CARTESIAN_POINT ( 'NONE',  ( -63.08758708074093136, 38.13199975834322686, 3.043809435734686986 ) ) ;
#37662 = ORIENTED_EDGE ( 'NONE', *, *, #7134, .T. ) ;
#37663 = CARTESIAN_POINT ( 'NONE',  ( 14.65281498853338782, -5.050736788034034142, 2.492857568421119829 ) ) ;
#37664 = CARTESIAN_POINT ( 'NONE',  ( 36.97979765674093500, -2.956942819130029765, -5.977989802757186055 ) ) ;
#37665 = CARTESIAN_POINT ( 'NONE',  ( -71.92837670882106238, -42.87473357531881391, 1.732050807568877637 ) ) ;
#37666 = DIRECTION ( 'NONE',  ( 0.000000000000000000, 0.000000000000000000, 1.000000000000000000 ) ) ;
#37667 = LINE ( 'NONE', #29240, #34082 ) ;
#37668 = CARTESIAN_POINT ( 'NONE',  ( -1.241387487007608925, -31.27463350997279790, 7.763628509615286610 ) ) ;
#37669 = VECTOR ( 'NONE', #23750, 1000.000000000000000 ) ;
#37670 = ORIENTED_EDGE ( 'NONE', *, *, #32608, .T. ) ;
#37671 = ORIENTED_EDGE ( 'NONE', *, *, #28966, .T. ) ;
#37672 = CARTESIAN_POINT ( 'NONE',  ( 30.88164994506820449, 0.6966255426222526248, 4.496776574569896212 ) ) ;
#37673 = LINE ( 'NONE', #9896, #5411 ) ;
#37674 = CARTESIAN_POINT ( 'NONE',  ( 66.56983546066652480, 57.83423415266778278, -3.999917672784519596 ) ) ;
#37675 = AXIS2_PLACEMENT_3D ( 'NONE', #11055, #26921, #5305 ) ;
#37676 = ADVANCED_FACE ( 'NONE', ( #2991 ), #28268, .F. ) ;
#37677 = ORIENTED_EDGE ( 'NONE', *, *, #26429, .T. ) ;
#37678 = CARTESIAN_POINT ( 'NONE',  ( 88.33288515625950765, -0.8619645424494146724, 0.9116167777034707154 ) ) ;
#37679 = CARTESIAN_POINT ( 'NONE',  ( -80.67847586496442602, -6.621814235793498149, -2.260889596539092938 ) ) ;
#37680 = FACE_BOUND ( 'NONE', #36508, .T. ) ;
#37681 =( NAMED_UNIT ( * ) PLANE_ANGLE_UNIT ( ) SI_UNIT ( $, .RADIAN. ) );
#37682 = VERTEX_POINT ( 'NONE', #15916 ) ;
#37683 = FACE_BOUND ( 'NONE', #26870, .T. ) ;
#37684 = CARTESIAN_POINT ( 'NONE',  ( 3.907593953511830254, -32.28622381979772626, 6.875671892026060661 ) ) ;
#37685 = ORIENTED_EDGE ( 'NONE', *, *, #4214, .F. ) ;
#37686 = CARTESIAN_POINT ( 'NONE',  ( 24.30163658516156033, 3.125396681048508096, 3.455688527987379910 ) ) ;
#37687 = CARTESIAN_POINT ( 'NONE',  ( 82.46885687451847957, 64.22182207139027810, -1.617049763656951411 ) ) ;
#37688 = CARTESIAN_POINT ( 'NONE',  ( 81.18585152890854317, 61.61024096112966220, 2.156541836018581293 ) ) ;
#37690 = ADVANCED_FACE ( 'NONE', ( #28477 ), #283, .F. ) ;
#37689 = CARTESIAN_POINT ( 'NONE',  ( 2.865950163328865319, -26.37595621308645022, 7.769368695748489095 ) ) ;
#37691 = ORIENTED_EDGE ( 'NONE', *, *, #30982, .T. ) ;
#37692 = CARTESIAN_POINT ( 'NONE',  ( 76.82516749139865908, 64.42394039557471785, -2.889099817377081880 ) ) ;
#37694 = DIRECTION ( 'NONE',  ( 1.000000000000000000, 0.000000000000000000, 0.000000000000000000 ) ) ;
#37693 = CARTESIAN_POINT ( 'NONE',  ( 3.963477911421234623, -32.23984282750152630, 7.750000000000001776 ) ) ;
#37695 = CARTESIAN_POINT ( 'NONE',  ( 19.31369698277901037, 7.427556948433061912, -3.124657957306991918 ) ) ;
#37696 = CARTESIAN_POINT ( 'NONE',  ( 78.80232334588868071, 66.09893194982532805, -1.428845309148525589 ) ) ;
#37697 = CARTESIAN_POINT ( 'NONE',  ( 77.06776432268850385, 63.96223838934589168, 3.363831406679905101 ) ) ;
#37698 = ORIENTED_EDGE ( 'NONE', *, *, #31451, .T. ) ;
#37699 = CARTESIAN_POINT ( 'NONE',  ( -59.93345510331042902, 24.73247967741478703, 9.800414904976365804 ) ) ;
#37700 = AXIS2_PLACEMENT_3D ( 'NONE', #32814, #32410, #16725 ) ;
#37701 = CARTESIAN_POINT ( 'NONE',  ( -0.8614879664499306422, -31.96464424086259370, 7.139344958878412584 ) ) ;
#37702 = CARTESIAN_POINT ( 'NONE',  ( 82.31416527841567188, 64.14174473599682358, 2.134985007309428973 ) ) ;
#37704 = CARTESIAN_POINT ( 'NONE',  ( -1.694464052375517671, -29.38293999636734810, 7.013842709614101167 ) ) ;
#37703 = CARTESIAN_POINT ( 'NONE',  ( 5.551251297819359110, -25.49307895267003587, 6.700000000000000178 ) ) ;
#37705 = CARTESIAN_POINT ( 'NONE',  ( 29.75157451403313758, 0.8046206704518127362, -4.785270562610461020 ) ) ;
#37706 = CARTESIAN_POINT ( 'NONE',  ( -1.376837950267322030, -31.23749498225474497, 6.863805608295729499 ) ) ;
#37707 = CARTESIAN_POINT ( 'NONE',  ( 20.41865484760615956, -3.555473204735890125, 2.500000000123285826 ) ) ;
#37708 = CARTESIAN_POINT ( 'NONE',  ( -62.87442376950010470, 35.57781650258885975, 5.904453864323423673 ) ) ;
#37709 = VECTOR ( 'NONE', #17316, 1000.000000000000000 ) ;
#37710 = DIRECTION ( 'NONE',  ( 1.000000000000000000, 2.973811673103098158E-15, 0.000000000000000000 ) ) ;
#37711 = DIRECTION ( 'NONE',  ( 1.000000000000000000, 0.000000000000000000, 0.000000000000000000 ) ) ;
#37712 = CARTESIAN_POINT ( 'NONE',  ( 5.660191562250180830, -26.39039255756133429, 7.013842709614101167 ) ) ;
#37713 = LINE ( 'NONE', #21694, #32152 ) ;
#37714 = CARTESIAN_POINT ( 'NONE',  ( 21.70417750497355058, 4.205083950317406227, -2.944929369283658893 ) ) ;
#37715 = CARTESIAN_POINT ( 'NONE',  ( 81.06637268519124007, 61.26626587534826740, -1.317877730053106378 ) ) ;
#37716 = CARTESIAN_POINT ( 'NONE',  ( 1.722902416880312426, -33.06986345199739930, 7.646866513072557048 ) ) ;
#37717 = CARTESIAN_POINT ( 'NONE',  ( -18.97867591359219475, -26.64985754041175525, 6.700000000000000178 ) ) ;
#37718 = DIRECTION ( 'NONE',  ( -0.8660254037844415942, 0.4999999999999950040, -0.000000000000000000 ) ) ;
#37719 = CARTESIAN_POINT ( 'NONE',  ( 1.665003373911284612, -26.17011430565816710, 7.680992449362118890 ) ) ;
#37720 = EDGE_CURVE ( 'NONE', #25870, #36371, #12821, .T. ) ;
#37721 = CARTESIAN_POINT ( 'NONE',  ( 21.85643539959777115, -15.24623503193425123, 0.9260495571226281530 ) ) ;
#37722 = CARTESIAN_POINT ( 'NONE',  ( 21.85643539959776760, -15.11462368761991293, 2.500000000000000000 ) ) ;
#37723 = CARTESIAN_POINT ( 'NONE',  ( -1.541386100576979556, -30.59505803358882403, 6.868387053540521592 ) ) ;
#37724 = ORIENTED_EDGE ( 'NONE', *, *, #37534, .F. ) ;
#37725 = B_SPLINE_CURVE_WITH_KNOTS ( 'NONE', 3,
 ( #28008, #16063, #9683, #18743, #18955, #9266 ),
 .UNSPECIFIED., .F., .F.,
 ( 4, 2, 4 ),
 ( 0.000000000000000000, 0.0004188893554603549240, 0.0008377787109207098480 ),
 .UNSPECIFIED. ) ;
#37726 = EDGE_CURVE ( 'NONE', #23756, #25426, #37934, .T. ) ;
#37727 = CARTESIAN_POINT ( 'NONE',  ( 4.361462012329716309, -31.84340686930758935, 6.894806418505347700 ) ) ;
#37728 = CARTESIAN_POINT ( 'NONE',  ( 68.11537257328342321, 58.15040817571434673, -3.985705108533861729 ) ) ;
#37729 = EDGE_CURVE ( 'NONE', #16251, #4540, #18182, .T. ) ;
#37730 = CIRCLE ( 'NONE', #18010, 0.1000000000000028644 ) ;
#37731 = ORIENTED_EDGE ( 'NONE', *, *, #26107, .T. ) ;
#37732 = CARTESIAN_POINT ( 'NONE',  ( -5.078675913592192614, -26.64985754041175525, 6.700000000000000178 ) ) ;
#37733 = DIRECTION ( 'NONE',  ( 0.000000000000000000, 0.000000000000000000, 1.000000000000000000 ) ) ;
#37734 = CARTESIAN_POINT ( 'NONE',  ( 24.43561622922326038, 2.813159176002239192, 3.833666132760469303 ) ) ;
#37735 = CARTESIAN_POINT ( 'NONE',  ( 5.030206442791328669, -28.49176951078394993, 6.867199677474202346 ) ) ;
#37736 = CARTESIAN_POINT ( 'NONE',  ( 3.549351527779726734, -26.59817285589183200, 6.865482280155369210 ) ) ;
#37737 = CARTESIAN_POINT ( 'NONE',  ( 5.025435985552490159, -30.27990892530747047, 7.754798119455333705 ) ) ;
#37738 = ORIENTED_EDGE ( 'NONE', *, *, #35684, .F. ) ;
#37739 = CARTESIAN_POINT ( 'NONE',  ( 22.87946623223324139, 4.338853656372669398, 3.053785548036103581 ) ) ;
#37740 = DIRECTION ( 'NONE',  ( -0.000000000000000000, -0.000000000000000000, 1.000000000000000000 ) ) ;
#37741 = VECTOR ( 'NONE', #14884, 1000.000000000000000 ) ;
#37742 = ORIENTED_EDGE ( 'NONE', *, *, #11696, .F. ) ;
#37744 = ADVANCED_FACE ( 'NONE', ( #34076 ), #8915, .F. ) ;
#37743 = CARTESIAN_POINT ( 'NONE',  ( 0.4696423075776997580, -26.29345953671220570, 7.698786668945011513 ) ) ;
#37745 = CIRCLE ( 'NONE', #20006, 0.1000000000000028644 ) ;
#37746 = VERTEX_POINT ( 'NONE', #28686 ) ;
#37747 = CARTESIAN_POINT ( 'NONE',  ( 79.47890774847340367, 63.12292952392867562, -3.765547211956735030 ) ) ;
#37749 = DIRECTION ( 'NONE',  ( -0.000000000000000000, -0.000000000000000000, 1.000000000000000000 ) ) ;
#37748 = CARTESIAN_POINT ( 'NONE',  ( 23.61296149509351139, 0.4561011562658625618, 5.500673751672807477 ) ) ;
#37750 = CARTESIAN_POINT ( 'NONE',  ( 80.60418185334548014, 65.53338749785481809, -2.819252638153959101 ) ) ;
#37751 = CARTESIAN_POINT ( 'NONE',  ( 78.65807594933866653, 65.42150623161261080, 2.716276829189492314 ) ) ;
#37752 = CARTESIAN_POINT ( 'NONE',  ( 81.96779975749585390, 61.96402392828839822, 1.000000000000000000 ) ) ;
#37753 = CARTESIAN_POINT ( 'NONE',  ( 3.121324086407806231, -26.64985754041175525, 6.800000000000000711 ) ) ;
#37754 = CARTESIAN_POINT ( 'NONE',  ( 21.85643539959777826, -9.955546997263933662, -6.545918539092090427 ) ) ;
#37755 = B_SPLINE_CURVE_WITH_KNOTS ( 'NONE', 3,
 ( #20750, #36407, #23449, #8178 ),
 .UNSPECIFIED., .F., .F.,
 ( 4, 4 ),
 ( 0.000000000000000000, 6.391136169995200940E-06 ),
 .UNSPECIFIED. ) ;
#37756 = DIRECTION ( 'NONE',  ( -1.000000000000000000, 0.000000000000000000, 0.000000000000000000 ) ) ;
#37757 = ORIENTED_EDGE ( 'NONE', *, *, #4732, .F. ) ;
#37758 = CARTESIAN_POINT ( 'NONE',  ( -74.45682198657978290, 9.142387462817648469, 9.358043394732074916 ) ) ;
#37759 = CARTESIAN_POINT ( 'NONE',  ( 36.87624210086934085, -3.358183527908076282, 5.907681686615140038 ) ) ;
#37760 = ORIENTED_EDGE ( 'NONE', *, *, #23432, .F. ) ;
#37761 = ADVANCED_FACE ( 'NONE', ( #38738 ), #19415, .T. ) ;
#37762 = PLANE ( 'NONE',  #32048 ) ;
#37763 = AXIS2_PLACEMENT_3D ( 'NONE', #29132, #17154, #10775 ) ;
#37764 = EDGE_CURVE ( 'NONE', #24052, #615, #30671, .T. ) ;
#37765 = CARTESIAN_POINT ( 'NONE',  ( -80.90946895960888696, 10.56086125674553422, -1.015159195828805760 ) ) ;
#37766 = CARTESIAN_POINT ( 'NONE',  ( -75.45330471031414277, 33.71485196875532608, 8.800414904976364028 ) ) ;
#37767 = CARTESIAN_POINT ( 'NONE',  ( 35.22138010156052701, -1.046722844669025765, -5.410276998223191747 ) ) ;
#37768 = CARTESIAN_POINT ( 'NONE',  ( 3.772447927860530736, -32.26558897670516757, 6.868387053540522480 ) ) ;
#37769 = CARTESIAN_POINT ( 'NONE',  ( 19.86572073012567330, 6.626268771028025917, 3.306924192844295618 ) ) ;
#37770 = DIRECTION ( 'NONE',  ( 0.000000000000000000, 0.000000000000000000, 1.000000000000000000 ) ) ;
#37771 = CARTESIAN_POINT ( 'NONE',  ( 29.65186663566715808, -3.798820256635906834, 4.430807847150231460 ) ) ;
#37772 = CARTESIAN_POINT ( 'NONE',  ( -2.348748702180637693, -25.49307895267003587, 6.800000000000000711 ) ) ;
#37773 = DIRECTION ( 'NONE',  ( 0.9848077530122080203, 0.1736481776669307198, -0.000000000000000000 ) ) ;
#37774 = CARTESIAN_POINT ( 'NONE',  ( 23.61900895148505697, 0.7560519036968751383, -5.377082254995243282 ) ) ;
#37775 = DIRECTION ( 'NONE',  ( 0.000000000000000000, 0.000000000000000000, 1.000000000000000000 ) ) ;
#37776 = CARTESIAN_POINT ( 'NONE',  ( 26.63902384589101047, 1.612943561579256224, -4.338441080883199241 ) ) ;
#37777 = ORIENTED_EDGE ( 'NONE', *, *, #12329, .T. ) ;
#37778 = ADVANCED_FACE ( 'NONE', ( #38138 ), #3794, .T. ) ;
#37780 = EDGE_CURVE ( 'NONE', #25105, #20784, #7253, .T. ) ;
#37779 = CARTESIAN_POINT ( 'NONE',  ( 67.47898117768387749, 58.07151159967423126, 3.997009152755514272 ) ) ;
#37781 = CARTESIAN_POINT ( 'NONE',  ( 37.00288072789806648, -2.989026547920700327, 5.981592474277436899 ) ) ;
#37782 = EDGE_CURVE ( 'NONE', #40651, #14452, #25798, .T. ) ;
#37783 = CARTESIAN_POINT ( 'NONE',  ( -81.45877670850643426, 35.14220020903839270, 12.50000000000000000 ) ) ;
#37784 = CARTESIAN_POINT ( 'NONE',  ( 84.43092178082896737, 2.949567725576020649, 1.921192885956162444 ) ) ;
#37785 = CARTESIAN_POINT ( 'NONE',  ( 24.75815691998409562, 3.019130790117518170, 3.350895687454368055 ) ) ;
#37786 = ORIENTED_EDGE ( 'NONE', *, *, #3378, .T. ) ;
#37787 = DIRECTION ( 'NONE',  ( 0.4582725098355734938, -0.8888117386314180468, 0.000000000000000000 ) ) ;
#37788 = CARTESIAN_POINT ( 'NONE',  ( 0.000000000000000000, 0.000000000000000000, 0.000000000000000000 ) ) ;
#37789 = CARTESIAN_POINT ( 'NONE',  ( 24.75839165839662925, 3.019244830385916956, -3.350409272483306111 ) ) ;
#37790 = CARTESIAN_POINT ( 'NONE',  ( -1.765215435290630408, -33.48785941387868803, 7.013842709614101167 ) ) ;
#37791 = ORIENTED_EDGE ( 'NONE', *, *, #28655, .T. ) ;
#37792 = CARTESIAN_POINT ( 'NONE',  ( 3.964281165953357000, -26.91534161652651491, 7.781480525794718162 ) ) ;
#37793 = AXIS2_PLACEMENT_3D ( 'NONE', #7003, #29036, #13372 ) ;
#37794 = UNCERTAINTY_MEASURE_WITH_UNIT (LENGTH_MEASURE( 1.000000000000000082E-05 ), #6529, 'distance_accuracy_value', 'NONE');
#37795 = CIRCLE ( 'NONE', #2994, 0.1000000000000028644 ) ;
#37796 = EDGE_LOOP ( 'NONE', ( #21264, #98, #29998, #10544 ) ) ;
#37797 = CARTESIAN_POINT ( 'NONE',  ( 80.29143557890645866, 63.14717164025322660, -3.649417990092601372 ) ) ;
#37798 = VECTOR ( 'NONE', #31408, 1000.000000000000000 ) ;
#37799 = FACE_OUTER_BOUND ( 'NONE', #28179, .T. ) ;
#37800 = CARTESIAN_POINT ( 'NONE',  ( 80.18433095895142060, 63.45046554133028138, 3.702313260098204495 ) ) ;
#37802 = ORIENTED_EDGE ( 'NONE', *, *, #2692, .T. ) ;
#37801 = CARTESIAN_POINT ( 'NONE',  ( -10.87867591359219155, -26.64985754041175525, 6.800000000000000711 ) ) ;
#37803 = VECTOR ( 'NONE', #11292, 1000.000000000000000 ) ;
#37804 = CARTESIAN_POINT ( 'NONE',  ( -0.03917690187701790977, -26.53924484835505382, 7.773839561854631874 ) ) ;
#37805 = CARTESIAN_POINT ( 'NONE',  ( -63.03213158086148837, 38.26878225442762016, -4.032857076800600460 ) ) ;
#37806 = CARTESIAN_POINT ( 'NONE',  ( -71.90227038838925466, -21.04509535909790330, 9.952591258774150518 ) ) ;
#37807 = CARTESIAN_POINT ( 'NONE',  ( -54.80986203264403400, 31.50205531805574211, 1.053352963064339898 ) ) ;
#37808 = CARTESIAN_POINT ( 'NONE',  ( 22.62157167972026883, 4.589994619255199915, -3.081681181103287592 ) ) ;
#37809 = ORIENTED_EDGE ( 'NONE', *, *, #5344, .F. ) ;
#37810 = CARTESIAN_POINT ( 'NONE',  ( -80.92837670882107659, 2.429809908903242555, 15.50000000000000000 ) ) ;
#37811 = ORIENTED_EDGE ( 'NONE', *, *, #37499, .T. ) ;
#37812 = CARTESIAN_POINT ( 'NONE',  ( -1.030057409390036538, -31.59592535501132460, 6.988553391373222290 ) ) ;
#37813 = CARTESIAN_POINT ( 'NONE',  ( -67.16566696069978093, 37.18524951245930055, 8.491446490665028435 ) ) ;
#37814 = CARTESIAN_POINT ( 'NONE',  ( -80.88644286667957317, -6.600206128780238046, -1.001251069996826448 ) ) ;
#37815 = CARTESIAN_POINT ( 'NONE',  ( 5.011198270955363299, -30.34358980514384285, 7.013842709614101167 ) ) ;
#37816 = CARTESIAN_POINT ( 'NONE',  ( 78.67345636894508232, 66.04656848779337963, 1.137963815189256600 ) ) ;
#37817 = CARTESIAN_POINT ( 'NONE',  ( 84.75081314860828741, 2.206698042984908792, -4.319373971756642838 ) ) ;
#37818 = CARTESIAN_POINT ( 'NONE',  ( 22.47899254214195608, 3.957058747972870716, -2.823133405592673562 ) ) ;
#37819 = EDGE_LOOP ( 'NONE', ( #39845, #26168, #4625, #15115 ) ) ;
#37820 = CARTESIAN_POINT ( 'NONE',  ( -64.28450485721612040, 34.79050374529649758, -5.196496127070091120 ) ) ;
#37821 = CARTESIAN_POINT ( 'NONE',  ( 22.07330900774856275, 4.463300359340192536, 0.7514602381188923985 ) ) ;
#37822 = ADVANCED_FACE ( 'NONE', ( #38332 ), #35287, .F. ) ;
#37823 = ORIENTED_EDGE ( 'NONE', *, *, #9436, .T. ) ;
#37824 = VECTOR ( 'NONE', #8185, 1000.000000000000000 ) ;
#37825 = CIRCLE ( 'NONE', #30620, 24.28220113893567245 ) ;
#37826 = CARTESIAN_POINT ( 'NONE',  ( 1.675697498098485116, -26.17001468787846719, 7.740055089680400791 ) ) ;
#37827 = ADVANCED_FACE ( 'NONE', ( #19216 ), #10133, .T. ) ;
#37828 = CARTESIAN_POINT ( 'NONE',  ( 14.80983598776561472, -5.580000773509008027, -2.503340399836785579 ) ) ;
#37829 = DIRECTION ( 'NONE',  ( 0.000000000000000000, 0.000000000000000000, 1.000000000000000000 ) ) ;
#37830 = CARTESIAN_POINT ( 'NONE',  ( 85.61058318453605409, 0.9550117787157472726, 5.816704139769944604 ) ) ;
#37831 = VERTEX_POINT ( 'NONE', #16514 ) ;
#37832 = CARTESIAN_POINT ( 'NONE',  ( 21.25348936832362412, 3.320962282439187341, 3.523519052146550923 ) ) ;
#37833 = AXIS2_PLACEMENT_3D ( 'NONE', #19520, #32101, #29392 ) ;
#37834 = EDGE_CURVE ( 'NONE', #34419, #11926, #35126, .T. ) ;
#37835 = CARTESIAN_POINT ( 'NONE',  ( 87.18644375116411993, 0.4257728571452945587, -5.011944538332810062 ) ) ;
#37836 = VERTEX_POINT ( 'NONE', #37647 ) ;
#37838 = CARTESIAN_POINT ( 'NONE',  ( -3.676122991083663472E-15, 0.5999999999999995337, 3.779754562795982764 ) ) ;
#37837 = CARTESIAN_POINT ( 'NONE',  ( 81.27646189173411528, 61.63998710316791829, -2.098997056522961646 ) ) ;
#37839 = CARTESIAN_POINT ( 'NONE',  ( 5.200346647029098435, -29.55249110255828882, 7.749999999999999112 ) ) ;
#37840 = ORIENTED_EDGE ( 'NONE', *, *, #22485, .F. ) ;
#37841 = CARTESIAN_POINT ( 'NONE',  ( -1.647457617777850825, -28.97670534922106000, 7.769368695748486431 ) ) ;
#37842 = ORIENTED_EDGE ( 'NONE', *, *, #29482, .T. ) ;
#37843 = CARTESIAN_POINT ( 'NONE',  ( -77.13767261641073958, -6.081113133698417883, 7.841263487880433480 ) ) ;
#37845 = ORIENTED_EDGE ( 'NONE', *, *, #39361, .F. ) ;
#37844 = ORIENTED_EDGE ( 'NONE', *, *, #21627, .T. ) ;
#37846 = CARTESIAN_POINT ( 'NONE',  ( 81.09181894009961411, 61.27555711777438319, -1.268354304253237697 ) ) ;
#37847 = CARTESIAN_POINT ( 'NONE',  ( 36.00559039101765535, -3.152632923976596224, 5.825941197649304293 ) ) ;
#37849 = CARTESIAN_POINT ( 'NONE',  ( 37.10781593239299525, -2.412025766632669210, 5.952297030325896188 ) ) ;
#37848 = CARTESIAN_POINT ( 'NONE',  ( 23.78674307609086824, 1.600237366897277802, 4.774347307045557542 ) ) ;
#37851 = ORIENTED_EDGE ( 'NONE', *, *, #5402, .T. ) ;
#37850 = ORIENTED_EDGE ( 'NONE', *, *, #6142, .F. ) ;
#37852 = CARTESIAN_POINT ( 'NONE',  ( 80.84167751523406764, 65.66068717198510285, -2.558871340112543358 ) ) ;
#37853 = VECTOR ( 'NONE', #1316, 1000.000000000000000 ) ;
#37854 = DIRECTION ( 'NONE',  ( -0.000000000000000000, -0.000000000000000000, 1.000000000000000000 ) ) ;
#37855 =( BOUNDED_CURVE ( )  B_SPLINE_CURVE ( 3, ( #10576, #9774, #19854, #29327 ),
 .UNSPECIFIED., .F., .T. ) 
 B_SPLINE_CURVE_WITH_KNOTS ( ( 4, 4 ),
 ( 1.347909859412852684, 1.534781240595297414 ),
 .UNSPECIFIED. ) 
 CURVE ( )  GEOMETRIC_REPRESENTATION_ITEM ( )  RATIONAL_B_SPLINE_CURVE ( ( 1.000000000000000000, 0.9970920404276226723, 0.9970920404276226723, 1.000000000000000000 ) ) 
 REPRESENTATION_ITEM ( '' )  );
#37857 = DIRECTION ( 'NONE',  ( -7.232507224765808510E-18, 1.000000000000000000, 0.000000000000000000 ) ) ;
#37856 = CARTESIAN_POINT ( 'NONE',  ( 3.342564306745924974, -32.66067906797238152, 7.753200566781577763 ) ) ;
#37858 = CARTESIAN_POINT ( 'NONE',  ( -24.44874870218064089, -25.49307895267003587, 6.800000000000000711 ) ) ;
#37859 = CARTESIAN_POINT ( 'NONE',  ( -63.08758708074093136, 41.04287353446839148, -4.000000000000000000 ) ) ;
#37860 = CARTESIAN_POINT ( 'NONE',  ( 71.66251436080506210, 60.98061884659115606, 3.745173303738185577 ) ) ;
#37861 = ORIENTED_EDGE ( 'NONE', *, *, #13402, .T. ) ;
#37862 = CARTESIAN_POINT ( 'NONE',  ( 22.02527683978544104, 4.022755422383132107, -4.157466662046956252 ) ) ;
#37863 = ORIENTED_EDGE ( 'NONE', *, *, #5735, .T. ) ;
#37864 = CIRCLE ( 'NONE', #8941, 6.000000000000005329 ) ;
#37865 = ORIENTED_EDGE ( 'NONE', *, *, #30798, .F. ) ;
#37866 = CARTESIAN_POINT ( 'NONE',  ( 21.85643539959780313, -9.021070270546461600, 11.21731785579436291 ) ) ;
#37867 = CARTESIAN_POINT ( 'NONE',  ( 3.487362763175719138, -26.57752209578763569, 7.785344483711591934 ) ) ;
#37868 = CARTESIAN_POINT ( 'NONE',  ( -1.078675913592196167, -24.55319635012989110, 6.700000000000000178 ) ) ;
#37869 = CARTESIAN_POINT ( 'NONE',  ( 81.74240050578451644, 63.84683571418597836, 2.967158453528944140 ) ) ;
#37870 = CARTESIAN_POINT ( 'NONE',  ( 85.64504565501374600, 2.098084819171330828, -4.577105872335450520 ) ) ;
#37871 = ORIENTED_EDGE ( 'NONE', *, *, #37834, .F. ) ;
#37872 = CARTESIAN_POINT ( 'NONE',  ( -81.82381003581529910, -5.600672066111338943, -0.2226990585086200125 ) ) ;
#37873 = CARTESIAN_POINT ( 'NONE',  ( 14.89717971670494556, -5.930256159152071938, 2.520399783277118111 ) ) ;
#37874 = CARTESIAN_POINT ( 'NONE',  ( 36.89700021831158949, -3.001725562179715201, -5.965067260026661877 ) ) ;
#37875 = CARTESIAN_POINT ( 'NONE',  ( 5.140392049853408807, -28.99927055885797600, 7.783750581861601070 ) ) ;
#37876 = LINE ( 'NONE', #645, #2965 ) ;
#37877 = CARTESIAN_POINT ( 'NONE',  ( -71.72837670882105954, -31.30579396504363388, -1.385640646055078307 ) ) ;
#37878 = EDGE_CURVE ( 'NONE', #7222, #38011, #34406, .T. ) ;
#37879 = ADVANCED_FACE ( 'NONE', ( #19138 ), #37254, .F. ) ;
#37880 = CARTESIAN_POINT ( 'NONE',  ( -1.296490702453536592, -31.17578218382766408, 7.768425012602592439 ) ) ;
#37881 = EDGE_CURVE ( 'NONE', #27685, #8017, #11965, .T. ) ;
#37882 = CARTESIAN_POINT ( 'NONE',  ( 32.91909972634648796, -3.046172459632647822, 5.344219682368552604 ) ) ;
#37883 = EDGE_LOOP ( 'NONE', ( #11950, #38051, #9899, #2319, #38189, #11296 ) ) ;
#37884 = ORIENTED_EDGE ( 'NONE', *, *, #24869, .T. ) ;
#37885 = CARTESIAN_POINT ( 'NONE',  ( 36.87008432447370154, -2.088660079878024156, 5.864835073014669220 ) ) ;
#37886 = DIRECTION ( 'NONE',  ( -0.000000000000000000, -0.000000000000000000, -1.000000000000000000 ) ) ;
#37887 = COLOUR_RGB ( '',0.7921568627450980005, 0.8196078431372548767, 0.9333333333333333481 ) ;
#37888 = ORIENTED_EDGE ( 'NONE', *, *, #14799, .F. ) ;
#37889 = CARTESIAN_POINT ( 'NONE',  ( 66.54635149611212341, 57.90010100995254305, -3.999344142520906864 ) ) ;
#37890 = AXIS2_PLACEMENT_3D ( 'NONE', #23876, #4958, #30077 ) ;
#37891 = EDGE_LOOP ( 'NONE', ( #21619, #20361, #22639, #978, #37738 ) ) ;
#37892 = CARTESIAN_POINT ( 'NONE',  ( 88.26456443100552463, -0.7852234611469554038, -1.669442870725792449 ) ) ;
#37893 = CARTESIAN_POINT ( 'NONE',  ( -75.23895599219262920, 9.844379164151915163, -9.029202135315509636 ) ) ;
#37894 = AXIS2_PLACEMENT_3D ( 'NONE', #34102, #9149, #38316 ) ;
#37895 =( LENGTH_UNIT ( ) NAMED_UNIT ( * ) SI_UNIT ( .MILLI., .METRE. ) );
#37896 = PLANE ( 'NONE',  #20744 ) ;
#37897 = DIRECTION ( 'NONE',  ( 1.000000000000000000, 0.000000000000000000, 0.000000000000000000 ) ) ;
#37898 = ORIENTED_EDGE ( 'NONE', *, *, #15940, .F. ) ;
#37899 = CARTESIAN_POINT ( 'NONE',  ( 22.43706763645577595, 4.742359000873816122, 3.190859319307013831 ) ) ;
#37900 = CARTESIAN_POINT ( 'NONE',  ( 81.32357852907298934, 65.91643957835144363, -1.421283058691077850 ) ) ;
#37901 = CARTESIAN_POINT ( 'NONE',  ( 80.17861389908809144, 63.81053541282458497, 3.679799701112133281 ) ) ;
#37902 = CARTESIAN_POINT ( 'NONE',  ( -1.752498985642892304, -28.99760421947164701, 7.695279973900954751 ) ) ;
#37903 = ORIENTED_EDGE ( 'NONE', *, *, #12365, .F. ) ;
#37904 = VERTEX_POINT ( 'NONE', #37451 ) ;
#37905 = CARTESIAN_POINT ( 'NONE',  ( 76.19453532209955426, 64.30418437363987039, -2.661196496273629641 ) ) ;
#37907 = CARTESIAN_POINT ( 'NONE',  ( 5.566493729709874216, -33.07902254873519610, 6.954324564059724878 ) ) ;
#37906 = CARTESIAN_POINT ( 'NONE',  ( 2.343537225896454856, -33.01033157941493101, 7.686927408461905031 ) ) ;
#37908 = CARTESIAN_POINT ( 'NONE',  ( 16.06987909445021856, 10.26701343839525826, -2.714491302820267737 ) ) ;
#37909 = CARTESIAN_POINT ( 'NONE',  ( 79.27186652256901311, 65.93364065454107958, -2.332991218130509026 ) ) ;
#37910 = CARTESIAN_POINT ( 'NONE',  ( 77.40632518803428752, 64.64540924511487674, 2.913524936156969058 ) ) ;
#37911 = VERTEX_POINT ( 'NONE', #34203 ) ;
#37912 = VERTEX_POINT ( 'NONE', #27781 ) ;
#37913 = VECTOR ( 'NONE', #37995, 1000.000000000000000 ) ;
#37914 = CARTESIAN_POINT ( 'NONE',  ( -39.07867591359219261, -26.64985754041175525, 6.700000000000000178 ) ) ;
#37915 = CARTESIAN_POINT ( 'NONE',  ( 81.96987370863080002, 65.13652322159784092, 1.905332024690495007 ) ) ;
#37917 = CARTESIAN_POINT ( 'NONE',  ( 14.72270833303476500, 13.21629034477860998, 2.500000000000005773 ) ) ;
#37916 = CARTESIAN_POINT ( 'NONE',  ( 4.254245903155988273, -31.96321675751186220, 6.941203072598475465 ) ) ;
#37918 = CARTESIAN_POINT ( 'NONE',  ( 30.01304521823198712, -3.946539318896107318, -3.661452490695084272 ) ) ;
#37919 = VECTOR ( 'NONE', #22874, 1000.000000000000000 ) ;
#37920 = CARTESIAN_POINT ( 'NONE',  ( -1.371934420958921486, -31.24648083264167298, 6.865554069792297653 ) ) ;
#37921 = AXIS2_PLACEMENT_3D ( 'NONE', #30573, #32301, #36734 ) ;
#37922 = CARTESIAN_POINT ( 'NONE',  ( -1.796521113867400654, -29.56993018341788826, 7.767301406056523305 ) ) ;
#37923 = CARTESIAN_POINT ( 'NONE',  ( -64.26379470914699255, 34.82012742686826101, 5.122105205699089225 ) ) ;
#37924 = DIRECTION ( 'NONE',  ( 0.000000000000000000, 0.000000000000000000, 1.000000000000000000 ) ) ;
#37925 = ORIENTED_EDGE ( 'NONE', *, *, #26045, .F. ) ;
#37926 = CARTESIAN_POINT ( 'NONE',  ( -0.6300129605891890971, -32.04565666399172841, 6.903372536218456368 ) ) ;
#37927 = CARTESIAN_POINT ( 'NONE',  ( 81.16957891225065680, 61.30398062001311388, 1.085775560726838895 ) ) ;
#37928 = CARTESIAN_POINT ( 'NONE',  ( 36.96297856671265691, -3.150510869464469899, -5.966408781979020581 ) ) ;
#37929 = CARTESIAN_POINT ( 'NONE',  ( 81.16957891225065680, 61.30398062001312809, -1.085786403289926261 ) ) ;
#37930 = FACE_OUTER_BOUND ( 'NONE', #17827, .T. ) ;
#37931 = CARTESIAN_POINT ( 'NONE',  ( 15.21509089441225981, -3.846322154070160426, -2.581080931073590268 ) ) ;
#37932 = CARTESIAN_POINT ( 'NONE',  ( 3.431434570054124222, -32.49627346798381211, 7.695279973900954751 ) ) ;
#37933 = CARTESIAN_POINT ( 'NONE',  ( -80.76903247909713457, 10.51040070415216299, 4.971711105935894714 ) ) ;
#37934 = LINE ( 'NONE', #9743, #39233 ) ;
#37935 = LINE ( 'NONE', #22323, #4657 ) ;
#37936 = EDGE_CURVE ( 'NONE', #4035, #13762, #36065, .T. ) ;
#37937 = DIRECTION ( 'NONE',  ( -0.9999026450364576490, -0.01395351027862084224, 0.000000000000000000 ) ) ;
#37938 = ORIENTED_EDGE ( 'NONE', *, *, #14619, .T. ) ;
#37939 = DIRECTION ( 'NONE',  ( -0.000000000000000000, -0.000000000000000000, 1.000000000000000000 ) ) ;
#37940 = CARTESIAN_POINT ( 'NONE',  ( 68.10340323693496600, 58.18244674706191688, -3.988335407916729025 ) ) ;
#37941 = CIRCLE ( 'NONE', #27459, 0.1000000000000028644 ) ;
#37942 = VERTEX_POINT ( 'NONE', #34815 ) ;
#37943 = CARTESIAN_POINT ( 'NONE',  ( 5.640181823254226678, -32.92274630468555330, 7.695279973900954751 ) ) ;
#37944 = CARTESIAN_POINT ( 'NONE',  ( 30.77693785172156282, -3.327810147074260705, 4.963017966735677078 ) ) ;
#37945 = CARTESIAN_POINT ( 'NONE',  ( 22.62052229059043640, 3.442390791615673518, 4.088590503876035953 ) ) ;
#37946 = VECTOR ( 'NONE', #30154, 1000.000000000000000 ) ;
#37947 = CARTESIAN_POINT ( 'NONE',  ( -63.96477757089261473, 34.57625524247897175, 15.50000000000000000 ) ) ;
#37948 = AXIS2_PLACEMENT_3D ( 'NONE', #31614, #3437, #22761 ) ;
#37949 = CARTESIAN_POINT ( 'NONE',  ( -16.97867591359219475, -26.64985754041175525, 6.700000000000000178 ) ) ;
#37950 = ORIENTED_EDGE ( 'NONE', *, *, #37960, .T. ) ;
#37951 = DIRECTION ( 'NONE',  ( 0.000000000000000000, 1.000000000000000000, 0.000000000000000000 ) ) ;
#37952 = CARTESIAN_POINT ( 'NONE',  ( 81.19854122754009040, 61.34870327520654598, 1.508787936435544541 ) ) ;
#37953 = ORIENTED_EDGE ( 'NONE', *, *, #34615, .T. ) ;
#37954 = DIRECTION ( 'NONE',  ( -0.000000000000000000, -0.000000000000000000, -1.000000000000000000 ) ) ;
#37955 = ORIENTED_EDGE ( 'NONE', *, *, #7895, .F. ) ;
#37956 = CARTESIAN_POINT ( 'NONE',  ( 79.22522514097650514, 63.97890519848277791, -3.707164540951486398 ) ) ;
#37958 = CARTESIAN_POINT ( 'NONE',  ( -1.482099749853996951, -30.76649125703855958, 7.692469944509198854 ) ) ;
#37957 = CARTESIAN_POINT ( 'NONE',  ( 25.95513938031040269, 0.9030353738542202802, 4.429115342626236185 ) ) ;
#37959 = CARTESIAN_POINT ( 'NONE',  ( 81.04289631910501157, 64.65011820514618535, -3.243459512787966403 ) ) ;
#37960 = EDGE_CURVE ( 'NONE', #27958, #40083, #20812, .T. ) ;
#37961 = CARTESIAN_POINT ( 'NONE',  ( 78.37355578220726215, 65.75145430471653185, 1.935054690158702684 ) ) ;
#37962 = ORIENTED_EDGE ( 'NONE', *, *, #14885, .T. ) ;
#37963 = DIRECTION ( 'NONE',  ( -0.000000000000000000, -0.000000000000000000, 1.000000000000000000 ) ) ;
#37964 = ORIENTED_EDGE ( 'NONE', *, *, #21922, .T. ) ;
#37965 = CARTESIAN_POINT ( 'NONE',  ( 22.58802438714224081, -2.565763546402358486, 8.787087332313648247 ) ) ;
#37966 = DIRECTION ( 'NONE',  ( -0.7055275666422136105, -0.2567910337120335451, -0.6605219282605402364 ) ) ;
#37967 = ORIENTED_EDGE ( 'NONE', *, *, #31579, .F. ) ;
#37968 = CARTESIAN_POINT ( 'NONE',  ( -74.09938582373443694, 6.767060077088832060, 10.75363259336874933 ) ) ;
#37969 = CARTESIAN_POINT ( 'NONE',  ( 27.44078372763345541, 0.9562943962831292888, -4.489200806087393580 ) ) ;
#37970 = VERTEX_POINT ( 'NONE', #22034 ) ;
#37971 = ADVANCED_FACE ( 'NONE', ( #9248 ), #8255, .T. ) ;
#37972 = CARTESIAN_POINT ( 'NONE',  ( 0.6198671074021896432, -26.24097615965804664, 7.753200566781576875 ) ) ;
#37973 = VECTOR ( 'NONE', #11670, 1000.000000000000000 ) ;
#37974 = CARTESIAN_POINT ( 'NONE',  ( 1.732569342880620367, -32.96977789996720531, 7.721096864323902409 ) ) ;
#37975 = CARTESIAN_POINT ( 'NONE',  ( 3.419158195859357097, -26.52102280379090971, 7.697032948437506406 ) ) ;
#37976 = CARTESIAN_POINT ( 'NONE',  ( 36.49360370896476979, -3.560832467653986200, -5.796016089073773969 ) ) ;
#37977 = CARTESIAN_POINT ( 'NONE',  ( -1.560093393064529321, -30.53390888824981531, 6.939395833800445779 ) ) ;
#37978 = DIRECTION ( 'NONE',  ( 0.000000000000000000, 0.000000000000000000, -1.000000000000000000 ) ) ;
#37979 =( BOUNDED_SURFACE ( )  B_SPLINE_SURFACE ( 3, 2, ( 
 ( #2252, #31066, #11678 ),
 ( #6146, #27751, #40499 ),
 ( #15398, #24255, #21797 ),
 ( #12309, #33551, #21179 ),
 ( #36818, #5736, #9218 ),
 ( #21385, #37222, #40107 ) ),
 .UNSPECIFIED., .F., .F., .F. ) 
 B_SPLINE_SURFACE_WITH_KNOTS ( ( 4, 2, 4 ),
 ( 3, 3 ),
 ( 0.6656944266037791991, 1.118245376699337879, 1.570796326794896558 ),
 ( 0.000000000000000000, 1.000000000000000000 ),
 .UNSPECIFIED. ) 
 GEOMETRIC_REPRESENTATION_ITEM ( )  RATIONAL_B_SPLINE_SURFACE ( (
 ( 1.000000000000000000, 0.5935057080259644735, 1.000000000000000000),
 ( 1.000000000000000000, 0.6082500109240246422, 1.000000000000000000),
 ( 1.000000000000000000, 0.6267038978090974100, 1.000000000000000000),
 ( 1.000000000000000000, 0.6661308060341680770, 1.000000000000000000),
 ( 1.000000000000000000, 0.6870851634079389036, 1.000000000000000000),
 ( 1.000000000000000000, 0.7071067811865475727, 1.000000000000000000) ) ) 
 REPRESENTATION_ITEM ( '' )  SURFACE ( )  );
#37980 = CARTESIAN_POINT ( 'NONE',  ( 15.93325076494975256, 10.76686990589485049, 2.654092171972521452 ) ) ;
#37981 = CARTESIAN_POINT ( 'NONE',  ( 5.195328097890849151, -29.75810123217307890, 6.980586498568961851 ) ) ;
#37982 = CARTESIAN_POINT ( 'NONE',  ( 2.343537225896455745, -33.01033157941493101, 7.695279973900954751 ) ) ;
#37983 = CARTESIAN_POINT ( 'NONE',  ( -18.24874870218063450, -26.64985754041175525, 6.800000000000000711 ) ) ;
#37984 = CIRCLE ( 'NONE', #10391, 3.499999999999999556 ) ;
#37985 = AXIS2_PLACEMENT_3D ( 'NONE', #39206, #38605, #10995 ) ;
#37986 = CARTESIAN_POINT ( 'NONE',  ( -2.508659216904252975, -30.29838823369475520, 7.635761828346577573 ) ) ;
#37987 = CARTESIAN_POINT ( 'NONE',  ( 23.99747144395669807, 1.007762411719124618, -4.993298325900711987 ) ) ;
#37988 = CARTESIAN_POINT ( 'NONE',  ( 30.57682521627442185, -3.782462783739084067, -4.515814102832556465 ) ) ;
#37989 = DIRECTION ( 'NONE',  ( 0.000000000000000000, -0.000000000000000000, -1.000000000000000000 ) ) ;
#37990 = EDGE_CURVE ( 'NONE', #33400, #30328, #3116, .T. ) ;
#37991 = ORIENTED_EDGE ( 'NONE', *, *, #2825, .T. ) ;
#37992 = CARTESIAN_POINT ( 'NONE',  ( 66.69105935506532035, 57.95800471661298303, 3.998864354720668146 ) ) ;
#37993 = LINE ( 'NONE', #9795, #24710 ) ;
#37994 = CARTESIAN_POINT ( 'NONE',  ( 88.55280947256005675, -1.781472883390815110, -2.828200999223334566 ) ) ;
#37995 = DIRECTION ( 'NONE',  ( -0.000000000000000000, -0.000000000000000000, 1.000000000000000000 ) ) ;
#37996 = VECTOR ( 'NONE', #5055, 1000.000000000000000 ) ;
#37997 = ORIENTED_EDGE ( 'NONE', *, *, #32057, .T. ) ;
#37998 = CARTESIAN_POINT ( 'NONE',  ( 24.56661666422449741, 2.976733537025225029, 3.586665788575320146 ) ) ;
#37999 = DIRECTION ( 'NONE',  ( 0.000000000000000000, 0.000000000000000000, 1.000000000000000000 ) ) ;
#38000 = CARTESIAN_POINT ( 'NONE',  ( 25.06774369592266538, 3.218163280828734596, -2.425390343617369826 ) ) ;
#38001 = DIRECTION ( 'NONE',  ( 0.000000000000000000, 0.000000000000000000, -1.000000000000000000 ) ) ;
#38002 = ADVANCED_FACE ( 'NONE', ( #33324 ), #17844, .F. ) ;
#38003 = ORIENTED_EDGE ( 'NONE', *, *, #19032, .T. ) ;
#38004 = CARTESIAN_POINT ( 'NONE',  ( -36.44874870218064444, -25.49307895267003587, 6.700000000000000178 ) ) ;
#38005 = DIRECTION ( 'NONE',  ( 1.000000000000000000, 0.000000000000000000, 0.000000000000000000 ) ) ;
#38006 = ORIENTED_EDGE ( 'NONE', *, *, #30995, .T. ) ;
#38007 = CARTESIAN_POINT ( 'NONE',  ( 79.23217405491418219, 65.02354781853190957, -3.268578535636863514 ) ) ;
#38008 = CARTESIAN_POINT ( 'NONE',  ( -1.697659286293943692, -29.45477631113573480, 7.761597726988852308 ) ) ;
#38009 = CARTESIAN_POINT ( 'NONE',  ( 78.69071029820845808, 65.87362605733925136, 2.012706562768930230 ) ) ;
#38012 = EDGE_LOOP ( 'NONE', ( #30385, #20304, #18729, #28751 ) ) ;
#38011 = VERTEX_POINT ( 'NONE', #2235 ) ;
#38010 = CARTESIAN_POINT ( 'NONE',  ( -70.92837670882107659, 13.87661300689593880, 3.784187430299790211 ) ) ;
#38013 = CYLINDRICAL_SURFACE ( 'NONE', #17271, 0.1000000000000028644 ) ;
#38014 = CARTESIAN_POINT ( 'NONE',  ( 0.9853232624859283861, -32.99610581046875524, 6.864673517077424236 ) ) ;
#38015 = CARTESIAN_POINT ( 'NONE',  ( -65.15086340151077593, 36.36839105661640303, -8.980608347108747225 ) ) ;
#38016 = EDGE_CURVE ( 'NONE', #8738, #3771, #39675, .T. ) ;
#38017 = ADVANCED_FACE ( 'NONE', ( #11058 ), #11663, .F. ) ;
#38018 = CARTESIAN_POINT ( 'NONE',  ( 21.85643539959774273, 11.87467848218428834, -0.9583437110454642305 ) ) ;
#38019 = CARTESIAN_POINT ( 'NONE',  ( 23.43039554023339122, 3.779663734359625771, -3.137929522636683455 ) ) ;
#38020 = ORIENTED_EDGE ( 'NONE', *, *, #28084, .T. ) ;
#38021 = EDGE_CURVE ( 'NONE', #20380, #18803, #14756, .T. ) ;
#38022 = ORIENTED_EDGE ( 'NONE', *, *, #37226, .T. ) ;
#38023 = CARTESIAN_POINT ( 'NONE',  ( -0.9401865930518452652, -31.71174127773586449, 6.887041543973311697 ) ) ;
#38024 = CARTESIAN_POINT ( 'NONE',  ( -8.248748702180632719, -25.49307895267003587, 6.700000000000000178 ) ) ;
#38025 = CARTESIAN_POINT ( 'NONE',  ( -77.69396300944833911, -6.284379105152234857, -7.366555388289405926 ) ) ;
#38026 = CYLINDRICAL_SURFACE ( 'NONE', #34722, 3.499999999999999556 ) ;
#38027 = DIRECTION ( 'NONE',  ( -1.000000000000000000, -0.000000000000000000, -0.000000000000000000 ) ) ;
#38028 = CARTESIAN_POINT ( 'NONE',  ( 81.27876882982990026, 62.57402737888433109, 3.057227112800006807 ) ) ;
#38029 = CARTESIAN_POINT ( 'NONE',  ( 86.43572624768424362, -0.5192074800720991590, -5.777013305174518720 ) ) ;
#38030 = DIRECTION ( 'NONE',  ( -0.8888117386314182689, -0.4582725098355732163, 0.000000000000000000 ) ) ;
#38031 = EDGE_LOOP ( 'NONE', ( #1603, #34247, #15383, #35258, #15204 ) ) ;
#38032 = VECTOR ( 'NONE', #23341, 1000.000000000000000 ) ;
#38033 = CARTESIAN_POINT ( 'NONE',  ( -0.8954611659357714082, -31.76573441880953297, 7.635761828346577573 ) ) ;
#38034 = CARTESIAN_POINT ( 'NONE',  ( -10.97867591359219475, -24.55319635012989110, 6.700000000000000178 ) ) ;
#38035 = CARTESIAN_POINT ( 'NONE',  ( -64.84514717441435039, 36.26677316194255241, 6.475000919363831819 ) ) ;
#38036 = CARTESIAN_POINT ( 'NONE',  ( -18.24874870218063450, -25.49307895267003587, 6.800000000000000711 ) ) ;
#38037 = CARTESIAN_POINT ( 'NONE',  ( -1.676686771118219177, -28.62493188826283941, 7.501983001166816933 ) ) ;
#38038 = PLANE ( 'NONE',  #8243 ) ;
#38039 = ADVANCED_FACE ( 'NONE', ( #27325 ), #24238, .F. ) ;
#38040 = B_SPLINE_CURVE_WITH_KNOTS ( 'NONE', 3,
 ( #23362, #7707, #20258, #30975, #28068, #18587, #8916, #11996, #37128, #37530, #2578, #24993, #20873 ),
 .UNSPECIFIED., .F., .F.,
 ( 4, 2, 1, 2, 2, 2, 4 ),
 ( 0.3391172959757620120, 0.4217276339787944250, 0.4630328029803104650, 0.4836853874810680409, 0.5043379719818256168, 0.6695586479878841146, 1.000000000000000000 ),
 .UNSPECIFIED. ) ;
#38041 = VERTEX_POINT ( 'NONE', #25070 ) ;
#38042 = CARTESIAN_POINT ( 'NONE',  ( 35.45320544181257105, -1.915487943862905773, 5.739728166845379675 ) ) ;
#38043 = B_SPLINE_CURVE_WITH_KNOTS ( 'NONE', 3,
 ( #19414, #21899, #31172, #40616, #3400, #37719, #9322, #3792, #3594, #34477 ),
 .UNSPECIFIED., .F., .F.,
 ( 4, 3, 3, 4 ),
 ( 2.168404344971008868E-19, 3.025570593003157737E-05, 6.051145698344088600E-05, 6.468151674593620168E-05 ),
 .UNSPECIFIED. ) ;
#38044 = AXIS2_PLACEMENT_3D ( 'NONE', #29768, #11422, #23987 ) ;
#38045 = VERTEX_POINT ( 'NONE', #22197 ) ;
#38047 = CARTESIAN_POINT ( 'NONE',  ( 8.290806648384990041, -10.90558813203967148, 2.500000000000000000 ) ) ;
#38046 = CARTESIAN_POINT ( 'NONE',  ( 81.26055678261326420, 61.79680472324191243, -2.407735119910393351 ) ) ;
#38048 = CARTESIAN_POINT ( 'NONE',  ( -70.01360951184285852, -48.30983266357521444, 9.958407075284599230 ) ) ;
#38049 = CARTESIAN_POINT ( 'NONE',  ( -0.9006701161811203615, -27.22837715677322379, 7.754798119455333705 ) ) ;
#38050 = LINE ( 'NONE', #9850, #21132 ) ;
#38051 = ORIENTED_EDGE ( 'NONE', *, *, #15191, .F. ) ;
#38052 = CARTESIAN_POINT ( 'NONE',  ( -1.636944644631000756, -28.92016341951145719, 7.785172627573962778 ) ) ;
#38053 = EDGE_LOOP ( 'NONE', ( #6271, #1304, #18647, #40627, #33757, #7567, #6931, #9569 ) ) ;
#38054 = CARTESIAN_POINT ( 'NONE',  ( -75.54470190824260101, -5.203473257850061984, 8.872432550771755189 ) ) ;
#38055 = ORIENTED_EDGE ( 'NONE', *, *, #8902, .F. ) ;
#38056 = AXIS2_PLACEMENT_3D ( 'NONE', #40401, #22104, #31983 ) ;
#38057 = CARTESIAN_POINT ( 'NONE',  ( 81.07324312733535976, 61.26878263851435236, -1.298998371267911400 ) ) ;
#38058 = CARTESIAN_POINT ( 'NONE',  ( -71.72839076221272592, -0.1688020727937513676, 5.947163767836365800 ) ) ;
#38059 = CARTESIAN_POINT ( 'NONE',  ( 22.02680808259401957, 1.706773391190979039, 6.102062103760552247 ) ) ;
#38060 = VERTEX_POINT ( 'NONE', #2858 ) ;
#38061 = EDGE_CURVE ( 'NONE', #18594, #38404, #14939, .T. ) ;
#38062 = CARTESIAN_POINT ( 'NONE',  ( 79.18750747900352849, 66.22443723336834864, -1.498428902123936091 ) ) ;
#38063 = ADVANCED_FACE ( 'NONE', ( #18257 ), #40288, .T. ) ;
#38064 = CARTESIAN_POINT ( 'NONE',  ( 4.744203891191327571, -28.05493923841747161, 6.959317978105162616 ) ) ;
#38066 = CARTESIAN_POINT ( 'NONE',  ( 85.35528217256008077, 2.482620454404805166, 2.380853641630215289 ) ) ;
#38065 = CARTESIAN_POINT ( 'NONE',  ( 4.537656249502012962, -31.44341042241281059, 6.920489980334477487 ) ) ;
#38067 = CARTESIAN_POINT ( 'NONE',  ( 3.423404917024849059, -32.61643964784510530, 6.894806418505347700 ) ) ;
#38068 = CARTESIAN_POINT ( 'NONE',  ( 0.6079532840439894059, -26.24751273171437660, 7.766640943994647550 ) ) ;
#38069 = CARTESIAN_POINT ( 'NONE',  ( 72.21306447944246543, 59.67152943164661849, 3.942504219364092233 ) ) ;
#38070 = CARTESIAN_POINT ( 'NONE',  ( 22.58150593364278791, 3.840177467176269843, -3.813772455918038595 ) ) ;
#38071 = EDGE_LOOP ( 'NONE', ( #29760, #19131, #35407, #22585 ) ) ;
#38072 = DIRECTION ( 'NONE',  ( 1.000000000000000000, -0.000000000000000000, 0.000000000000000000 ) ) ;
#38073 = EDGE_CURVE ( 'NONE', #4341, #26564, #19363, .T. ) ;
#38074 = ORIENTED_EDGE ( 'NONE', *, *, #2408, .T. ) ;
#38075 = CARTESIAN_POINT ( 'NONE',  ( 21.85643539959775694, 0.3794388012242833064, 14.22155525766799045 ) ) ;
#38076 = CARTESIAN_POINT ( 'NONE',  ( -57.16504416091206053, 33.41445838748276742, -4.000000000000000000 ) ) ;
#38077 = CARTESIAN_POINT ( 'NONE',  ( 70.21968079846043054, -4.730580361459368888, 6.000000000000000888 ) ) ;
#38078 = CARTESIAN_POINT ( 'NONE',  ( 81.20219841815031714, 64.34456771236992267, 3.243459512806143863 ) ) ;
#38079 = CARTESIAN_POINT ( 'NONE',  ( 85.19300053701067554, 2.612159253720373275, 3.340723803646971302 ) ) ;
#38080 = VERTEX_POINT ( 'NONE', #21987 ) ;
#38081 = CARTESIAN_POINT ( 'NONE',  ( 0.5091161720689987291, -32.75440289402452265, 7.782167645815905033 ) ) ;
#38082 = CARTESIAN_POINT ( 'NONE',  ( 26.27630619708502735, -2.986427969042946717, 4.300631657982672884 ) ) ;
#38083 = CARTESIAN_POINT ( 'NONE',  ( 34.13619771771038813, -3.132990105432221561, -5.534177259546053662 ) ) ;
#38084 = CARTESIAN_POINT ( 'NONE',  ( 5.061235702123782154, -30.12945902767138406, 7.257242401810555243 ) ) ;
#38085 = LINE ( 'NONE', #21643, #11452 ) ;
#38086 = CARTESIAN_POINT ( 'NONE',  ( 30.63618695437729400, -3.604233874750632616, -4.761443182589183643 ) ) ;
#38087 = ORIENTED_EDGE ( 'NONE', *, *, #25204, .T. ) ;
#38088 = PLANE ( 'NONE',  #38823 ) ;
#38089 = CARTESIAN_POINT ( 'NONE',  ( 28.82329466325964873, -3.930707862937422359, 4.251064711185412293 ) ) ;
#38090 = ORIENTED_EDGE ( 'NONE', *, *, #9302, .T. ) ;
#38091 = EDGE_LOOP ( 'NONE', ( #9602, #29533, #30361, #40634 ) ) ;
#38092 = CARTESIAN_POINT ( 'NONE',  ( 21.73837075214035508, 4.234937956566636963, 2.803927625586267514 ) ) ;
#38093 = CARTESIAN_POINT ( 'NONE',  ( 1.632755592654337118, -33.05534186026571319, 7.784725160561909441 ) ) ;
#38094 = VERTEX_POINT ( 'NONE', #9400 ) ;
#38095 = CARTESIAN_POINT ( 'NONE',  ( 66.57179245706689130, 57.82874523672322908, -3.999903336035371293 ) ) ;
#38096 = ADVANCED_FACE ( 'NONE', ( #18884 ), #27733, .F. ) ;
#38097 = ORIENTED_EDGE ( 'NONE', *, *, #32287, .T. ) ;
#38098 = CARTESIAN_POINT ( 'NONE',  ( 5.928245814084836418, -30.19173177851781276, 7.754798119455333705 ) ) ;
#38099 = DIRECTION ( 'NONE',  ( 0.000000000000000000, 0.6662082868431841165, -0.7457657263118691038 ) ) ;
#38100 = CARTESIAN_POINT ( 'NONE',  ( -17.69482985384421880, -42.37473357531882101, 6.000000000000000000 ) ) ;
#38101 =( BOUNDED_CURVE ( )  B_SPLINE_CURVE ( 3, ( #19492, #16387, #13295, #34251 ),
 .UNSPECIFIED., .F., .T. ) 
 B_SPLINE_CURVE_WITH_KNOTS ( ( 4, 4 ),
 ( 1.381924640371167579, 1.396263401595456699 ),
 .UNSPECIFIED. ) 
 CURVE ( )  GEOMETRIC_REPRESENTATION_ITEM ( )  RATIONAL_B_SPLINE_CURVE ( ( 1.000000000000000000, 0.9999828667339337729, 0.9999828667339337729, 1.000000000000000000 ) ) 
 REPRESENTATION_ITEM ( '' )  );
#38102 = VERTEX_POINT ( 'NONE', #28562 ) ;
#38103 = FACE_BOUND ( 'NONE', #970, .T. ) ;
#38104 = CARTESIAN_POINT ( 'NONE',  ( -24.34874870218063592, -26.64985754041175525, 6.800000000000000711 ) ) ;
#38105 = ORIENTED_EDGE ( 'NONE', *, *, #39587, .T. ) ;
#38106 = CARTESIAN_POINT ( 'NONE',  ( 80.68997016403551470, 66.19852044017248716, -1.342843868341962121 ) ) ;
#38107 = CARTESIAN_POINT ( 'NONE',  ( 79.57367618494546946, 64.93149010139244126, 3.380189700376624362 ) ) ;
#38108 = VECTOR ( 'NONE', #3976, 1000.000000000000000 ) ;
#38109 = CARTESIAN_POINT ( 'NONE',  ( -70.66575442428671749, -21.75648676341283760, 3.995461420868123170 ) ) ;
#38110 = ORIENTED_EDGE ( 'NONE', *, *, #19990, .F. ) ;
#38111 = CARTESIAN_POINT ( 'NONE',  ( 75.98741087703852770, 61.93803417815126977, -3.887901781367206322 ) ) ;
#38113 = CARTESIAN_POINT ( 'NONE',  ( -77.95330471031414277, 33.71485196875532608, 8.800414904976364028 ) ) ;
#38112 = CARTESIAN_POINT ( 'NONE',  ( -1.610418084489225299, -28.79627056164295595, 7.013842709614101167 ) ) ;
#38114 = CARTESIAN_POINT ( 'NONE',  ( 19.77298615262494863, 6.502606513668326649, -3.292450719231072132 ) ) ;
#38115 = CARTESIAN_POINT ( 'NONE',  ( 81.09074532527955625, 63.51554843946187390, -3.425340496581091632 ) ) ;
#38116 = CARTESIAN_POINT ( 'NONE',  ( 75.36936014427642760, 63.22485534106650817, 3.346357594022750792 ) ) ;
#38117 = ORIENTED_EDGE ( 'NONE', *, *, #31284, .T. ) ;
#38118 = EDGE_CURVE ( 'NONE', #37042, #1511, #34768, .T. ) ;
#38119 = CARTESIAN_POINT ( 'NONE',  ( 1.816638696304109235, -26.07269691363555708, 7.761113333117549473 ) ) ;
#38120 = EDGE_CURVE ( 'NONE', #30519, #24028, #12701, .T. ) ;
#38121 = CARTESIAN_POINT ( 'NONE',  ( -58.67303335837859635, 29.89448198981503779, 5.423464252313282330 ) ) ;
#38122 = CARTESIAN_POINT ( 'NONE',  ( 82.16223423120683833, 62.72759567084531795, 2.080779877698173408 ) ) ;
#38124 = CARTESIAN_POINT ( 'NONE',  ( 17.73639058713895267, 11.88077765114964279, 2.500000000000007550 ) ) ;
#38123 = CARTESIAN_POINT ( 'NONE',  ( -0.9720661970843325062, -31.83001367219261013, 7.635761828346575797 ) ) ;
#38125 = CARTESIAN_POINT ( 'NONE',  ( 30.13146195922598380, -4.635528103762326602, -0.9093114724505712010 ) ) ;
#38126 = CARTESIAN_POINT ( 'NONE',  ( -1.699425784502139880, -29.60531690271519523, 7.680992449362115337 ) ) ;
#38127 = CARTESIAN_POINT ( 'NONE',  ( 3.579383117828557559, -26.73631314339753473, 6.949473656533216470 ) ) ;
#38128 = CIRCLE ( 'NONE', #28915, 24.28220113893567245 ) ;
#38129 = CARTESIAN_POINT ( 'NONE',  ( 2.829405163535267942, -26.36285597610873310, 7.695279973900954751 ) ) ;
#38130 = CARTESIAN_POINT ( 'NONE',  ( -70.92837670882107659, -37.87473357531881391, 0.000000000000000000 ) ) ;
#38131 = DIRECTION ( 'NONE',  ( 0.000000000000000000, 0.000000000000000000, 1.000000000000000000 ) ) ;
#38132 = CYLINDRICAL_SURFACE ( 'NONE', #29512, 3.399999999999999911 ) ;
#38133 = CARTESIAN_POINT ( 'NONE',  ( 23.13399818617703119, 3.188625524576914394, -3.769247952470702323 ) ) ;
#38134 = CARTESIAN_POINT ( 'NONE',  ( 11.29080664838499182, -35.94265729135299381, -6.000000000000000000 ) ) ;
#38135 = CARTESIAN_POINT ( 'NONE',  ( 1.736346942945644400, -33.06974547922812491, 7.685194954629195330 ) ) ;
#38136 = CARTESIAN_POINT ( 'NONE',  ( 1.735776812554923332, -32.96974606112863171, 7.680992449362117114 ) ) ;
#38137 = CARTESIAN_POINT ( 'NONE',  ( 2.093592994196940449, -32.94711934045682966, 6.997764925645183709 ) ) ;
#38138 = FACE_OUTER_BOUND ( 'NONE', #1574, .T. ) ;
#38139 = CARTESIAN_POINT ( 'NONE',  ( -1.506684114051581869, -28.44091511309124343, 7.703977250142847844 ) ) ;
#38140 = VECTOR ( 'NONE', #18989, 1000.000000000000000 ) ;
#38141 = ORIENTED_EDGE ( 'NONE', *, *, #543, .T. ) ;
#38142 = FACE_OUTER_BOUND ( 'NONE', #10509, .T. ) ;
#38143 = CARTESIAN_POINT ( 'NONE',  ( 67.99537475662653208, 58.47140781303536983, -3.994255761866590149 ) ) ;
#38144 = VERTEX_POINT ( 'NONE', #5718 ) ;
#38145 = DIRECTION ( 'NONE',  ( -0.000000000000000000, -0.000000000000000000, -1.000000000000000000 ) ) ;
#38146 = CARTESIAN_POINT ( 'NONE',  ( -1.594457770366995319, -28.38926191680453925, 7.750000000000000888 ) ) ;
#38147 = CARTESIAN_POINT ( 'NONE',  ( 24.24310498680376469, 2.794393895970717523, 3.876533112567932537 ) ) ;
#38148 = CARTESIAN_POINT ( 'NONE',  ( -0.7800240848564992113, -27.24451720821412337, 7.013842709614101167 ) ) ;
#38149 = PRODUCT_DEFINITION ( 'UNKNOWN', '', #33396, #23806 ) ;
#38150 = CARTESIAN_POINT ( 'NONE',  ( 5.751251297819365504, -25.49307895267003587, 6.800000000000000711 ) ) ;
#38151 = VERTEX_POINT ( 'NONE', #40481 ) ;
#38152 = VECTOR ( 'NONE', #5893, 1000.000000000000114 ) ;
#38153 = CARTESIAN_POINT ( 'NONE',  ( -40.34874870218063592, -25.49307895267003587, 6.800000000000000711 ) ) ;
#38154 = CARTESIAN_POINT ( 'NONE',  ( 79.00945943828583040, 65.94065490460722856, 2.112861953993760089 ) ) ;
#38155 = CYLINDRICAL_SURFACE ( 'NONE', #17300, 7.538952224936807056 ) ;
#38156 = VERTEX_POINT ( 'NONE', #15381 ) ;
#38157 = CARTESIAN_POINT ( 'NONE',  ( 79.21623058866053668, 63.63573840405092596, -3.765547211956732365 ) ) ;
#38159 = CARTESIAN_POINT ( 'NONE',  ( -1.003704078136529176, -27.34779726144116552, 7.698786668945016842 ) ) ;
#38158 = CARTESIAN_POINT ( 'NONE',  ( 21.73550026715119543, 0.2732327172998176845, 8.957745052953152154 ) ) ;
#38160 = CARTESIAN_POINT ( 'NONE',  ( 81.31796987085881767, 61.39415816021765693, -1.370814772365191114 ) ) ;
#38161 = CARTESIAN_POINT ( 'NONE',  ( 78.49476978275076533, 65.27812458131612061, 2.797036776683046622 ) ) ;
#38162 = EDGE_CURVE ( 'NONE', #13498, #2581, #24751, .T. ) ;
#38163 = AXIS2_PLACEMENT_3D ( 'NONE', #14427, #14831, #8447 ) ;
#38164 = ADVANCED_FACE ( 'NONE', ( #6335 ), #12500, .T. ) ;
#38165 = CARTESIAN_POINT ( 'NONE',  ( -1.625693567409081108, -30.65681645307677883, 7.761113333117553914 ) ) ;
#38166 = B_SPLINE_CURVE_WITH_KNOTS ( 'NONE', 3,
 ( #7632, #7231, #19792, #13609, #26181, #29465, #32365, #19390, #7426, #1276 ),
 .UNSPECIFIED., .F., .F.,
 ( 4, 3, 3, 4 ),
 ( 0.0002170292169044772744, 0.0002420761345915938153, 0.0002723302478206962997, 0.0002816811360866765842 ),
 .UNSPECIFIED. ) ;
#38168 = ORIENTED_EDGE ( 'NONE', *, *, #14569, .T. ) ;
#38167 = CARTESIAN_POINT ( 'NONE',  ( -64.08758708074093136, 41.04287353446839148, 4.000000000000000000 ) ) ;
#38169 = CARTESIAN_POINT ( 'NONE',  ( 22.49677218534670331, -0.6234722885575160189, 9.207484322151008982 ) ) ;
#38170 = CARTESIAN_POINT ( 'NONE',  ( -71.72837670882105954, -31.30579396504363388, 1.385640646055090519 ) ) ;
#38171 = VERTEX_POINT ( 'NONE', #34156 ) ;
#38172 = CARTESIAN_POINT ( 'NONE',  ( -74.21348950129103628, -2.081539577114183803, 9.498975700750209583 ) ) ;
#38173 = CARTESIAN_POINT ( 'NONE',  ( 21.96608578389022171, 0.2111773095693803282, -7.751388582462531929 ) ) ;
#38174 = ORIENTED_EDGE ( 'NONE', *, *, #27849, .T. ) ;
#38175 = CARTESIAN_POINT ( 'NONE',  ( -0.04847345716399687615, -32.59792774950750527, 7.767720160662273443 ) ) ;
#38176 = CARTESIAN_POINT ( 'NONE',  ( 23.38231645333376818, 4.144860998403037122, 2.192943146592336134 ) ) ;
#38177 = CARTESIAN_POINT ( 'NONE',  ( 28.82242951612792581, -3.931231161810520014, -4.250723811025777010 ) ) ;
#38178 = CARTESIAN_POINT ( 'NONE',  ( 33.94570531977476691, -0.4887297205857646931, -5.122339712429196723 ) ) ;
#38179 = CARTESIAN_POINT ( 'NONE',  ( 3.725780183617367403, -32.30082791660831987, 6.920489980334481039 ) ) ;
#38180 = CARTESIAN_POINT ( 'NONE',  ( 15.78123433858440450, 10.66027319286623687, 2.669441307767606020 ) ) ;
#38181 = CARTESIAN_POINT ( 'NONE',  ( 5.199813315060819896, -29.63410109264166081, 6.870737987065016483 ) ) ;
#38182 = CARTESIAN_POINT ( 'NONE',  ( -5.316495087772350914, -32.84709638682603838, 0.000000000000000000 ) ) ;
#38183 = DIRECTION ( 'NONE',  ( 1.000000000000000000, -0.000000000000000000, 0.000000000000000000 ) ) ;
#38184 = AXIS2_PLACEMENT_3D ( 'NONE', #27460, #36931, #40015 ) ;
#38185 = CARTESIAN_POINT ( 'NONE',  ( -9.078675913592196167, -24.55319635012989110, 6.700000000000000178 ) ) ;
#38186 = CARTESIAN_POINT ( 'NONE',  ( 25.37327375539348751, 1.417373392026759493, -4.399323053431193564 ) ) ;
#38187 = CARTESIAN_POINT ( 'NONE',  ( 29.87221045764711747, 1.073546826849551161, -4.301872174529671078 ) ) ;
#38188 = CARTESIAN_POINT ( 'NONE',  ( 5.030284764849001000, -28.49206123220129783, 7.750000000000000888 ) ) ;
#38189 = ORIENTED_EDGE ( 'NONE', *, *, #33110, .T. ) ;
#38190 = EDGE_LOOP ( 'NONE', ( #28754, #10248, #20570, #18 ) ) ;
#38191 = CARTESIAN_POINT ( 'NONE',  ( 66.54439450091902586, 57.90558988169555477, 3.999229419688612008 ) ) ;
#38192 = EDGE_CURVE ( 'NONE', #24834, #14785, #5647, .T. ) ;
#38193 = CARTESIAN_POINT ( 'NONE',  ( -0.1977194167126442581, -34.26956452006460552, 6.954324564059724878 ) ) ;
#38194 = CARTESIAN_POINT ( 'NONE',  ( 84.96877181165257298, 2.299433286287765554, -4.273906790846864645 ) ) ;
#38195 = VECTOR ( 'NONE', #14669, 1000.000000000000000 ) ;
#38196 = DIRECTION ( 'NONE',  ( -0.000000000000000000, -0.000000000000000000, -1.000000000000000000 ) ) ;
#38197 = VERTEX_POINT ( 'NONE', #31255 ) ;
#38198 = CARTESIAN_POINT ( 'NONE',  ( 27.14060876212918316, 1.318306631261646045, 4.438683710678335004 ) ) ;
#38199 = LINE ( 'NONE', #26466, #25165 ) ;
#38200 = LINE ( 'NONE', #1369, #27282 ) ;
#38201 = ORIENTED_EDGE ( 'NONE', *, *, #25634, .F. ) ;
#38202 = EDGE_CURVE ( 'NONE', #22978, #24175, #10521, .T. ) ;
#38203 = EDGE_LOOP ( 'NONE', ( #11916, #31525, #32704, #29812 ) ) ;
#38204 = CARTESIAN_POINT ( 'NONE',  ( 80.38728350982638915, 62.86383526565660418, -3.543129918319041227 ) ) ;
#38205 = CARTESIAN_POINT ( 'NONE',  ( 5.043330201822981529, -28.53322799357174588, 7.013842709614101167 ) ) ;
#38206 = CARTESIAN_POINT ( 'NONE',  ( 80.45282402617027628, 62.88786617374236698, 3.531602295408444281 ) ) ;
#38208 = ORIENTED_EDGE ( 'NONE', *, *, #5549, .T. ) ;
#38207 = CARTESIAN_POINT ( 'NONE',  ( -34.44874870218064444, -25.49307895267003587, 6.700000000000000178 ) ) ;
#38209 = AXIS2_PLACEMENT_3D ( 'NONE', #23266, #4536, #7207 ) ;
#38210 = DIRECTION ( 'NONE',  ( -1.000000000000000000, 0.000000000000000000, 0.000000000000000000 ) ) ;
#38211 = EDGE_CURVE ( 'NONE', #32354, #10467, #21543, .T. ) ;
#38212 = B_SPLINE_CURVE_WITH_KNOTS ( 'NONE', 3,
 ( #33362, #33562, #30672, #15207, #30049, #1862, #2265, #36830, #5339, #27761, #36425, #20984, #27358, #15003, #17875, #8612, #23849, #24057, #30878, #26955, #21191, #36625, #12104, #8813, #33764, #5747, #5542, #39500, #14580, #40315, #40119, #17668, #8410 ),
 .UNSPECIFIED., .F., .F.,
 ( 4, 2, 2, 2, 2, 1, 1, 1, 1, 2, 2, 2, 2, 1, 1, 1, 1, 1, 2, 2, 4 ),
 ( 0.000000000000000000, 0.1250000000000277278, 0.1875000000000412725, 0.2187500000000483225, 0.2343750000000518474, 0.2421875000000538458, 0.2460937500000548173, 0.2480468750000554834, 0.2490234375000556222, 0.2495117187500556777, 0.2500000000000557332, 0.3750000000000170974, 0.4374999999999981126, 0.4687499999999886202, 0.4843749999999836242, 0.4921874999999813483, 0.4960937499999801825, 0.4980468749999799050, 0.4990234374999800160, 0.4999999999999801270, 1.000000000000000000 ),
 .UNSPECIFIED. ) ;
#38213 = CARTESIAN_POINT ( 'NONE',  ( 27.34605239800119136, -4.443250099184577806, 3.670018459242561981 ) ) ;
#38214 = CARTESIAN_POINT ( 'NONE',  ( 2.875937710231030398, -32.76024173560432473, 7.635761828346577573 ) ) ;
#38215 = CARTESIAN_POINT ( 'NONE',  ( 21.85643539959777115, 5.662525507098640887, -13.61651877770312957 ) ) ;
#38216 = CARTESIAN_POINT ( 'NONE',  ( 23.14021789239912863, 4.034458455300417690, -3.103648843234191101 ) ) ;
#38217 = VERTEX_POINT ( 'NONE', #16990 ) ;
#38218 = CARTESIAN_POINT ( 'NONE',  ( -64.85784325972055342, 34.81586596186931359, -6.466735817496061856 ) ) ;
#38219 = ORIENTED_EDGE ( 'NONE', *, *, #28685, .T. ) ;
#38220 = CARTESIAN_POINT ( 'NONE',  ( -1.024433710227528715, -31.60349360017290010, 7.006423389747791219 ) ) ;
#38221 = CARTESIAN_POINT ( 'NONE',  ( -11.07867591359219794, -26.64985754041175525, 6.700000000000000178 ) ) ;
#38222 = TOROIDAL_SURFACE ( 'NONE', #29677, 3.778021175560965172, 0.2000000000000000111 ) ;
#38223 = CARTESIAN_POINT ( 'NONE',  ( -74.23111751286343463, -2.107699029187716455, -9.492660611869487397 ) ) ;
#38224 = DIRECTION ( 'NONE',  ( 0.5751513419797864568, 0.4826092789263677907, -0.6605219282605402364 ) ) ;
#38225 = DIRECTION ( 'NONE',  ( 0.000000000000000000, 1.000000000000000000, 0.000000000000000000 ) ) ;
#38226 = CARTESIAN_POINT ( 'NONE',  ( 80.13405435096434815, 64.91068451853310250, 3.368075118064914886 ) ) ;
#38227 = CARTESIAN_POINT ( 'NONE',  ( 88.13894822871212398, -2.422255244508634053, -0.8714879239747004291 ) ) ;
#38228 = CARTESIAN_POINT ( 'NONE',  ( -0.5662622401650002635, -26.90303891564647643, 7.743886751744256003 ) ) ;
#38229 = DIRECTION ( 'NONE',  ( 0.000000000000000000, 0.000000000000000000, 1.000000000000000000 ) ) ;
#38230 = CARTESIAN_POINT ( 'NONE',  ( 22.07207100664286870, 4.383386263552846884, 1.524166271142376239 ) ) ;
#38231 = CARTESIAN_POINT ( 'NONE',  ( 33.64165290529265206, -1.232672941509324716, 5.456991580957781807 ) ) ;
#38232 = ORIENTED_EDGE ( 'NONE', *, *, #20166, .F. ) ;
#38233 = CARTESIAN_POINT ( 'NONE',  ( 1.780896029553550974, -26.17087081469721710, 7.782034975670476307 ) ) ;
#38234 = CARTESIAN_POINT ( 'NONE',  ( -0.3205960974507152672, -26.83577306605956281, 6.969307238440506147 ) ) ;
#38235 = CARTESIAN_POINT ( 'NONE',  ( 4.655111535418318347, -27.88775428304872861, 7.779495906702015517 ) ) ;
#38236 = VERTEX_POINT ( 'NONE', #25875 ) ;
#38237 = CARTESIAN_POINT ( 'NONE',  ( 35.45419760563620315, -1.912960601587893716, 5.739883018005628834 ) ) ;
#38238 = ADVANCED_FACE ( 'NONE', ( #29562 ), #21775, .T. ) ;
#38239 = CARTESIAN_POINT ( 'NONE',  ( 72.25564410411975302, 59.56945073910184618, -3.929231508797897288 ) ) ;
#38240 = CARTESIAN_POINT ( 'NONE',  ( 4.224974933773748553, -31.84731275619759927, 7.754798119455333705 ) ) ;
#38241 = CARTESIAN_POINT ( 'NONE',  ( 85.32384696181071604, 2.517929975123688990, -2.669340390032339361 ) ) ;
#38242 = ORIENTED_EDGE ( 'NONE', *, *, #17587, .F. ) ;
#38244 = CARTESIAN_POINT ( 'NONE',  ( -0.4167251375549447245, -26.78284871713423954, 6.895394898881664680 ) ) ;
#38243 = CARTESIAN_POINT ( 'NONE',  ( 80.90982241169463407, 63.07641264110139190, -3.420541042474583460 ) ) ;
#38245 = EDGE_CURVE ( 'NONE', #19379, #20545, #33921, .T. ) ;
#38246 = DIRECTION ( 'NONE',  ( 0.000000000000000000, -0.000000000000000000, -1.000000000000000000 ) ) ;
#38247 = VERTEX_POINT ( 'NONE', #18237 ) ;
#38248 = EDGE_CURVE ( 'NONE', #10739, #37970, #21329, .T. ) ;
#38249 = DIRECTION ( 'NONE',  ( 1.000000000000000000, 0.000000000000000000, 0.000000000000000000 ) ) ;
#38250 = EDGE_LOOP ( 'NONE', ( #1846, #37585, #9539, #27319 ) ) ;
#38251 = CARTESIAN_POINT ( 'NONE',  ( -78.33784134423007117, -6.465022251522651864, 6.728521485594535001 ) ) ;
#38252 = EDGE_CURVE ( 'NONE', #36487, #25629, #24842, .T. ) ;
#38253 = VECTOR ( 'NONE', #19137, 1000.000000000000000 ) ;
#38255 = ORIENTED_EDGE ( 'NONE', *, *, #5858, .T. ) ;
#38254 = ORIENTED_EDGE ( 'NONE', *, *, #36082, .F. ) ;
#38256 = ORIENTED_EDGE ( 'NONE', *, *, #8812, .F. ) ;
#38257 = CARTESIAN_POINT ( 'NONE',  ( 78.89771339490202706, 65.85133954292349756, -2.202709653501102149 ) ) ;
#38258 = DIRECTION ( 'NONE',  ( 6.733236168141593227E-15, 0.8314686954258621032, 0.5555716052200788679 ) ) ;
#38259 = CARTESIAN_POINT ( 'NONE',  ( 23.79107460766518400, 2.334731070376283579, 4.312254787772835662 ) ) ;
#38260 = EDGE_LOOP ( 'NONE', ( #25248, #20514, #16375, #15005 ) ) ;
#38261 = CARTESIAN_POINT ( 'NONE',  ( 4.685711905533233690, -27.94270749518966568, 6.870716933885665512 ) ) ;
#38262 = ADVANCED_FACE ( 'NONE', ( #2635 ), #34133, .F. ) ;
#38264 = DIRECTION ( 'NONE',  ( -1.000000000000000000, 0.000000000000000000, 0.000000000000000000 ) ) ;
#38263 = CARTESIAN_POINT ( 'NONE',  ( 14.75988012746532441, 13.12337194104328653, -2.499999999999869882 ) ) ;
#38265 = CARTESIAN_POINT ( 'NONE',  ( -70.92837670882107659, -56.35932253828836025, 0.000000000000000000 ) ) ;
#38266 = CARTESIAN_POINT ( 'NONE',  ( -63.70768059281056850, 44.39675795404822622, -1.227363068883322139 ) ) ;
#38267 = CARTESIAN_POINT ( 'NONE',  ( 69.72614016916874391, 59.17085620800508394, 3.982895692900133344 ) ) ;
#38268 = ORIENTED_EDGE ( 'NONE', *, *, #4572, .F. ) ;
#38269 = CARTESIAN_POINT ( 'NONE',  ( 24.12389204279378063, 2.961437545701208318, -3.763128746285317128 ) ) ;
#38270 = ORIENTED_EDGE ( 'NONE', *, *, #13488, .T. ) ;
#38271 = FACE_OUTER_BOUND ( 'NONE', #21401, .T. ) ;
#38272 = ORIENTED_EDGE ( 'NONE', *, *, #34462, .T. ) ;
#38273 = CARTESIAN_POINT ( 'NONE',  ( 21.85643539959774273, -5.916281280498693285, 11.28130179073419015 ) ) ;
#38274 = CARTESIAN_POINT ( 'NONE',  ( 21.85643539959905368, 4.448544635521362700, -2.117591927232864712 ) ) ;
#38275 = CARTESIAN_POINT ( 'NONE',  ( 4.044183932535696080, -26.97057787552901331, 7.751599049952198506 ) ) ;
#38276 = CARTESIAN_POINT ( 'NONE',  ( 80.19843342641586048, 65.64991096649582403, 2.811330881970102613 ) ) ;
#38277 = CARTESIAN_POINT ( 'NONE',  ( 88.80901725076027731, -1.591322664339660298, -1.862171775454326550 ) ) ;
#38278 = ORIENTED_EDGE ( 'NONE', *, *, #35312, .F. ) ;
#38279 = CARTESIAN_POINT ( 'NONE',  ( 14.77315594796431064, 13.19392823276595195, 2.499999999999996891 ) ) ;
#38280 = CARTESIAN_POINT ( 'NONE',  ( 14.73577947313193270, -4.490654621266425117, 2.506272791592270899 ) ) ;
#38281 = CARTESIAN_POINT ( 'NONE',  ( 36.08720898791031573, -2.181208829428816109, 5.838679753647628701 ) ) ;
#38282 = CARTESIAN_POINT ( 'NONE',  ( -10.24874870218063450, -25.49307895267003587, 6.700000000000000178 ) ) ;
#38283 = CARTESIAN_POINT ( 'NONE',  ( 36.14153500552394149, -3.143492148517922580, -5.847158642575881693 ) ) ;
#38284 = CARTESIAN_POINT ( 'NONE',  ( -34.44874870218064444, -26.64985754041175525, 6.700000000000000178 ) ) ;
#38285 = LINE ( 'NONE', #32147, #27255 ) ;
#38286 = CARTESIAN_POINT ( 'NONE',  ( -72.89163490554884106, 1.565256442275936966, 10.95728629449147995 ) ) ;
#38287 = ORIENTED_EDGE ( 'NONE', *, *, #35567, .F. ) ;
#38288 = CARTESIAN_POINT ( 'NONE',  ( 1.713892699967726196, -25.86893018339335271, 7.635761828346577573 ) ) ;
#38289 = CARTESIAN_POINT ( 'NONE',  ( 29.54621482125871879, -3.606128174059152869, 4.678900705189122711 ) ) ;
#38290 = EDGE_LOOP ( 'NONE', ( #900, #29244 ) ) ;
#38291 = ORIENTED_EDGE ( 'NONE', *, *, #32049, .T. ) ;
#38292 = CARTESIAN_POINT ( 'NONE',  ( 37.10858378118385303, -2.405180162493830487, 5.952030529888895138 ) ) ;
#38293 = CARTESIAN_POINT ( 'NONE',  ( -1.555370887017037518, -28.56597033754369619, 7.139196562012273262 ) ) ;
#38294 = EDGE_CURVE ( 'NONE', #38236, #19152, #36627, .T. ) ;
#38295 = CARTESIAN_POINT ( 'NONE',  ( 66.56787846382142959, 57.83972306852010803, -3.999917672784798039 ) ) ;
#38296 = CARTESIAN_POINT ( 'NONE',  ( 87.20834523746592026, -1.621581766752904441, -4.479905140931061958 ) ) ;
#38297 = EDGE_CURVE ( 'NONE', #19232, #2584, #19574, .T. ) ;
#38298 = EDGE_LOOP ( 'NONE', ( #7319, #24281, #9547, #28279 ) ) ;
#38299 = CARTESIAN_POINT ( 'NONE',  ( 4.929393269055085902, -28.50520041390408110, 6.864651958020304257 ) ) ;
#38300 = CARTESIAN_POINT ( 'NONE',  ( 11.29080664838499182, -35.94265729135299381, 6.000000000000000000 ) ) ;
#38301 = EDGE_LOOP ( 'NONE', ( #19892, #3909, #39932, #31708 ) ) ;
#38302 = CARTESIAN_POINT ( 'NONE',  ( 11.65737507970504616, -30.94667987854474234, 6.800000000000000711 ) ) ;
#38303 = DIRECTION ( 'NONE',  ( 0.000000000000000000, 0.000000000000000000, 1.000000000000000000 ) ) ;
#38304 = ORIENTED_EDGE ( 'NONE', *, *, #21484, .T. ) ;
#38305 = CARTESIAN_POINT ( 'NONE',  ( 82.37993866337100712, 63.11845131094293038, -1.936735430446280048 ) ) ;
#38306 = CYLINDRICAL_SURFACE ( 'NONE', #5781, 0.09010775117052928496 ) ;
#38307 = CARTESIAN_POINT ( 'NONE',  ( 2.891664014397211435, -26.38545747276229037, 7.782167645815905921 ) ) ;
#38308 = ORIENTED_EDGE ( 'NONE', *, *, #10508, .F. ) ;
#38309 = CARTESIAN_POINT ( 'NONE',  ( 75.63732367802946044, 59.67466586216193036, -3.300071129360658162 ) ) ;
#38311 = CARTESIAN_POINT ( 'NONE',  ( 0.6711941891205335242, 0.5999999999999995337, -3.974981096219152299 ) ) ;
#38310 = CARTESIAN_POINT ( 'NONE',  ( -3.078675913592197944, -26.64985754041175525, 6.700000000000000178 ) ) ;
#38312 = CARTESIAN_POINT ( 'NONE',  ( 15.86194215377555494, 10.70901654444746676, -2.668816250362950449 ) ) ;
#38313 = CARTESIAN_POINT ( 'NONE',  ( 76.46948511138620574, 60.90388096812812790, 3.723120700756737289 ) ) ;
#38314 = ORIENTED_EDGE ( 'NONE', *, *, #21484, .F. ) ;
#38315 = VECTOR ( 'NONE', #5657, 1000.000000000000000 ) ;
#38316 = DIRECTION ( 'NONE',  ( -0.6427876096865502431, -0.7660444431189689096, 0.000000000000000000 ) ) ;
#38317 = CARTESIAN_POINT ( 'NONE',  ( -17.27251170661583402, 3.729367930467589076, 6.000000000000000000 ) ) ;
#38318 = CARTESIAN_POINT ( 'NONE',  ( 81.84349429120960906, 61.90138267109058745, 1.539394129974046344 ) ) ;
#38319 = CARTESIAN_POINT ( 'NONE',  ( 87.04213330793400871, 0.5878691963681530464, -4.891134986362597914 ) ) ;
#38320 = CARTESIAN_POINT ( 'NONE',  ( 26.98641761431236930, 1.293889648236598022, -5.140668381306381818 ) ) ;
#38321 = CARTESIAN_POINT ( 'NONE',  ( 2.320588003725592152, -26.22697422319578919, 7.782167645815905033 ) ) ;
#38322 = CARTESIAN_POINT ( 'NONE',  ( 3.565367263018084376, -26.72706101894873854, 7.006423389747789443 ) ) ;
#38323 = CARTESIAN_POINT ( 'NONE',  ( 3.121324086407806231, -26.64985754041175525, 6.700000000000000178 ) ) ;
#38324 = DIRECTION ( 'NONE',  ( 0.2567910337120318243, -0.7055275666422164971, 0.6605219282605376829 ) ) ;
#38325 = PLANE ( 'NONE',  #32855 ) ;
#38326 = CARTESIAN_POINT ( 'NONE',  ( 37.11166072668748228, -2.778356675396603581, -5.998012396607308894 ) ) ;
#38327 = CARTESIAN_POINT ( 'NONE',  ( -70.92837670882107659, -56.35932253828836025, -10.00000000000000888 ) ) ;
#38328 = CARTESIAN_POINT ( 'NONE',  ( -0.8958908980039607117, -31.76523428969960960, 7.756377446753169203 ) ) ;
#38329 = CARTESIAN_POINT ( 'NONE',  ( 3.405093419812497135, -32.51170776363409232, 7.763628509615287498 ) ) ;
#38330 = CARTESIAN_POINT ( 'NONE',  ( 2.088980497471658371, -32.94765204068701081, 6.920489980334479263 ) ) ;
#38331 = EDGE_CURVE ( 'NONE', #22060, #21747, #8510, .T. ) ;
#38332 = FACE_OUTER_BOUND ( 'NONE', #17943, .T. ) ;
#38333 = CARTESIAN_POINT ( 'NONE',  ( -1.459351274368037465, -28.31449385892586079, 7.774064877406528851 ) ) ;
#38334 = ADVANCED_FACE ( 'NONE', ( #37388 ), #19477, .F. ) ;
#38335 = CARTESIAN_POINT ( 'NONE',  ( 32.50899170535470262, -3.013835995739015061, 5.280212407192823143 ) ) ;
#38336 = ORIENTED_EDGE ( 'NONE', *, *, #39830, .F. ) ;
#38337 =( BOUNDED_CURVE ( )  B_SPLINE_CURVE ( 3, ( #10957, #38558, #14053, #29114 ),
 .UNSPECIFIED., .F., .T. ) 
 B_SPLINE_CURVE_WITH_KNOTS ( ( 4, 4 ),
 ( 4.708531083176466403, 4.895802057644187855 ),
 .UNSPECIFIED. ) 
 CURVE ( )  GEOMETRIC_REPRESENTATION_ITEM ( )  RATIONAL_B_SPLINE_CURVE ( ( 1.000000000000000000, 0.9970795998553221295, 0.9970795998553221295, 1.000000000000000000 ) ) 
 REPRESENTATION_ITEM ( '' )  );
#38338 = DIRECTION ( 'NONE',  ( -0.000000000000000000, 1.000000000000000000, -0.000000000000000000 ) ) ;
#38339 = CARTESIAN_POINT ( 'NONE',  ( 67.75953150630846267, 58.21208410194267202, -3.997018227265522139 ) ) ;
#38340 = MECHANICAL_DESIGN_GEOMETRIC_PRESENTATION_REPRESENTATION (  '', ( #15334 ), #16612 ) ;
#38341 = EDGE_CURVE ( 'NONE', #11093, #16613, #6108, .T. ) ;
#38342 = ORIENTED_EDGE ( 'NONE', *, *, #36132, .F. ) ;
#38343 = CARTESIAN_POINT ( 'NONE',  ( -2.707143391484601924, -27.16588715693004730, 7.754798119455333705 ) ) ;
#38344 = EDGE_CURVE ( 'NONE', #25619, #25932, #1166, .T. ) ;
#38345 = DIRECTION ( 'NONE',  ( 0.000000000000000000, 1.000000000000000000, 0.000000000000000000 ) ) ;
#38346 = CARTESIAN_POINT ( 'NONE',  ( 23.90227964751484535, 3.010637336354621496, 3.787656613205743650 ) ) ;
#38347 = CARTESIAN_POINT ( 'NONE',  ( 0.4868412872024892035, -26.28704995000200029, 7.640616322432099317 ) ) ;
#38348 = CARTESIAN_POINT ( 'NONE',  ( -1.468618840926277036, -28.33807089344026764, 6.874555630061441214 ) ) ;
#38349 = DIRECTION ( 'NONE',  ( 1.000000000000000000, 0.000000000000000000, 0.000000000000000000 ) ) ;
#38350 = DIRECTION ( 'NONE',  ( -0.000000000000000000, -0.000000000000000000, 1.000000000000000000 ) ) ;
#38351 = EDGE_LOOP ( 'NONE', ( #30886, #25194, #19101, #1993, #8775 ) ) ;
#38352 = CARTESIAN_POINT ( 'NONE',  ( 24.75663416313030751, 3.018532308770745409, 3.353834330914950090 ) ) ;
#38353 = DIRECTION ( 'NONE',  ( 0.000000000000000000, 0.000000000000000000, 1.000000000000000000 ) ) ;
#38355 = VECTOR ( 'NONE', #4435, 1000.000000000000000 ) ;
#38354 = CARTESIAN_POINT ( 'NONE',  ( 80.90982241169463407, 63.07641264110139190, 3.420541042474586568 ) ) ;
#38356 = DIRECTION ( 'NONE',  ( -0.000000000000000000, -0.000000000000000000, 1.000000000000000000 ) ) ;
#38357 = ORIENTED_EDGE ( 'NONE', *, *, #22298, .F. ) ;
#38358 = CARTESIAN_POINT ( 'NONE',  ( 78.81457101317378999, 64.04164361847183784, -3.641957811749153340 ) ) ;
#38359 = CARTESIAN_POINT ( 'NONE',  ( 23.59559651940404024, 0.4311816695734068117, 5.519554995405929532 ) ) ;
#38360 = CARTESIAN_POINT ( 'NONE',  ( 80.71932482181539115, 65.23126254902230414, -3.019969592843242179 ) ) ;
#38361 = CARTESIAN_POINT ( 'NONE',  ( 80.31443933487476272, 61.76769068803228890, 3.015657119755351889 ) ) ;
#38362 = AXIS2_PLACEMENT_3D ( 'NONE', #39059, #14352, #39672 ) ;
#38363 = CARTESIAN_POINT ( 'NONE',  ( -69.92837670882107659, -0.7829914368874778541, 9.949874371066204759 ) ) ;
#38364 = CARTESIAN_POINT ( 'NONE',  ( 80.03496335128151884, 66.36160760684386162, 1.085061034363233201 ) ) ;
#38365 = CARTESIAN_POINT ( 'NONE',  ( -63.23394756505680903, 41.82033939425821956, 3.940708880140557202 ) ) ;
#38366 = CARTESIAN_POINT ( 'NONE',  ( 25.20438522764541744, -3.119311913904994515, 5.422531462276817038 ) ) ;
#38367 = CARTESIAN_POINT ( 'NONE',  ( 4.336009428051142756, -27.42202173051807890, 6.894806418505345924 ) ) ;
#38368 = ORIENTED_EDGE ( 'NONE', *, *, #6940, .T. ) ;
#38369 = CARTESIAN_POINT ( 'NONE',  ( -74.57913178212034211, -4.413113548761699256, 9.314603197924022027 ) ) ;
#38370 = CARTESIAN_POINT ( 'NONE',  ( 26.76647965857537415, 0.8302664925678825414, -4.383954519114094950 ) ) ;
#38371 = CARTESIAN_POINT ( 'NONE',  ( -77.92837670882107659, 2.429809908903242555, -12.50000000000000000 ) ) ;
#38372 = CARTESIAN_POINT ( 'NONE',  ( -0.9900718542488416984, -31.79106902588718597, 7.781480525794717273 ) ) ;
#38373 = CARTESIAN_POINT ( 'NONE',  ( 33.45639490703039343, -3.830543181052060486, -5.092503944725620180 ) ) ;
#38374 = CARTESIAN_POINT ( 'NONE',  ( -42.83131703149249603, -32.06993018339340296, 6.800000000000000711 ) ) ;
#38375 = CARTESIAN_POINT ( 'NONE',  ( 3.738435213701987614, -32.29140130045581714, 6.895222827070023541 ) ) ;
#38376 = CARTESIAN_POINT ( 'NONE',  ( 22.27827011423021375, 5.092264179490945786, 3.633461677088038577 ) ) ;
#38377 = CARTESIAN_POINT ( 'NONE',  ( -2.227706725756020578, -32.93668375692303130, 7.695279973900954751 ) ) ;
#38378 = DIRECTION ( 'NONE',  ( -1.000000000000000000, 0.000000000000000000, 0.000000000000000000 ) ) ;
#38379 = DIRECTION ( 'NONE',  ( 1.000000000000000000, 0.000000000000000000, 0.000000000000000000 ) ) ;
#38380 = CIRCLE ( 'NONE', #9434, 12.38600677260393113 ) ;
#38381 = CARTESIAN_POINT ( 'NONE',  ( 20.40287464304303100, 10.75613383955523616, -2.500000000000000000 ) ) ;
#38382 = CIRCLE ( 'NONE', #25912, 7.341749246864647915 ) ;
#38383 = CARTESIAN_POINT ( 'NONE',  ( 24.44373853437086197, 1.125249206679775238, -4.746398584013702404 ) ) ;
#38384 = CARTESIAN_POINT ( 'NONE',  ( 33.50539668211418842, -0.3143895519534527505, -5.031603207882493045 ) ) ;
#38385 = LINE ( 'NONE', #25850, #3906 ) ;
#38386 = ORIENTED_EDGE ( 'NONE', *, *, #1916, .T. ) ;
#38387 = CARTESIAN_POINT ( 'NONE',  ( 66.56200747226770886, 57.85618981312373421, 3.999874661883398463 ) ) ;
#38388 = ADVANCED_FACE ( 'NONE', ( #12481 ), #39198, .F. ) ;
#38389 = EDGE_CURVE ( 'NONE', #18938, #24066, #32077, .T. ) ;
#38390 = CIRCLE ( 'NONE', #7485, 0.1000000000000028644 ) ;
#38391 = LINE ( 'NONE', #29147, #15469 ) ;
#38392 = CARTESIAN_POINT ( 'NONE',  ( 86.35968278939613185, 0.3242946576005459325, -6.017936684944984016 ) ) ;
#38393 = ADVANCED_FACE ( 'NONE', ( #36138 ), #7717, .T. ) ;
#38394 = CARTESIAN_POINT ( 'NONE',  ( -0.6250228819461873808, -32.05034436148299193, 7.013842709614101167 ) ) ;
#38395 = ORIENTED_EDGE ( 'NONE', *, *, #35636, .T. ) ;
#38396 = FACE_OUTER_BOUND ( 'NONE', #31448, .T. ) ;
#38397 =( LENGTH_UNIT ( ) NAMED_UNIT ( * ) SI_UNIT ( .MILLI., .METRE. ) );
#38398 = CARTESIAN_POINT ( 'NONE',  ( 2.221308981034764152, -32.92980290402432786, 7.784476445165072533 ) ) ;
#38399 = DIRECTION ( 'NONE',  ( -1.000000000000000000, -5.551115123125787751E-14, 0.000000000000000000 ) ) ;
#38400 = EDGE_LOOP ( 'NONE', ( #32995, #9072, #32053, #1886, #9992 ) ) ;
#38401 = PRESENTATION_STYLE_ASSIGNMENT (( #562 ) ) ;
#38402 = DIRECTION ( 'NONE',  ( -1.000000000000000000, 0.000000000000000000, 0.000000000000000000 ) ) ;
#38403 = EDGE_LOOP ( 'NONE', ( #27907, #24082, #1517, #36006 ) ) ;
#38404 = VERTEX_POINT ( 'NONE', #1759 ) ;
#38405 = CARTESIAN_POINT ( 'NONE',  ( 80.12334914806359620, 63.07862483458217895, -3.671038198312435163 ) ) ;
#38406 = CARTESIAN_POINT ( 'NONE',  ( 78.79414303495669003, 65.54496243571018965, 2.640205493567678641 ) ) ;
#38409 = ORIENTED_EDGE ( 'NONE', *, *, #29195, .F. ) ;
#38408 = VERTEX_POINT ( 'NONE', #39402 ) ;
#38407 = FACE_OUTER_BOUND ( 'NONE', #6305, .T. ) ;
#38410 = DIRECTION ( 'NONE',  ( -0.000000000000000000, -0.000000000000000000, 1.000000000000000000 ) ) ;
#38411 = CIRCLE ( 'NONE', #7503, 3.499999999999999556 ) ;
#38412 = CARTESIAN_POINT ( 'NONE',  ( 25.95070172733332825, 1.815565124465190250, 4.256632643280088502 ) ) ;
#38413 = CARTESIAN_POINT ( 'NONE',  ( 0.9047207686989762188, -32.97828907382665165, 6.945385021654666424 ) ) ;
#38414 = LINE ( 'NONE', #35953, #32123 ) ;
#38415 = CARTESIAN_POINT ( 'NONE',  ( 33.78722970661161185, -4.852430101419790809, -3.455127649274125190 ) ) ;
#38416 = CARTESIAN_POINT ( 'NONE',  ( 24.73483262695019391, 3.010241890163435574, -3.394196563057135130 ) ) ;
#38417 = EDGE_LOOP ( 'NONE', ( #6537, #13235, #36222, #10200 ) ) ;
#38418 = CARTESIAN_POINT ( 'NONE',  ( 5.200346560046187783, -29.55237849334843503, 7.640616322432100205 ) ) ;
#38419 = CARTESIAN_POINT ( 'NONE',  ( -1.027896628602648299, -31.59884209547612954, 6.911401339314958037 ) ) ;
#38420 = CARTESIAN_POINT ( 'NONE',  ( 3.651251297819360531, -26.64985754041175525, 6.800000000000000711 ) ) ;
#38421 = CARTESIAN_POINT ( 'NONE',  ( -73.53810101549979095, -0.8611987601447699259, -10.86982216486306640 ) ) ;
#38422 = DIRECTION ( 'NONE',  ( 0.6834397476448822450, 0.000000000000000000, 0.7300069255418744074 ) ) ;
#38423 = CARTESIAN_POINT ( 'NONE',  ( 1.700390093233090871, -29.56993018339339940, 7.800000000000000711 ) ) ;
#38424 = CARTESIAN_POINT ( 'NONE',  ( 81.39943925848319850, 61.85181198611488895, 2.332991218130497924 ) ) ;
#38425 = CARTESIAN_POINT ( 'NONE',  ( 84.36871573755720988, 2.689384369868815128, -2.914620128191189874 ) ) ;
#38426 = DIRECTION ( 'NONE',  ( -0.000000000000000000, 0.000000000000000000, 1.000000000000000000 ) ) ;
#38427 = DIRECTION ( 'NONE',  ( 0.000000000000000000, 0.000000000000000000, 1.000000000000000000 ) ) ;
#38428 = CARTESIAN_POINT ( 'NONE',  ( 21.54803796295231777, 7.333299173607420229, 1.920888206966631984 ) ) ;
#38429 = CARTESIAN_POINT ( 'NONE',  ( 0.9213240864078056092, -26.64985754041175525, 6.700000000000000178 ) ) ;
#38430 = CARTESIAN_POINT ( 'NONE',  ( -0.3434165924072999365, -26.85277739775768779, 6.887945620086119547 ) ) ;
#38431 = CARTESIAN_POINT ( 'NONE',  ( 4.664684489921304689, -27.90468147679489164, 7.784838882742139532 ) ) ;
#38432 = DIRECTION ( 'NONE',  ( 0.000000000000000000, 1.000000000000000000, 0.000000000000000000 ) ) ;
#38433 = CARTESIAN_POINT ( 'NONE',  ( 69.19640405677364470, 58.81667877646589204, 3.990151341881418290 ) ) ;
#38434 = CARTESIAN_POINT ( 'NONE',  ( 36.64647822751152262, -2.460832023537397273, 5.925967244464915851 ) ) ;
#38435 = AXIS2_PLACEMENT_3D ( 'NONE', #26449, #7497, #10977 ) ;
#38436 = CARTESIAN_POINT ( 'NONE',  ( -0.4545477510665002496, -26.81228124332190532, 7.754798119455333705 ) ) ;
#38437 = CIRCLE ( 'NONE', #34546, 0.1000000000000028644 ) ;
#38438 = CARTESIAN_POINT ( 'NONE',  ( 85.11099552155531001, 2.757014815357352155, -1.204572545719858834 ) ) ;
#38439 = ADVANCED_FACE ( 'NONE', ( #35543 ), #19680, .T. ) ;
#38440 = ORIENTED_EDGE ( 'NONE', *, *, #6540, .T. ) ;
#38442 = CARTESIAN_POINT ( 'NONE',  ( 4.818630077464289840, -30.92514033129047490, 6.979335674598001305 ) ) ;
#38441 = CARTESIAN_POINT ( 'NONE',  ( 79.17166177841365027, 65.86836750419898578, -2.393593008231246877 ) ) ;
#38443 = DIRECTION ( 'NONE',  ( -0.000000000000000000, -1.000000000000000000, -0.000000000000000000 ) ) ;
#38444 = ORIENTED_EDGE ( 'NONE', *, *, #7448, .T. ) ;
#38445 = PLANE ( 'NONE',  #23403 ) ;
#38446 = VECTOR ( 'NONE', #17932, 1000.000000000000000 ) ;
#38447 = ORIENTED_EDGE ( 'NONE', *, *, #30165, .F. ) ;
#38448 = CARTESIAN_POINT ( 'NONE',  ( -73.55543068772023219, -3.221851483746068112, 9.649644320831473721 ) ) ;
#38449 = ORIENTED_EDGE ( 'NONE', *, *, #2853, .F. ) ;
#38450 = CARTESIAN_POINT ( 'NONE',  ( 78.97848303377267598, 65.71588112483769351, -2.516896548562721492 ) ) ;
#38451 =( BOUNDED_SURFACE ( )  B_SPLINE_SURFACE ( 3, 2, ( 
 ( #33688, #1779, #29968 ),
 ( #5467, #15130, #20693 ),
 ( #30386, #36354, #17800 ),
 ( #40242, #18007, #39848 ),
 ( #30171, #36959, #20906 ),
 ( #40044, #8739, #5058 ),
 ( #11615, #1992, #30596 ),
 ( #24195, #27085, #17591 ),
 ( #11211, #11819, #11413 ),
 ( #27686, #36754, #21322 ),
 ( #12026, #23980, #24605 ),
 ( #2404, #36552, #20484 ),
 ( #37160, #8330, #33491 ),
 ( #14926, #26879, #27495 ),
 ( #33068, #4852, #14310 ),
 ( #39422, #8121, #28304 ),
 ( #22356, #21731, #3630 ),
 ( #31204, #5881, #34719 ),
 ( #321, #31006, #22147 ),
 ( #12244, #34923, #31815 ),
 ( #21531, #6699, #34313 ),
 ( #3232, #9567, #31611 ),
 ( #37758, #19047, #19248 ),
 ( #37560, #28719, #15751 ),
 ( #122, #9155, #40435 ),
 ( #6082, #25229, #16155 ),
 ( #25427, #12860, #37968 ),
 ( #531, #9355, #3434 ),
 ( #18617, #9773, #3024 ),
 ( #18418, #13066, #6498 ),
 ( #15544, #28098, #12654 ),
 ( #25627, #24818, #15947 ),
 ( #28511, #8946, #34107 ),
 ( #2811, #15333, #40652 ),
 ( #27888, #37360, #12454 ),
 ( #25023, #21936, #34510 ),
 ( #6286, #18835, #31407 ),
 ( #38573, #6895, #23345 ),
 ( #35716, #4426, #10769 ),
 ( #32026, #13677, #725 ),
 ( #16950, #38172, #32229 ),
 ( #22555, #22956, #32631 ),
 ( #4618, #3831, #38779 ),
 ( #38369, #9975, #35118 ),
 ( #16351, #13876, #20245 ),
 ( #35325, #1143, #7492 ),
 ( #16547, #4221, #28924 ),
 ( #10575, #35917, #23149 ),
 ( #20052, #19452, #13266 ),
 ( #19657, #38970, #4029 ),
 ( #7696, #25834, #1530 ),
 ( #26247, #35519, #32827 ),
 ( #26443, #10379, #29720 ),
 ( #17148, #14064, #10166 ),
 ( #22757, #7290, #7093 ),
 ( #29128, #29528, #1340 ),
 ( #931, #13465, #26039 ),
 ( #19853, #32423, #16742 ),
 ( #29326, #26838, #29919 ),
 ( #11571, #20647, #20857 ),
 ( #21071, #36310, #2561 ),
 ( #8282, #33024, #2354 ),
 ( #17752, #8695, #27041 ),
 ( #26641, #39175, #39585 ),
 ( #30133, #40001, #4814 ),
 ( #23937, #24146, #1948 ) ),
 .UNSPECIFIED., .F., .F., .F. ) 
 B_SPLINE_SURFACE_WITH_KNOTS ( ( 4, 2, 2, 2, 2, 2, 2, 2, 2, 2, 2, 2, 2, 2, 2, 2, 2, 2, 2, 2, 2, 2, 2, 2, 2, 2, 2, 2, 2, 2, 2, 2, 4 ),
 ( 3, 3 ),
 ( 0.000000000000000000, 0.002658035264796820320, 0.003987052897195230913, 0.005316070529593640639, 0.006645088161992051233, 0.007974105794390461827, 0.009303123426788871553, 0.009967632242988076416, 0.01063214105918728128, 0.01196115869158569101, 0.01262566750778489760, 0.01329017632398410247, 0.01461919395638251393, 0.01594821158878092365, 0.01727722922117933338, 0.01860624685357774311, 0.01993526448597615283, 0.02126428211837456256, 0.02392231738317138201, 0.02525133501556979521, 0.02658035264796820493, 0.02790937028036661466, 0.02923838791276502785, 0.03056740554516343758, 0.03189642317756184731, 0.03322544080996026050, 0.03455445844235866676, 0.03588347607475707302, 0.03721249370715548621, 0.03854151133955389941, 0.03987052897195230566, 0.04119954660435071192, 0.04252856423674912512 ),
 ( 0.000000000000000000, 1.000000000000000000 ),
 .UNSPECIFIED. ) 
 GEOMETRIC_REPRESENTATION_ITEM ( )  RATIONAL_B_SPLINE_SURFACE ( (
 ( 1.000000000000000000, 0.7441515679388579496, 1.000000000000000000),
 ( 1.000000000000000000, 0.7418889564077462140, 1.000000000000000000),
 ( 1.000000000000000000, 0.7352412587068134497, 1.000000000000000000),
 ( 1.000000000000000000, 0.7200556229443167977, 1.000000000000000000),
 ( 1.000000000000000000, 0.7140806601001210563, 1.000000000000000000),
 ( 1.000000000000000000, 0.7009386729189606147, 1.000000000000000000),
 ( 1.000000000000000000, 0.6938174132529958404, 1.000000000000000000),
 ( 1.000000000000000000, 0.6790697772413124556, 1.000000000000000000),
 ( 1.000000000000000000, 0.6714408432011916839, 1.000000000000000000),
 ( 1.000000000000000000, 0.6564065633759171847, 1.000000000000000000),
 ( 1.000000000000000000, 0.6489510379847600596, 1.000000000000000000),
 ( 1.000000000000000000, 0.6356113203842299608, 1.000000000000000000),
 ( 1.000000000000000000, 0.6296912164606264239, 1.000000000000000000),
 ( 1.000000000000000000, 0.6225417645797769461, 1.000000000000000000),
 ( 1.000000000000000000, 0.6204465321787280274, 1.000000000000000000),
 ( 1.000000000000000000, 0.6169216871892950760, 1.000000000000000000),
 ( 1.000000000000000000, 0.6155016171862526253, 1.000000000000000000),
 ( 1.000000000000000000, 0.6123816062328042431, 1.000000000000000000),
 ( 1.000000000000000000, 0.6117967163037434375, 1.000000000000000000),
 ( 1.000000000000000000, 0.6130028206688593606, 1.000000000000000000),
 ( 1.000000000000000000, 0.6137491082589734415, 1.000000000000000000),
 ( 1.000000000000000000, 0.6158696746842220460, 1.000000000000000000),
 ( 1.000000000000000000, 0.6172499807807707572, 1.000000000000000000),
 ( 1.000000000000000000, 0.6220975276951665744, 1.000000000000000000),
 ( 1.000000000000000000, 0.6262835279352212403, 1.000000000000000000),
 ( 1.000000000000000000, 0.6355396176620391469, 1.000000000000000000),
 ( 1.000000000000000000, 0.6406497905274252114, 1.000000000000000000),
 ( 1.000000000000000000, 0.6505234917001551098, 1.000000000000000000),
 ( 1.000000000000000000, 0.6552943981022679720, 1.000000000000000000),
 ( 1.000000000000000000, 0.6637656571438727005, 1.000000000000000000),
 ( 1.000000000000000000, 0.6674871567836762054, 1.000000000000000000),
 ( 1.000000000000000000, 0.6731590004692020734, 1.000000000000000000),
 ( 1.000000000000000000, 0.6751296496122961566, 1.000000000000000000),
 ( 1.000000000000000000, 0.6771305984922478816, 1.000000000000000000),
 ( 1.000000000000000000, 0.6771548257842952001, 1.000000000000000000),
 ( 1.000000000000000000, 0.6742147169802384932, 1.000000000000000000),
 ( 1.000000000000000000, 0.6682671589301644177, 1.000000000000000000),
 ( 1.000000000000000000, 0.6555315094090650163, 1.000000000000000000),
 ( 1.000000000000000000, 0.6507284898546285001, 1.000000000000000000),
 ( 1.000000000000000000, 0.6409367973921450412, 1.000000000000000000),
 ( 1.000000000000000000, 0.6359230196329027640, 1.000000000000000000),
 ( 1.000000000000000000, 0.6266085828807440583, 1.000000000000000000),
 ( 1.000000000000000000, 0.6223160178622464400, 1.000000000000000000),
 ( 1.000000000000000000, 0.6158161838050073555, 1.000000000000000000),
 ( 1.000000000000000000, 0.6135607247596366332, 1.000000000000000000),
 ( 1.000000000000000000, 0.6117889963409239851, 1.000000000000000000),
 ( 1.000000000000000000, 0.6123161496792929315, 1.000000000000000000),
 ( 1.000000000000000000, 0.6163584728649634803, 1.000000000000000000),
 ( 1.000000000000000000, 0.6198375735205692294, 1.000000000000000000),
 ( 1.000000000000000000, 0.6292699336656990550, 1.000000000000000000),
 ( 1.000000000000000000, 0.6352691617163160887, 1.000000000000000000),
 ( 1.000000000000000000, 0.6485718343924502527, 1.000000000000000000),
 ( 1.000000000000000000, 0.6558929686343136778, 1.000000000000000000),
 ( 1.000000000000000000, 0.6709892557901798726, 1.000000000000000000),
 ( 1.000000000000000000, 0.6787899122752630854, 1.000000000000000000),
 ( 1.000000000000000000, 0.6936905356355238528, 1.000000000000000000),
 ( 1.000000000000000000, 0.7008379245427935889, 1.000000000000000000),
 ( 1.000000000000000000, 0.7139594056183991011, 1.000000000000000000),
 ( 1.000000000000000000, 0.7199647099235089165, 1.000000000000000000),
 ( 1.000000000000000000, 0.7301796029319667092, 1.000000000000000000),
 ( 1.000000000000000000, 0.7343899733826660947, 1.000000000000000000),
 ( 1.000000000000000000, 0.7408103714601322887, 1.000000000000000000),
 ( 1.000000000000000000, 0.7430216292999781702, 1.000000000000000000),
 ( 1.000000000000000000, 0.7452812010865806913, 1.000000000000000000),
 ( 1.000000000000000000, 0.7453214615320080672, 1.000000000000000000),
 ( 1.000000000000000000, 0.7442417417348949904, 1.000000000000000000) ) ) 
 REPRESENTATION_ITEM ( '' )  SURFACE ( )  );
#38452 = DIRECTION ( 'NONE',  ( 0.000000000000000000, 0.000000000000000000, 1.000000000000000000 ) ) ;
#38453 = CARTESIAN_POINT ( 'NONE',  ( 23.12586401754871446, 1.482052930854636186, 5.229025453252686972 ) ) ;
#38455 = ORIENTED_EDGE ( 'NONE', *, *, #28206, .F. ) ;
#38454 = VERTEX_POINT ( 'NONE', #32444 ) ;
#38456 = FACE_OUTER_BOUND ( 'NONE', #40123, .T. ) ;
#38458 = CARTESIAN_POINT ( 'NONE',  ( 85.51486067931016066, 2.303374301570278782, 3.104493111481445133 ) ) ;
#38457 = CARTESIAN_POINT ( 'NONE',  ( 14.74962925723565021, 13.05063958597602713, -2.500338280337093710 ) ) ;
#38459 = CARTESIAN_POINT ( 'NONE',  ( -20.24874870218063805, -25.49307895267003587, 6.700000000000000178 ) ) ;
#38460 = CARTESIAN_POINT ( 'NONE',  ( -63.70246229030799867, 44.36789000525197224, -1.452554708948875284 ) ) ;
#38461 = CARTESIAN_POINT ( 'NONE',  ( 71.10141846075379135, 59.08792130574165924, 3.942344351592514062 ) ) ;
#38462 = EDGE_CURVE ( 'NONE', #18594, #35446, #4242, .T. ) ;
#38463 = CARTESIAN_POINT ( 'NONE',  ( 23.65021474120684175, 3.294044046464493114, -3.628962476493511335 ) ) ;
#38464 = ORIENTED_EDGE ( 'NONE', *, *, #12742, .T. ) ;
#38465 = CARTESIAN_POINT ( 'NONE',  ( -71.92837670882109080, -0.6505656586640776728, 5.916079783099611689 ) ) ;
#38466 = ORIENTED_EDGE ( 'NONE', *, *, #22423, .T. ) ;
#38467 = CARTESIAN_POINT ( 'NONE',  ( 21.85643539959777826, -3.517407513333692837, -12.34883488727242806 ) ) ;
#38468 = AXIS2_PLACEMENT_3D ( 'NONE', #28343, #22390, #5915 ) ;
#38469 = CARTESIAN_POINT ( 'NONE',  ( 17.09215160922207133, 14.51084972820098606, -1.912535534561643491 ) ) ;
#38470 = CARTESIAN_POINT ( 'NONE',  ( 1.111671518581322848, -33.02006264939198132, 7.747520101777646495 ) ) ;
#38471 = CARTESIAN_POINT ( 'NONE',  ( 81.69769846481528930, 62.77423530096622528, 2.811330881970099504 ) ) ;
#38472 = CARTESIAN_POINT ( 'NONE',  ( 87.06807637922989329, 0.009568187950425697044, -5.830412620327568796 ) ) ;
#38473 = VERTEX_POINT ( 'NONE', #32649 ) ;
#38474 = VECTOR ( 'NONE', #24215, 1000.000000000000000 ) ;
#38475 = CARTESIAN_POINT ( 'NONE',  ( 0.4368679818768612111, -32.72644202797246749, 7.768425012602594215 ) ) ;
#38476 = ORIENTED_EDGE ( 'NONE', *, *, #496, .T. ) ;
#38477 = CARTESIAN_POINT ( 'NONE',  ( 5.885943586549580608, -28.70822073431874344, 7.754798119455333705 ) ) ;
#38478 = EDGE_CURVE ( 'NONE', #28633, #15847, #16974, .T. ) ;
#38479 = CARTESIAN_POINT ( 'NONE',  ( 32.30199181244099549, -3.779839205847876027, 4.859909891667491877 ) ) ;
#38480 = CARTESIAN_POINT ( 'NONE',  ( 36.63338369844979781, -3.080224374057493719, -5.923923526512606230 ) ) ;
#38481 = CARTESIAN_POINT ( 'NONE',  ( 0.5712820523693047381, -32.77697165990360162, 7.691066658568947112 ) ) ;
#38482 = CARTESIAN_POINT ( 'NONE',  ( 84.37976216279319885, 2.675842969773557734, -2.958831758778651455 ) ) ;
#38483 = CARTESIAN_POINT ( 'NONE',  ( -73.12195409265169133, 0.3003155719458506789, 10.93237219782067093 ) ) ;
#38484 = VERTEX_POINT ( 'NONE', #11392 ) ;
#38485 = CARTESIAN_POINT ( 'NONE',  ( 3.858641814960187766, -26.94277397789914730, 7.680992449362115337 ) ) ;
#38486 = CARTESIAN_POINT ( 'NONE',  ( 3.431349736501141390, -32.49632364862963385, 7.691066658568946224 ) ) ;
#38487 = CARTESIAN_POINT ( 'NONE',  ( 33.45208957067621469, -3.251134754649326553, 5.427405637984302089 ) ) ;
#38488 = EDGE_CURVE ( 'NONE', #38156, #9413, #9067, .T. ) ;
#38489 = VERTEX_POINT ( 'NONE', #17778 ) ;
#38490 = ORIENTED_EDGE ( 'NONE', *, *, #9203, .F. ) ;
#38491 = CARTESIAN_POINT ( 'NONE',  ( 36.68486169653590423, -1.915814949631118758, 5.803682713086825373 ) ) ;
#38492 = CARTESIAN_POINT ( 'NONE',  ( -6.978675913592191193, -24.55319635012989110, 6.800000000000000711 ) ) ;
#38493 = CARTESIAN_POINT ( 'NONE',  ( 3.015109609237833332, -26.32624206733842698, 7.750000000000000888 ) ) ;
#38494 = CARTESIAN_POINT ( 'NONE',  ( 87.91312586971599785, -2.495764367860345612, 0.6122158967995121603 ) ) ;
#38495 = VERTEX_POINT ( 'NONE', #33876 ) ;
#38496 = AXIS2_PLACEMENT_3D ( 'NONE', #28787, #7156, #23015 ) ;
#38497 = VERTEX_POINT ( 'NONE', #39828 ) ;
#38498 = CARTESIAN_POINT ( 'NONE',  ( 38.29999999999999716, 0.000000000000000000, 0.000000000000000000 ) ) ;
#38499 = ORIENTED_EDGE ( 'NONE', *, *, #13641, .T. ) ;
#38500 = CARTESIAN_POINT ( 'NONE',  ( -55.43956553351897298, 30.97124788692901376, -1.442063311134004877 ) ) ;
#38501 = CARTESIAN_POINT ( 'NONE',  ( 3.802745552976189991, -32.36816203956407634, 6.980586498568969844 ) ) ;
#38502 = ORIENTED_EDGE ( 'NONE', *, *, #5494, .F. ) ;
#38503 = CARTESIAN_POINT ( 'NONE',  ( 22.25877217673135888, 4.971410982095481046, 3.249134972655711273 ) ) ;
#38504 = AXIS2_PLACEMENT_3D ( 'NONE', #32221, #35512, #22549 ) ;
#38505 = CARTESIAN_POINT ( 'NONE',  ( 81.79239483946106759, 65.43557760269889911, -1.755995906648851523 ) ) ;
#38506 = EDGE_CURVE ( 'NONE', #19029, #30413, #11595, .T. ) ;
#38507 = CARTESIAN_POINT ( 'NONE',  ( -1.233968097352797555, -31.28736617508928575, 7.643333865083958401 ) ) ;
#38508 = ORIENTED_EDGE ( 'NONE', *, *, #12109, .T. ) ;
#38509 = CARTESIAN_POINT ( 'NONE',  ( 75.74268929893177926, 62.45338499886817374, -3.784676997166835921 ) ) ;
#38511 = CARTESIAN_POINT ( 'NONE',  ( 4.448805861693501562, -27.40704168211281910, 7.766640943994347346 ) ) ;
#38510 = CARTESIAN_POINT ( 'NONE',  ( -80.92837670882107659, 2.429809908903242555, -12.50000000000000000 ) ) ;
#38512 = FACE_OUTER_BOUND ( 'NONE', #10270, .T. ) ;
#38513 = CARTESIAN_POINT ( 'NONE',  ( 77.06614703306252068, 61.11928327932300675, 3.683100983543551088 ) ) ;
#38514 = EDGE_LOOP ( 'NONE', ( #31729, #12221, #13725, #3931 ) ) ;
#38515 = CARTESIAN_POINT ( 'NONE',  ( 4.337561542305367723, -27.42392627274044514, 6.892063359921933419 ) ) ;
#38516 = CARTESIAN_POINT ( 'NONE',  ( 1.768024593811872380, -26.08451850652108206, 7.784725160561909441 ) ) ;
#38517 = CARTESIAN_POINT ( 'NONE',  ( 27.43879703630890887, 0.9604363013853572939, -4.488885905966782275 ) ) ;
#38518 = CARTESIAN_POINT ( 'NONE',  ( 78.68884106766326170, 66.05749720280910253, 1.041818241550643842 ) ) ;
#38519 = CARTESIAN_POINT ( 'NONE',  ( -0.1886652755034646245, -32.51637180025015539, 6.887547729233694405 ) ) ;
#38520 = CARTESIAN_POINT ( 'NONE',  ( 29.86640044794213011, -3.433240980530400499, 4.572246828724481738 ) ) ;
#38521 = EDGE_CURVE ( 'NONE', #28243, #614, #29708, .T. ) ;
#38522 = EDGE_CURVE ( 'NONE', #18637, #24328, #8926, .T. ) ;
#38523 = CARTESIAN_POINT ( 'NONE',  ( -1.699484971103116582, -29.59922004846627885, 7.730758795053803922 ) ) ;
#38524 = CARTESIAN_POINT ( 'NONE',  ( -70.66609929912286248, -21.75673952224967422, 9.997285688091769984 ) ) ;
#38525 = EDGE_CURVE ( 'NONE', #17878, #35921, #9028, .T. ) ;
#38526 = CARTESIAN_POINT ( 'NONE',  ( -60.75950795826495465, 23.17721540975219341, 15.50000000000000000 ) ) ;
#38527 = CARTESIAN_POINT ( 'NONE',  ( -18.87867591359219333, -26.64985754041175525, 6.700000000000000178 ) ) ;
#38528 = CIRCLE ( 'NONE', #16124, 2.500000000000000000 ) ;
#38529 = CARTESIAN_POINT ( 'NONE',  ( -1.461284153450459922, -28.05286529242975035, 7.501983001166816933 ) ) ;
#38530 = CARTESIAN_POINT ( 'NONE',  ( 34.51608426288976972, -1.013665949057833915, -5.504871762502034471 ) ) ;
#38531 = CARTESIAN_POINT ( 'NONE',  ( 1.115330424693315559, -32.91922472814544420, 7.763628509615286610 ) ) ;
#38532 = CARTESIAN_POINT ( 'NONE',  ( -0.6250228819461873808, -32.05034436148299193, 7.013842709614101167 ) ) ;
#38533 = FACE_OUTER_BOUND ( 'NONE', #1503, .T. ) ;
#38534 = CARTESIAN_POINT ( 'NONE',  ( 2.177802833585739339, -32.93624524222983752, 6.864276522220859711 ) ) ;
#38535 = AXIS2_PLACEMENT_3D ( 'NONE', #14413, #1682, #4753 ) ;
#38536 = DIRECTION ( 'NONE',  ( 0.7541618601367590102, 0.000000000000000000, 0.6566885781822794366 ) ) ;
#38537 = CARTESIAN_POINT ( 'NONE',  ( 14.77315594796849574, 13.19392823276453441, -2.500000000000005773 ) ) ;
#38538 = EDGE_LOOP ( 'NONE', ( #20936, #36243, #14445, #30894, #34979 ) ) ;
#38539 = CARTESIAN_POINT ( 'NONE',  ( 31.86209868568754544, -0.1501604454850196113, 5.152680217172298960 ) ) ;
#38540 = CARTESIAN_POINT ( 'NONE',  ( -1.237321756456247979, -31.28161037787917209, 7.635761828346577573 ) ) ;
#38541 = CARTESIAN_POINT ( 'NONE',  ( 67.73962338513339887, 58.26590004628993569, -3.997461085607390885 ) ) ;
#38542 = DIRECTION ( 'NONE',  ( 1.000000000000000000, 0.000000000000000000, 0.000000000000000000 ) ) ;
#38543 = ORIENTED_EDGE ( 'NONE', *, *, #35033, .F. ) ;
#38544 = DIRECTION ( 'NONE',  ( 1.000000000000000000, 0.000000000000000000, 0.000000000000000000 ) ) ;
#38545 = CARTESIAN_POINT ( 'NONE',  ( -1.600658481268679267, -28.40671124064021669, 7.695279973900954751 ) ) ;
#38546 = CARTESIAN_POINT ( 'NONE',  ( 23.25558064308254558, 3.168631396969136649, 3.922402285246370024 ) ) ;
#38547 = CARTESIAN_POINT ( 'NONE',  ( -58.99872204295123623, 28.48507918597066180, 6.834244957304007606 ) ) ;
#38548 = CARTESIAN_POINT ( 'NONE',  ( 1.149416566283971264, -26.21485601168476265, 7.784838882742139532 ) ) ;
#38549 = CARTESIAN_POINT ( 'NONE',  ( -56.34850605459112671, 30.68671187671609246, 2.749655849400831187 ) ) ;
#38550 = EDGE_LOOP ( 'NONE', ( #471, #25311, #39439, #19036 ) ) ;
#38551 = CARTESIAN_POINT ( 'NONE',  ( 24.40511021066326336, 3.163327161787246933, 3.272226049981214135 ) ) ;
#38552 = CARTESIAN_POINT ( 'NONE',  ( -1.740577464315611778, -30.21005312756170014, 7.720710062488897130 ) ) ;
#38553 = CARTESIAN_POINT ( 'NONE',  ( 80.17018276713265834, 64.56786917328069819, 3.540619799101248244 ) ) ;
#38554 = CARTESIAN_POINT ( 'NONE',  ( 0.4825641552805304269, -26.28863138271496069, 7.743886751744252450 ) ) ;
#38555 = ORIENTED_EDGE ( 'NONE', *, *, #33408, .F. ) ;
#38556 = CARTESIAN_POINT ( 'NONE',  ( 79.25863321418395913, 62.43675908411265141, -3.670385203786648454 ) ) ;
#38558 = CARTESIAN_POINT ( 'NONE',  ( 5.060299201773582389, -28.56549731252922442, 7.387053503561886281 ) ) ;
#38557 = CARTESIAN_POINT ( 'NONE',  ( 23.59267417321471427, 0.4265057547314817232, 5.522590887384096092 ) ) ;
#38559 = VECTOR ( 'NONE', #34184, 1000.000000000000000 ) ;
#38560 = CARTESIAN_POINT ( 'NONE',  ( 81.58232553940138132, 62.71761900943698009, -2.892908819258012798 ) ) ;
#38561 = CARTESIAN_POINT ( 'NONE',  ( 80.42502267531087057, 61.03612496587228975, 1.832491541757258258 ) ) ;
#38562 = CIRCLE ( 'NONE', #13594, 0.1000000000000028644 ) ;
#38563 = ORIENTED_EDGE ( 'NONE', *, *, #1249, .F. ) ;
#38564 = EDGE_CURVE ( 'NONE', #12896, #35515, #19597, .T. ) ;
#38565 = AXIS2_PLACEMENT_3D ( 'NONE', #30867, #5326, #39904 ) ;
#38566 = DIRECTION ( 'NONE',  ( -0.6427876096865430267, 0.7660444431189749048, -0.000000000000000000 ) ) ;
#38567 = EDGE_CURVE ( 'NONE', #31406, #11548, #27870, .T. ) ;
#38568 = CARTESIAN_POINT ( 'NONE',  ( 80.38645948019593845, 66.31981033314002616, 1.103079483641125069 ) ) ;
#38569 = CARTESIAN_POINT ( 'NONE',  ( -63.08758708074093136, 41.04287353446839148, 4.000000000000000000 ) ) ;
#38570 = CARTESIAN_POINT ( 'NONE',  ( 22.63837051618441620, -3.414681707391253429, 8.302592004085083133 ) ) ;
#38571 = CARTESIAN_POINT ( 'NONE',  ( -63.23359472962059158, 35.57513467056950418, -6.582177359051184062 ) ) ;
#38572 = VERTEX_POINT ( 'NONE', #8721 ) ;
#38573 = CARTESIAN_POINT ( 'NONE',  ( -72.46102572804289821, -1.248168175329565255, 9.882956611723583862 ) ) ;
#38574 = CARTESIAN_POINT ( 'NONE',  ( 26.76858707236903712, 0.8094380621706002144, -4.384283432004588477 ) ) ;
#38575 = EDGE_CURVE ( 'NONE', #37640, #10191, #38799, .T. ) ;
#38576 = DIRECTION ( 'NONE',  ( -1.000000000000000000, -0.000000000000000000, -0.000000000000000000 ) ) ;
#38577 = CARTESIAN_POINT ( 'NONE',  ( 25.01091293555841233, 3.329590545877085805, 1.936828124349011526 ) ) ;
#38578 = CARTESIAN_POINT ( 'NONE',  ( 36.68540230263305801, -1.915051275179609380, -5.803267592155077814 ) ) ;
#38579 = CARTESIAN_POINT ( 'NONE',  ( 3.364053381479577443, -33.98248085747043490, 7.695279973900954751 ) ) ;
#38580 = CARTESIAN_POINT ( 'NONE',  ( 8.290806648384990041, -35.94265729135299381, -2.500000000000000444 ) ) ;
#38581 = CARTESIAN_POINT ( 'NONE',  ( 5.108578917255564456, -30.36632773413393593, 6.961115707816237119 ) ) ;
#38582 = CARTESIAN_POINT ( 'NONE',  ( 5.198488150005315944, -29.68529909257772204, 6.865482280155367434 ) ) ;
#38583 = CARTESIAN_POINT ( 'NONE',  ( 5.012114302463782423, -30.72325263940121332, 7.255881584735163869 ) ) ;
#38584 = CARTESIAN_POINT ( 'NONE',  ( -42.44874870218064444, -25.49307895267003587, 6.800000000000000711 ) ) ;
#38585 = AXIS2_PLACEMENT_3D ( 'NONE', #26536, #10071, #23446 ) ;
#38586 = LINE ( 'NONE', #19467, #37472 ) ;
#38587 = CARTESIAN_POINT ( 'NONE',  ( 21.89213072762610679, 0.4842128809993961336, -7.752462955432138259 ) ) ;
#38588 = CARTESIAN_POINT ( 'NONE',  ( 30.52514172340196907, 0.8294708601856738417, -4.428110633612789115 ) ) ;
#38589 = CARTESIAN_POINT ( 'NONE',  ( -6.448748702180637338, -26.64985754041175525, 6.700000000000000178 ) ) ;
#38590 = CARTESIAN_POINT ( 'NONE',  ( 2.262617859748651483, -33.02448960739329920, 6.880608371227950215 ) ) ;
#38591 = ORIENTED_EDGE ( 'NONE', *, *, #21900, .F. ) ;
#38592 = ORIENTED_EDGE ( 'NONE', *, *, #21724, .T. ) ;
#38593 = CARTESIAN_POINT ( 'NONE',  ( 66.73521764480442187, 57.83500309307840581, 3.999076693781861813 ) ) ;
#38594 = CIRCLE ( 'NONE', #23503, 3.499999999999999556 ) ;
#38595 = AXIS2_PLACEMENT_3D ( 'NONE', #15715, #18387, #21499 ) ;
#38596 = CARTESIAN_POINT ( 'NONE',  ( -64.08758708074093136, 38.34280096101142732, 3.014656224624933323 ) ) ;
#38597 = CARTESIAN_POINT ( 'NONE',  ( 84.80660115723814840, 2.320002077609508717, 4.142190259225312587 ) ) ;
#38598 = CARTESIAN_POINT ( 'NONE',  ( -1.423139387634945630, -28.22694525714970837, 7.006423389747790331 ) ) ;
#38599 = ORIENTED_EDGE ( 'NONE', *, *, #33763, .T. ) ;
#38600 = CARTESIAN_POINT ( 'NONE',  ( -74.96765229735504477, 7.901165263090923929, -10.49888776350863040 ) ) ;
#38601 = DIRECTION ( 'NONE',  ( 0.000000000000000000, 0.000000000000000000, 1.000000000000000000 ) ) ;
#38602 = CARTESIAN_POINT ( 'NONE',  ( 3.011115207906999380, -26.32487479661073948, 7.754798119455333705 ) ) ;
#38603 = CARTESIAN_POINT ( 'NONE',  ( 38.29999999999999716, 2.500000000000000000, 0.000000000000000000 ) ) ;
#38604 = ORIENTED_EDGE ( 'NONE', *, *, #33806, .F. ) ;
#38605 = DIRECTION ( 'NONE',  ( 1.000000000000000000, -0.000000000000000000, 0.000000000000000000 ) ) ;
#38606 = VERTEX_POINT ( 'NONE', #26616 ) ;
#38607 = ORIENTED_EDGE ( 'NONE', *, *, #18400, .T. ) ;
#38608 = CARTESIAN_POINT ( 'NONE',  ( 80.44027647058022978, 62.28541378099806280, -3.311815948186457970 ) ) ;
#38609 = CARTESIAN_POINT ( 'NONE',  ( 33.77557131158557269, -4.800086674967288580, 3.580757159575843396 ) ) ;
#38610 = CARTESIAN_POINT ( 'NONE',  ( 80.59739669508314819, 62.32949743464991599, 3.275607309966489300 ) ) ;
#38611 = CARTESIAN_POINT ( 'NONE',  ( -83.92837670882109080, 2.429809908903242999, -12.50000000000000000 ) ) ;
#38612 = FACE_OUTER_BOUND ( 'NONE', #35518, .T. ) ;
#38613 = DIRECTION ( 'NONE',  ( 0.000000000000000000, 0.000000000000000000, 1.000000000000000000 ) ) ;
#38614 = DIRECTION ( 'NONE',  ( 0.000000000000000000, 1.000000000000000000, 0.000000000000000000 ) ) ;
#38615 = B_SPLINE_CURVE_WITH_KNOTS ( 'NONE', 3,
 ( #21814, #3109, #15629, #28178, #3, #12534, #25316, #9441, #6376, #18924, #3315, #37847, #9651, #22237, #639, #31929, #3736, #19566, #10281, #19356, #22664, #16259, #25740, #38281, #16460, #10078, #29033, #35229, #837, #13369, #39023, #3688, #6952, #4277, #23202, #38231, #10028, #16801, #22611, #35179, #32090, #3894, #16409, #28984, #787, #8133, #17205, #33696, #20704, #14117, #29976, #26696, #40055, #39231, #29771 ),
 .UNSPECIFIED., .F., .F.,
 ( 4, 1, 1, 1, 1, 2, 2, 1, 1, 1, 1, 1, 1, 2, 2, 1, 1, 1, 1, 2, 2, 1, 1, 1, 1, 1, 1, 1, 1, 2, 2, 1, 1, 1, 1, 1, 1, 2, 2, 1, 1, 1, 4 ),
 ( 0.000000000000000000, 0.08647898122975995749, 0.1080987265372002210, 0.1189085991909197421, 0.1243135355177801410, 0.1249891525586373786, 0.1251580568188523090, 0.1253269610790672672, 0.1256647695994971836, 0.1270160036812162940, 0.1297184718446550700, 0.1729579624596754572, 0.1837678351134310606, 0.1864703032768696978, 0.1891727714403083349, 0.1945777077671867750, 0.2161974530747031165, 0.2378171983822194580, 0.2486270710359776148, 0.2499783051176977522, 0.2503161136381279461, 0.2506539221585581401, 0.2513295391994198602, 0.2540320073628683506, 0.2594369436897639436, 0.3459159249200896569, 0.3675356702276709187, 0.3729406065545658455, 0.3742918406362890638, 0.3749674576771503398, 0.3753052661975809223, 0.3756430747180115048, 0.3783455428814596622, 0.3891554155352489608, 0.4323949061504016034, 0.4756343967655542460, 0.4972541420731305672, 0.4999566102365775588, 0.5013078443183011101, 0.5026590784000246614, 0.5080640147269191997, 0.5188738873807084984, 0.6918318498413339457 ),
 .UNSPECIFIED. ) ;
#38616 = LINE ( 'NONE', #18076, #26553 ) ;
#38617 = CARTESIAN_POINT ( 'NONE',  ( 21.85643539959778892, -12.39743456692229628, -10.22857181343751520 ) ) ;
#38619 = DIRECTION ( 'NONE',  ( 1.000000000000000000, 0.000000000000000000, 0.000000000000000000 ) ) ;
#38618 = VECTOR ( 'NONE', #32831, 1000.000000000000227 ) ;
#38620 = CARTESIAN_POINT ( 'NONE',  ( 23.75175095104303225, 3.571146634990261415, -3.154077189411854665 ) ) ;
#38621 = VERTEX_POINT ( 'NONE', #38547 ) ;
#38622 = DIRECTION ( 'NONE',  ( -0.000000000000000000, -0.000000000000000000, 1.000000000000000000 ) ) ;
#38623 = VECTOR ( 'NONE', #30574, 1000.000000000000000 ) ;
#38624 = EDGE_CURVE ( 'NONE', #14639, #26823, #36838, .T. ) ;
#38625 = EDGE_CURVE ( 'NONE', #23856, #38408, #22134, .T. ) ;
#38626 = CARTESIAN_POINT ( 'NONE',  ( 1.826415646469069731, -26.07219983930859897, 7.750000000000000888 ) ) ;
#38627 = CARTESIAN_POINT ( 'NONE',  ( -0.5359795030213230227, -32.26226207767182785, 7.750000000000001776 ) ) ;
#38628 = EDGE_CURVE ( 'NONE', #7900, #17955, #35496, .T. ) ;
#38629 = CARTESIAN_POINT ( 'NONE',  ( -72.05796840954714355, -0.01142228043888725460, -9.936409781712523426 ) ) ;
#38630 = DIRECTION ( 'NONE',  ( -0.000000000000000000, -0.000000000000000000, -1.000000000000000000 ) ) ;
#38631 = DIRECTION ( 'NONE',  ( 1.000000000000000000, 0.000000000000000000, 0.000000000000000000 ) ) ;
#38632 = CARTESIAN_POINT ( 'NONE',  ( 79.45632949585316851, 65.80330994668891265, 2.596981798947342934 ) ) ;
#38633 = CARTESIAN_POINT ( 'NONE',  ( 87.90619863186083194, -2.144287391213948624, -2.780224877855328014 ) ) ;
#38634 = LINE ( 'NONE', #28981, #28586 ) ;
#38635 = CARTESIAN_POINT ( 'NONE',  ( -1.578505209958239064, -30.79420367845479234, 7.730015791551944737 ) ) ;
#38636 = CARTESIAN_POINT ( 'NONE',  ( 3.922483456672744673, -26.86580350659783178, 7.695279973900954751 ) ) ;
#38637 = LINE ( 'NONE', #38429, #16437 ) ;
#38638 = CARTESIAN_POINT ( 'NONE',  ( -0.4045127432807891776, -26.89981875494305896, 6.864651958020304257 ) ) ;
#38639 = CARTESIAN_POINT ( 'NONE',  ( 4.884195952716768652, -28.37687517664920023, 7.721096864323903297 ) ) ;
#38640 = CARTESIAN_POINT ( 'NONE',  ( -1.654432145176447877, -28.54863573104451291, 7.139344958878412584 ) ) ;
#38641 = CIRCLE ( 'NONE', #12338, 0.1000000000000028644 ) ;
#38642 = CARTESIAN_POINT ( 'NONE',  ( 34.77309709234581447, -3.162889125028089055, 5.633580810428385099 ) ) ;
#38643 = CARTESIAN_POINT ( 'NONE',  ( 85.93841924537714760, 1.827613216861550205, 4.619486236290579306 ) ) ;
#38645 = CARTESIAN_POINT ( 'NONE',  ( 4.821622712055471105, -30.91823983726953529, 6.911401339314952708 ) ) ;
#38644 = CARTESIAN_POINT ( 'NONE',  ( 81.12411360294466078, 61.28734817074503383, -1.205449537698830564 ) ) ;
#38646 = CARTESIAN_POINT ( 'NONE',  ( -1.231427077925708824, -27.65826548145907893, 6.931070083220557621 ) ) ;
#38647 = AXIS2_PLACEMENT_3D ( 'NONE', #11078, #20157, #23649 ) ;
#38648 = B_SPLINE_CURVE_WITH_KNOTS ( 'NONE', 3,
 ( #10350, #35489, #38943, #35689, #7865, #19824, #26608, #23120, #16919, #17118 ),
 .UNSPECIFIED., .F., .F.,
 ( 4, 3, 3, 4 ),
 ( 0.0002170292169044793886, 0.0002420761345915981521, 0.0002723302478207042686, 0.0002816811360866789153 ),
 .UNSPECIFIED. ) ;
#38649 = CARTESIAN_POINT ( 'NONE',  ( -56.22749146662677333, 30.67773648377099960, 3.904540345294678527 ) ) ;
#38650 = ORIENTED_EDGE ( 'NONE', *, *, #25531, .T. ) ;
#38651 = CARTESIAN_POINT ( 'NONE',  ( 4.976842733950423536, -28.33913446795707358, 7.695279973900954751 ) ) ;
#38652 = ORIENTED_EDGE ( 'NONE', *, *, #2886, .F. ) ;
#38653 = CARTESIAN_POINT ( 'NONE',  ( -89.20959394718985891, -30.27593629695115496, 6.954324564059724878 ) ) ;
#38654 = ORIENTED_EDGE ( 'NONE', *, *, #32705, .T. ) ;
#38655 = CARTESIAN_POINT ( 'NONE',  ( 80.99344733541398966, 61.93321701578152272, -2.778975589575374272 ) ) ;
#38656 = CARTESIAN_POINT ( 'NONE',  ( 24.94969356037918828, 3.454325501316659608, -1.299993212727057479 ) ) ;
#38657 = CARTESIAN_POINT ( 'NONE',  ( 25.02958830711385829, 2.171333288770124881, 4.140797983151394135 ) ) ;
#38659 = ORIENTED_EDGE ( 'NONE', *, *, #12109, .F. ) ;
#38658 = ORIENTED_EDGE ( 'NONE', *, *, #7722, .F. ) ;
#38660 = CYLINDRICAL_SURFACE ( 'NONE', #12761, 1.000000000000000888 ) ;
#38661 = VECTOR ( 'NONE', #11565, 1000.000000000000114 ) ;
#38663 = CARTESIAN_POINT ( 'NONE',  ( 85.37176321662279577, 2.464108163476022018, 2.465283846017703340 ) ) ;
#38662 = CARTESIAN_POINT ( 'NONE',  ( 4.617590328857891002, -31.31634092226461163, 6.889465824494259927 ) ) ;
#38664 = DIRECTION ( 'NONE',  ( -0.000000000000000000, -1.000000000000000000, -0.000000000000000000 ) ) ;
#38665 = CARTESIAN_POINT ( 'NONE',  ( -30.34874870218063947, -25.49307895267003587, 6.800000000000000711 ) ) ;
#38666 = CARTESIAN_POINT ( 'NONE',  ( 70.93434718597480071, 59.50194243796293136, 3.976054184260643609 ) ) ;
#38667 = ORIENTED_EDGE ( 'NONE', *, *, #12594, .F. ) ;
#38668 = CARTESIAN_POINT ( 'NONE',  ( 23.01179671817061845, 3.457809282331678169, -3.829885419034514626 ) ) ;
#38669 = VERTEX_POINT ( 'NONE', #14041 ) ;
#38670 = CARTESIAN_POINT ( 'NONE',  ( -71.80167951437309171, -0.2784832644296509896, 5.936322957303396208 ) ) ;
#38671 = ORIENTED_EDGE ( 'NONE', *, *, #30559, .T. ) ;
#38672 = CARTESIAN_POINT ( 'NONE',  ( 21.85643539959776049, -12.91308397612913161, -3.835380774090566103 ) ) ;
#38674 = EDGE_CURVE ( 'NONE', #40423, #13186, #10548, .T. ) ;
#38673 = CARTESIAN_POINT ( 'NONE',  ( 21.26333942293403467, 9.593021065652562740, 2.042309770454811435 ) ) ;
#38675 = ORIENTED_EDGE ( 'NONE', *, *, #10916, .T. ) ;
#38676 = CARTESIAN_POINT ( 'NONE',  ( -10.34874870218063769, -26.64985754041175525, 6.700000000000000178 ) ) ;
#38677 = CARTESIAN_POINT ( 'NONE',  ( 81.60486409337941893, 61.94451848015731343, 2.198649373794019812 ) ) ;
#38678 = CARTESIAN_POINT ( 'NONE',  ( 85.76961320806377387, 1.955528254085527662, 4.811735575706960866 ) ) ;
#38679 = VERTEX_POINT ( 'NONE', #32208 ) ;
#38680 = CARTESIAN_POINT ( 'NONE',  ( -81.73423472054517447, -5.610403504835165478, 1.501100129317205489 ) ) ;
#38681 = AXIS2_PLACEMENT_3D ( 'NONE', #31873, #3684, #16208 ) ;
#38682 = CARTESIAN_POINT ( 'NONE',  ( 23.84321753579541081, -2.715127441814079834, 3.927708765492790022 ) ) ;
#38683 = CARTESIAN_POINT ( 'NONE',  ( 5.078860115546572018, -29.18790842463809199, 6.949473656533217358 ) ) ;
#38684 = CARTESIAN_POINT ( 'NONE',  ( 33.95462147649067930, -3.429569851476566011, -5.493391470225660989 ) ) ;
#38685 = CARTESIAN_POINT ( 'NONE',  ( 36.78903429469688291, -3.040829720014896154, -5.948216566480869716 ) ) ;
#38686 = CARTESIAN_POINT ( 'NONE',  ( -6.348748702180634140, -25.49307895267003587, 6.700000000000000178 ) ) ;
#38687 = CARTESIAN_POINT ( 'NONE',  ( 84.11150843037509617, 3.004017517549075311, -0.5155748138339447673 ) ) ;
#38688 = CARTESIAN_POINT ( 'NONE',  ( 4.077110055691020918, -27.00064969655394620, 7.013842709614101167 ) ) ;
#38689 = DIRECTION ( 'NONE',  ( 1.000000000000000000, 6.106796269766979397E-16, 0.000000000000000000 ) ) ;
#38690 = CARTESIAN_POINT ( 'NONE',  ( 28.33744289130897442, -3.843786207261427723, 4.468846400079240055 ) ) ;
#38691 = AXIS2_PLACEMENT_3D ( 'NONE', #8086, #30965, #8700 ) ;
#38692 = VERTEX_POINT ( 'NONE', #4007 ) ;
#38693 = VERTEX_POINT ( 'NONE', #23126 ) ;
#38694 = CARTESIAN_POINT ( 'NONE',  ( 36.87144894572305986, -2.086539832640053049, 5.863895186686348460 ) ) ;
#38695 =( BOUNDED_CURVE ( )  B_SPLINE_CURVE ( 3, ( #8286, #8083, #26446, #1740 ),
 .UNSPECIFIED., .F., .T. ) 
 B_SPLINE_CURVE_WITH_KNOTS ( ( 4, 4 ),
 ( 1.347909859412853795, 1.396263401595456477 ),
 .UNSPECIFIED. ) 
 CURVE ( )  GEOMETRIC_REPRESENTATION_ITEM ( )  RATIONAL_B_SPLINE_CURVE ( ( 1.000000000000000000, 0.9998051707368829089, 0.9998051707368829089, 1.000000000000000000 ) ) 
 REPRESENTATION_ITEM ( '' )  );
#38696 = CARTESIAN_POINT ( 'NONE',  ( -1.648992718206064190, -30.58562869017961816, 6.971170733404099096 ) ) ;
#38697 = EDGE_CURVE ( 'NONE', #31392, #11306, #29489, .T. ) ;
#38698 = CARTESIAN_POINT ( 'NONE',  ( -63.03213158086148837, 38.26878225442760595, -4.032857076800604901 ) ) ;
#38699 = CARTESIAN_POINT ( 'NONE',  ( 87.07401102672321258, -1.450421667693342798, 4.784145908967932570 ) ) ;
#38700 = B_SPLINE_CURVE_WITH_KNOTS ( 'NONE', 5,
 ( #24985, #19207, #37519, #9119, #16113, #6856, #31569, #34470 ),
 .UNSPECIFIED., .F., .F.,
 ( 6, 2, 6 ),
 ( 0.000000000000000000, 0.5000000000000000000, 1.000000000000000000 ),
 .UNSPECIFIED. ) ;
#38701 = ORIENTED_EDGE ( 'NONE', *, *, #18864, .F. ) ;
#38702 = CARTESIAN_POINT ( 'NONE',  ( -64.08758708074094557, 36.44316031593082528, -3.600279212593069378 ) ) ;
#38703 = DIRECTION ( 'NONE',  ( 1.000000000000000000, 0.000000000000000000, 0.000000000000000000 ) ) ;
#38704 = VERTEX_POINT ( 'NONE', #26816 ) ;
#38705 = CARTESIAN_POINT ( 'NONE',  ( -56.76293260130697860, 30.10808691202855414, -4.002692287617906075 ) ) ;
#38706 = CARTESIAN_POINT ( 'NONE',  ( 3.876975877821416283, -32.31083862995539135, 6.863805608295730387 ) ) ;
#38707 = EDGE_LOOP ( 'NONE', ( #12901, #2435, #38816, #33351 ) ) ;
#38708 = CARTESIAN_POINT ( 'NONE',  ( 23.18984300410216903, 3.594347016654975135, 3.590839796171831910 ) ) ;
#38709 = CARTESIAN_POINT ( 'NONE',  ( 80.87103490326487076, 66.01227193428218243, -1.936735430446280937 ) ) ;
#38710 = CIRCLE ( 'NONE', #24251, 15.73502530973474478 ) ;
#38711 = EDGE_CURVE ( 'NONE', #8281, #24389, #27210, .T. ) ;
#38712 = DIRECTION ( 'NONE',  ( 0.000000000000000000, 0.000000000000000000, 1.000000000000000000 ) ) ;
#38713 = ORIENTED_EDGE ( 'NONE', *, *, #19206, .T. ) ;
#38714 = CARTESIAN_POINT ( 'NONE',  ( 75.51044298776172070, 62.93595297499962271, -3.562065002326785468 ) ) ;
#38716 = CARTESIAN_POINT ( 'NONE',  ( 0.8807958757747543777, 0.5999999999999995337, -3.993526596136941720 ) ) ;
#38715 = CARTESIAN_POINT ( 'NONE',  ( 2.477620004848760882, -26.15731123158247939, 6.898188844117810525 ) ) ;
#38717 = DIRECTION ( 'NONE',  ( 0.000000000000000000, 0.000000000000000000, 1.000000000000000000 ) ) ;
#38718 = CARTESIAN_POINT ( 'NONE',  ( 75.58676173236693785, 62.77776356238128130, 3.642592851537399312 ) ) ;
#38719 = CARTESIAN_POINT ( 'NONE',  ( -2.259411375784011078, -32.74946780922542899, 7.013842709614101167 ) ) ;
#38720 = LINE ( 'NONE', #35269, #27370 ) ;
#38722 = ADVANCED_FACE ( 'NONE', ( #30515 ), #11544, .F. ) ;
#38721 = CARTESIAN_POINT ( 'NONE',  ( 24.17959102519681736, 2.679401842515043430, -3.980207983737488409 ) ) ;
#38723 = CARTESIAN_POINT ( 'NONE',  ( 1.666174409104983711, -26.07009584004536862, 7.674970859709602244 ) ) ;
#38724 = B_SPLINE_CURVE_WITH_KNOTS ( 'NONE', 3,
 ( #13702, #4640, #17173, #26268, #38803, #10196, #22781, #23172, #29742, #35739 ),
 .UNSPECIFIED., .F., .F.,
 ( 4, 3, 3, 4 ),
 ( 0.0001585009270395723623, 0.0001815657551981830558, 0.0002118214035944115297, 0.0002170292169044746994 ),
 .UNSPECIFIED. ) ;
#38725 = CARTESIAN_POINT ( 'NONE',  ( 82.09872185058188165, 62.41535711091003691, 1.944145319385261583 ) ) ;
#38726 = CARTESIAN_POINT ( 'NONE',  ( 85.94962389285764459, 1.815027625006768730, -4.252598035848374813 ) ) ;
#38727 = CARTESIAN_POINT ( 'NONE',  ( 31.71671097226645131, -1.585248588153130855, -6.002663613118158992 ) ) ;
#38728 = CARTESIAN_POINT ( 'NONE',  ( 2.293614927405436266, -26.22208247238246059, 7.769368695748487319 ) ) ;
#38729 = CARTESIAN_POINT ( 'NONE',  ( -2.503969810797764151, -28.81487718949574983, 7.635761828346577573 ) ) ;
#38730 = CYLINDRICAL_SURFACE ( 'NONE', #12356, 3.399999999999999911 ) ;
#38731 = CARTESIAN_POINT ( 'NONE',  ( 0.6752622430376749030, -26.32815398958332409, 6.868387053540520704 ) ) ;
#38732 = DIRECTION ( 'NONE',  ( -0.000000000000000000, -1.000000000000000000, -0.000000000000000000 ) ) ;
#38733 = CARTESIAN_POINT ( 'NONE',  ( 35.97288949415787584, -1.842364254675447066, -5.810895595490718435 ) ) ;
#38734 = LINE ( 'NONE', #32388, #20684 ) ;
#38735 = CARTESIAN_POINT ( 'NONE',  ( 4.715819433959782536, -31.34677736058242559, 6.894806418505347700 ) ) ;
#38736 = DIRECTION ( 'NONE',  ( -0.000000000000000000, -1.000000000000000000, -0.000000000000000000 ) ) ;
#38737 = CARTESIAN_POINT ( 'NONE',  ( -63.61759533396914179, 43.90016037724900144, -2.585133859511243859 ) ) ;
#38738 = FACE_OUTER_BOUND ( 'NONE', #2840, .T. ) ;
#38739 = VECTOR ( 'NONE', #29130, 1000.000000000000000 ) ;
#38740 = EDGE_CURVE ( 'NONE', #39064, #9395, #2324, .T. ) ;
#38741 = DIRECTION ( 'NONE',  ( -0.000000000000000000, -0.000000000000000000, 1.000000000000000000 ) ) ;
#38742 = CARTESIAN_POINT ( 'NONE',  ( 6.126843302897349020, -31.19539656904077418, 7.635761828346577573 ) ) ;
#38743 = VERTEX_POINT ( 'NONE', #24115 ) ;
#38744 = CARTESIAN_POINT ( 'NONE',  ( 37.14562426157099395, -2.766377302884501344, 6.000546555870065468 ) ) ;
#38745 = B_SPLINE_CURVE_WITH_KNOTS ( 'NONE', 3,
 ( #7351, #19515, #20299, #35972, #4279, #994, #17005, #25894, #32685, #16602, #19908, #10631 ),
 .UNSPECIFIED., .F., .F.,
 ( 4, 2, 2, 2, 2, 4 ),
 ( 0.0002778957232965137826, 0.001623504286842941766, 0.002969112850389369479, 0.005660329977482225772, 0.008351547104575083799, 0.01104276423166794183 ),
 .UNSPECIFIED. ) ;
#38746 = DIRECTION ( 'NONE',  ( -0.2567910337120223874, -0.7055275666422197167, 0.6605219282605379050 ) ) ;
#38747 = CARTESIAN_POINT ( 'NONE',  ( 67.43935760634008147, 58.17964655298460741, -3.998402061830689025 ) ) ;
#38748 = DIRECTION ( 'NONE',  ( 0.000000000000000000, 0.000000000000000000, 1.000000000000000000 ) ) ;
#38749 = ORIENTED_EDGE ( 'NONE', *, *, #21406, .F. ) ;
#38750 = FACE_OUTER_BOUND ( 'NONE', #31090, .T. ) ;
#38751 = VECTOR ( 'NONE', #31104, 1000.000000000000000 ) ;
#38752 = CARTESIAN_POINT ( 'NONE',  ( 30.80517229667822932, -3.346871776499003470, 4.960489240099761332 ) ) ;
#38753 = CARTESIAN_POINT ( 'NONE',  ( 84.80999693743234502, 2.128580961947359462, -4.467585834308593462 ) ) ;
#38754 = CARTESIAN_POINT ( 'NONE',  ( 0.9044146924870181126, -32.87544423742601651, 6.959317978105164393 ) ) ;
#38755 = EDGE_CURVE ( 'NONE', #10538, #24333, #9433, .T. ) ;
#38756 = ADVANCED_FACE ( 'NONE', ( #29897, #39975, #40720 ), #39558, .T. ) ;
#38757 = CARTESIAN_POINT ( 'NONE',  ( 0.3289290232599537123, -32.79003885831642862, 6.984548363133216142 ) ) ;
#38758 = DIRECTION ( 'NONE',  ( 1.000000000000000000, 0.000000000000000000, 0.000000000000000000 ) ) ;
#38759 = ORIENTED_EDGE ( 'NONE', *, *, #40073, .T. ) ;
#38760 = EDGE_CURVE ( 'NONE', #3867, #833, #11342, .T. ) ;
#38761 = CARTESIAN_POINT ( 'NONE',  ( 21.98982740266793456, 5.607487361672509607, 3.095612616452370514 ) ) ;
#38762 = CARTESIAN_POINT ( 'NONE',  ( -1.740020712282138948, -30.21302698773406803, 7.698786668945015954 ) ) ;
#38763 = CARTESIAN_POINT ( 'NONE',  ( 80.49748116766495798, 63.97695225015618803, 3.602832836245131620 ) ) ;
#38764 = DIRECTION ( 'NONE',  ( -0.6427876096865430267, 0.7660444431189749048, -0.000000000000000000 ) ) ;
#38765 = ORIENTED_EDGE ( 'NONE', *, *, #7347, .T. ) ;
#38766 = CARTESIAN_POINT ( 'NONE',  ( 78.58588809754505178, 64.79968573292298117, -3.228498513792966040 ) ) ;
#38768 = CARTESIAN_POINT ( 'NONE',  ( -1.733656465401150149, -28.89360903037850292, 6.868650645600655302 ) ) ;
#38767 = CARTESIAN_POINT ( 'NONE',  ( 25.38030252091800065, 0.7242675303424039868, 4.602055157131172969 ) ) ;
#38769 = CARTESIAN_POINT ( 'NONE',  ( 79.25461589595286682, 66.09583247779735871, -1.930361577749150515 ) ) ;
#38770 = CARTESIAN_POINT ( 'NONE',  ( 80.35854813638249539, 61.23284135048810839, 2.372109611208351510 ) ) ;
#38771 = VECTOR ( 'NONE', #10608, 1000.000000000000000 ) ;
#38772 = CARTESIAN_POINT ( 'NONE',  ( -81.90664279350785648, 11.45717611192839591, 0.6911394749367770762 ) ) ;
#38773 = EDGE_CURVE ( 'NONE', #15750, #30676, #28112, .T. ) ;
#38774 = CARTESIAN_POINT ( 'NONE',  ( 78.69031774315027405, 66.05854625464691310, 1.008685033153497335 ) ) ;
#38775 = CARTESIAN_POINT ( 'NONE',  ( -64.08758708074091714, 43.73155672946558781, 2.304326576497605306 ) ) ;
#38776 = CARTESIAN_POINT ( 'NONE',  ( 22.76577552469399990, -5.388071312449273620, 6.143773694815460651 ) ) ;
#38777 = CARTESIAN_POINT ( 'NONE',  ( -64.30032790741503845, 34.77233229845787577, -5.249462333892792820 ) ) ;
#38778 = VERTEX_POINT ( 'NONE', #33818 ) ;
#38779 = CARTESIAN_POINT ( 'NONE',  ( -75.05072613888007993, -3.128072587506124602, 10.46819543870325475 ) ) ;
#38780 = CARTESIAN_POINT ( 'NONE',  ( 21.73379047671751962, 0.2086737143224493274, -9.125075291706918890 ) ) ;
#38781 = B_SPLINE_CURVE_WITH_KNOTS ( 'NONE', 3,
 ( #28985, #13317, #13738, #19514, #1202, #37826, #28580, #9631, #25490, #16015, #19308, #25689, #19714, #35384, #389, #6560, #22412, #38233, #19105, #23013, #35579, #22214, #31674, #31880, #3490 ),
 .UNSPECIFIED., .F., .F.,
 ( 4, 3, 3, 3, 3, 3, 3, 3, 4 ),
 ( 6.468151674593620168E-05, 9.076621574722080685E-05, 0.0001210204262067971669, 0.0001512763324577431315, 0.0001815301820994211592, 0.0002117781465860709496, 0.0002420274594459750450, 0.0002722905548971160054, 0.0002816827545175581917 ),
 .UNSPECIFIED. ) ;
#38782 = CARTESIAN_POINT ( 'NONE',  ( 3.300000000000000711, 0.000000000000000000, 0.000000000000000000 ) ) ;
#38783 = CARTESIAN_POINT ( 'NONE',  ( 23.03325835086280193, 4.443132776864800348, 2.273497529138607476 ) ) ;
#38784 = VECTOR ( 'NONE', #22160, 1000.000000000000000 ) ;
#38785 = VERTEX_POINT ( 'NONE', #33202 ) ;
#38786 = CARTESIAN_POINT ( 'NONE',  ( 35.73088790136473136, -1.303468173786156870, -5.537281536383253489 ) ) ;
#38787 = CARTESIAN_POINT ( 'NONE',  ( 30.58053394437551020, -3.206738070849787015, -4.963780911168087506 ) ) ;
#38788 = CARTESIAN_POINT ( 'NONE',  ( -6.448748702180637338, -26.64985754041175525, 6.800000000000000711 ) ) ;
#38789 = CARTESIAN_POINT ( 'NONE',  ( 5.115234526135282067, -30.33731918955309936, 6.887547729233687299 ) ) ;
#38790 = CARTESIAN_POINT ( 'NONE',  ( 5.195132101224134047, -29.76170719274372090, 6.941203072598468360 ) ) ;
#38791 = CARTESIAN_POINT ( 'NONE',  ( -80.19065981525227471, 31.27226540113725051, -8.800414904976364028 ) ) ;
#38792 = CARTESIAN_POINT ( 'NONE',  ( 2.242723711017451382, -32.92639770848892766, 6.894806418505347700 ) ) ;
#38793 = CARTESIAN_POINT ( 'NONE',  ( 1.755573734986932033, -26.07036524390695220, 6.875671892026062437 ) ) ;
#38794 = CARTESIAN_POINT ( 'NONE',  ( 4.342461014271223441, -31.84348076181812814, 7.785096263473212375 ) ) ;
#38795 = ORIENTED_EDGE ( 'NONE', *, *, #39545, .T. ) ;
#38796 = CARTESIAN_POINT ( 'NONE',  ( 66.71755507405909214, 57.88420400998732163, 3.999756211082241109 ) ) ;
#38798 = EDGE_CURVE ( 'NONE', #32959, #29224, #19125, .T. ) ;
#38797 = CARTESIAN_POINT ( 'NONE',  ( 86.59537683758360060, -0.3992097724244685342, -5.811584838773467432 ) ) ;
#38799 = B_SPLINE_CURVE_WITH_KNOTS ( 'NONE', 3,
 ( #2589, #15111, #28697, #9137, #9332, #32000, #21913, #22125, #18598, #12837, #37735, #31183, #34489, #18810, #3209, #9544, #12633, #25203, #28899, #13650, #10143, #20419, #1507, #904, #23526, #35297, #10355, #25807, #23324, #22733, #20222 ),
 .UNSPECIFIED., .F., .F.,
 ( 4, 3, 3, 3, 3, 3, 3, 3, 3, 3, 4 ),
 ( 8.673617379884035472E-19, 3.077658087705402906E-05, 6.152638666999016878E-05, 9.267501192706322183E-05, 0.0001241882240135154308, 0.0001556618703051673150, 0.0001866161554452174247, 0.0002167966385860936747, 0.0002463805737537735322, 0.0002758761370306494001, 0.0002847094172290008749 ),
 .UNSPECIFIED. ) ;
#38800 = PRODUCT_DEFINITION_SHAPE ( 'NONE', 'NONE',  #40730 ) ;
#38801 = B_SPLINE_SURFACE_WITH_KNOTS ( 'NONE', 5, 3, ( 
 ( #40152, #36459, #21434, #24511, #30493, #4765, #2303, #14615, #30284, #4969, #36661, #8649, #21025, #14825, #17496, #29877, #26798, #27391 ),
 ( #5576, #14422, #21226, #5173, #39335, #1902, #36867, #33401, #30707, #24303, #26991, #33797, #20804, #2514, #17705, #11126, #2099, #432 ),
 ( #3533, #37267, #5783, #24718, #30912, #9062, #28004, #12359, #28201, #12972, #15656, #33, #37465, #9884, #15858, #28629, #37873, #22050 ),
 ( #9463, #34420, #6192, #15445, #27796, #3138, #9678, #28415, #6606, #21638, #40348, #18321, #34219, #21842, #5989, #34830, #25540, #18526 ),
 ( #12760, #25339, #15240, #6400, #38082, #31111, #19153, #31516, #12145, #25131, #18738, #18952, #34627, #31719, #37663, #2923, #12560, #34010 ),
 ( #31316, #3339, #2720, #40546, #222, #24931, #9262, #16058, #22263, #6803, #16258, #19758, #13368, #25739, #35822, #1042, #638, #19355 ),
 ( #16646, #32337, #35027, #10077, #13575, #38682, #39078, #4131, #26542, #22460, #13177, #31928, #22661, #38280, #32143, #10280, #4332, #19951 ),
 ( #3735, #7000, #22857, #28831, #7599, #20152, #29232, #26148, #17049, #13973, #35228, #19565, #32531, #13783, #7398, #3940, #38883, #16852 ) ),
 .UNSPECIFIED., .F., .F., .F.,
 ( 6, 2, 6 ),
 ( 4, 1, 1, 1, 1, 1, 1, 1, 1, 1, 1, 1, 1, 1, 1, 4 ),
 ( 0.000000000000000000, 0.5000000000000000000, 1.000000000000000000 ),
 ( 0.006359509864058362355, 0.008899940506546142119, 0.01165379832700513818, 0.01387926207582779702, 0.01684654707425800937, 0.01907201082308066648, 0.02092656394709954681, 0.02241020644631465386, 0.02352293832072598415, 0.02445021488273542778, 0.02519203613234298131, 0.02574840206954863778, 0.02630476800675430812, 0.02686113394395997153, 0.02741749988116563841, 0.02797386581837130182 ),
 .UNSPECIFIED. ) ;
#38802 = VERTEX_POINT ( 'NONE', #6775 ) ;
#38803 = CARTESIAN_POINT ( 'NONE',  ( 2.866511140812421754, -26.26990339287398868, 7.720710062488891801 ) ) ;
#38804 = LINE ( 'NONE', #6919, #10047 ) ;
#38805 = EDGE_CURVE ( 'NONE', #7875, #19840, #22632, .T. ) ;
#38806 = DIRECTION ( 'NONE',  ( 0.000000000000000000, 0.000000000000000000, -1.000000000000000000 ) ) ;
#38807 = VERTEX_POINT ( 'NONE', #3916 ) ;
#38808 = DIRECTION ( 'NONE',  ( 1.000000000000000000, 0.000000000000000000, 0.000000000000000000 ) ) ;
#38809 = VECTOR ( 'NONE', #32344, 1000.000000000000000 ) ;
#38810 = ORIENTED_EDGE ( 'NONE', *, *, #10784, .T. ) ;
#38811 = CARTESIAN_POINT ( 'NONE',  ( 79.12445352002978893, 64.93440905817641351, -3.301258712451523358 ) ) ;
#38812 = CARTESIAN_POINT ( 'NONE',  ( 33.89602703800589012, -5.455856628420105103, 0.7063779492982765751 ) ) ;
#38813 = EDGE_CURVE ( 'NONE', #1662, #4028, #26120, .T. ) ;
#38814 = CARTESIAN_POINT ( 'NONE',  ( 78.60455099833413328, 65.79598288722411326, 2.095806625473878970 ) ) ;
#38816 = ORIENTED_EDGE ( 'NONE', *, *, #16777, .F. ) ;
#38815 = CARTESIAN_POINT ( 'NONE',  ( -1.318642678379643218, -31.13375132202764561, 6.871394612369934762 ) ) ;
#38817 = CARTESIAN_POINT ( 'NONE',  ( 25.33339624544385416, 2.111467966597739832, 4.160287193241738457 ) ) ;
#38818 = CARTESIAN_POINT ( 'NONE',  ( 0.9128126353795650294, -32.98017209969670205, 6.993830769476427456 ) ) ;
#38819 = FACE_OUTER_BOUND ( 'NONE', #35257, .T. ) ;
#38820 = CARTESIAN_POINT ( 'NONE',  ( 21.85643539959773207, -10.94848525941816675, -12.02078412262589602 ) ) ;
#38821 = CARTESIAN_POINT ( 'NONE',  ( 3.461027628862304084, -26.66127814943644125, 7.784476445165070757 ) ) ;
#38822 = CARTESIAN_POINT ( 'NONE',  ( 2.495473842921097418, -33.76723158512031375, 7.695279973900954751 ) ) ;
#38823 = AXIS2_PLACEMENT_3D ( 'NONE', #35036, #18746, #24939 ) ;
#38824 = CARTESIAN_POINT ( 'NONE',  ( 0.000000000000000000, 13.37661300689600097, 6.000000000000000000 ) ) ;
#38825 = CARTESIAN_POINT ( 'NONE',  ( -71.87765774115447925, 0.8657319589700837037, -9.955254003897318071 ) ) ;
#38826 = CARTESIAN_POINT ( 'NONE',  ( -1.614537886288068158, -25.59834652758622653, 7.635761828346577573 ) ) ;
#38827 = CARTESIAN_POINT ( 'NONE',  ( 5.200346647029098435, -29.55249110255828882, 7.749999999999999112 ) ) ;
#38828 = CARTESIAN_POINT ( 'NONE',  ( 79.73516162904326166, 65.38506083608318420, 3.083955809406667914 ) ) ;
#38829 = CARTESIAN_POINT ( 'NONE',  ( -2.527465627618633803, -28.94812858826901802, 7.754798119455333705 ) ) ;
#38830 = CARTESIAN_POINT ( 'NONE',  ( 3.894409106313954538, -26.97255664000370246, 7.775108481317160702 ) ) ;
#38831 = CARTESIAN_POINT ( 'NONE',  ( -1.339380734913657500, -27.83505459351727396, 7.750000000000002665 ) ) ;
#38832 = CYLINDRICAL_SURFACE ( 'NONE', #39669, 0.09010775117052974292 ) ;
#38833 = ADVANCED_FACE ( 'NONE', ( #19325 ), #19531, .F. ) ;
#38834 = CARTESIAN_POINT ( 'NONE',  ( 4.491609779761556176, -27.45826272268804047, 6.903112506833895878 ) ) ;
#38835 = AXIS2_PLACEMENT_3D ( 'NONE', #19407, #6040, #37319 ) ;
#38836 = FACE_OUTER_BOUND ( 'NONE', #39667, .T. ) ;
#38837 = CARTESIAN_POINT ( 'NONE',  ( -22.97867591359219119, -26.64985754041175525, 6.700000000000000178 ) ) ;
#38838 = DIRECTION ( 'NONE',  ( -0.000000000000000000, -0.000000000000000000, -1.000000000000000000 ) ) ;
#38839 = CARTESIAN_POINT ( 'NONE',  ( 2.910139986571841586, -32.85421171754464353, 7.635761828346577573 ) ) ;
#38840 = CARTESIAN_POINT ( 'NONE',  ( 68.58273017919226788, 58.67848115723035107, 3.992679187475148161 ) ) ;
#38841 = CARTESIAN_POINT ( 'NONE',  ( 36.44708399685710987, -2.354165099489201385, 5.894846952403873352 ) ) ;
#38842 = EDGE_CURVE ( 'NONE', #2595, #20836, #13338, .T. ) ;
#38843 = LINE ( 'NONE', #4490, #40437 ) ;
#38845 = EDGE_CURVE ( 'NONE', #9487, #19232, #18920, .T. ) ;
#38844 = CARTESIAN_POINT ( 'NONE',  ( 85.23697547898807159, 2.562304445728192714, -3.499295437968926947 ) ) ;
#38847 = CARTESIAN_POINT ( 'NONE',  ( -0.5201900046161557212, -26.86455205392092083, 6.887161170156907986 ) ) ;
#38846 = CARTESIAN_POINT ( 'NONE',  ( 80.92403995952693663, 62.73960429493251212, -3.332694751021839430 ) ) ;
#38848 = CARTESIAN_POINT ( 'NONE',  ( -1.282377406787723384, -27.73875492391482211, 6.863805608295729499 ) ) ;
#38849 = CARTESIAN_POINT ( 'NONE',  ( 2.390042335280297969, -26.14898894374510974, 7.780491323090172884 ) ) ;
#38850 = ORIENTED_EDGE ( 'NONE', *, *, #40273, .T. ) ;
#38851 = VECTOR ( 'NONE', #34668, 1000.000000000000000 ) ;
#38852 = CARTESIAN_POINT ( 'NONE',  ( -76.67582790101022283, 10.73401294744294532, -8.185679464797956939 ) ) ;
#38853 = CARTESIAN_POINT ( 'NONE',  ( -0.7996099067669091287, -29.56993018339339940, 6.000000000000000000 ) ) ;
#38854 = EDGE_CURVE ( 'NONE', #2584, #26610, #26516, .T. ) ;
#38855 = ORIENTED_EDGE ( 'NONE', *, *, #7945, .F. ) ;
#38856 = CARTESIAN_POINT ( 'NONE',  ( 21.85643539959777115, -33.54387950140291963, -2.500000000000000000 ) ) ;
#38857 = EDGE_CURVE ( 'NONE', #26935, #10351, #26716, .T. ) ;
#38858 = ORIENTED_EDGE ( 'NONE', *, *, #36524, .T. ) ;
#38859 = CARTESIAN_POINT ( 'NONE',  ( 80.52560336917625250, 62.91486207252160057, -3.518158556798104630 ) ) ;
#38860 = CARTESIAN_POINT ( 'NONE',  ( -27.07867591359219972, -26.64985754041175525, 6.700000000000000178 ) ) ;
#38861 = CARTESIAN_POINT ( 'NONE',  ( 81.04163241827637876, 61.94641952267326701, 2.758686562281579047 ) ) ;
#38862 = CARTESIAN_POINT ( 'NONE',  ( 23.62965689264861879, 0.6308181322251997791, 5.426430504554879519 ) ) ;
#38863 = EDGE_LOOP ( 'NONE', ( #37443, #34003, #26969, #23164 ) ) ;
#38864 = VECTOR ( 'NONE', #9228, 1000.000000000000000 ) ;
#38865 = CARTESIAN_POINT ( 'NONE',  ( -8.400069747914319152, -0.9236158798217076749, -2.500000000000000000 ) ) ;
#38867 = LINE ( 'NONE', #7780, #33495 ) ;
#38866 = CARTESIAN_POINT ( 'NONE',  ( -58.17330720045938364, 29.79550679426005644, -4.662693745304140158 ) ) ;
#38868 = CARTESIAN_POINT ( 'NONE',  ( -70.92837670882107659, -65.19654454972992141, 6.000000000000002665 ) ) ;
#38869 = CARTESIAN_POINT ( 'NONE',  ( -26.87867591359219333, -24.55319635012989110, 6.700000000000000178 ) ) ;
#38870 = ORIENTED_EDGE ( 'NONE', *, *, #29796, .T. ) ;
#38871 = CARTESIAN_POINT ( 'NONE',  ( 22.08468009823165801, 5.143601559783003374, -3.328927790978220891 ) ) ;
#38872 = ORIENTED_EDGE ( 'NONE', *, *, #3127, .T. ) ;
#38873 = DIRECTION ( 'NONE',  ( 1.000000000000000000, 0.000000000000000000, 0.000000000000000000 ) ) ;
#38874 = CARTESIAN_POINT ( 'NONE',  ( 21.85643539959779957, 2.883972393613821072, 11.80804406839454046 ) ) ;
#38875 = CARTESIAN_POINT ( 'NONE',  ( 21.69289330442630259, 6.888012688853828891, 2.083760414285012352 ) ) ;
#38876 = CARTESIAN_POINT ( 'NONE',  ( 17.47038192185404171, 11.99840028321635010, 2.499999999999993339 ) ) ;
#38877 = CARTESIAN_POINT ( 'NONE',  ( -14.87867591359218977, -26.64985754041175525, 6.800000000000000711 ) ) ;
#38878 = CARTESIAN_POINT ( 'NONE',  ( 81.64185025297332743, 61.96196063151020184, 2.170472567306916734 ) ) ;
#38879 = B_SPLINE_CURVE_WITH_KNOTS ( 'NONE', 3,
 ( #9572, #25030, #15339, #34114, #18621, #37165, #25432, #34516, #37975, #5676 ),
 .UNSPECIFIED., .F., .F.,
 ( 4, 3, 3, 4 ),
 ( 0.0001585009270395705192, 0.0001815657551981863355, 0.0002118214035944168423, 0.0002170292169044748620 ),
 .UNSPECIFIED. ) ;
#38880 = CARTESIAN_POINT ( 'NONE',  ( 86.11108918975101290, 0.7237488529220831301, -5.972109037703948076 ) ) ;
#38881 = CARTESIAN_POINT ( 'NONE',  ( -1.489952004402606667, -30.76578679454389587, 7.257242401810563237 ) ) ;
#38882 = EDGE_LOOP ( 'NONE', ( #7188, #3115, #18706, #24923, #34808 ) ) ;
#38883 = CARTESIAN_POINT ( 'NONE',  ( 14.75302088585650573, -5.978111498305209714, 2.508963731033090117 ) ) ;
#38884 = CARTESIAN_POINT ( 'NONE',  ( 31.00341140003851947, -3.765336078302973899, 4.602883256886119767 ) ) ;
#38885 = CARTESIAN_POINT ( 'NONE',  ( 26.27873381384168994, -2.762334174294334144, -4.307829983865710588 ) ) ;
#38886 = CARTESIAN_POINT ( 'NONE',  ( 36.89680064675319926, -3.001266127369541792, -5.965036112058319517 ) ) ;
#38887 = CARTESIAN_POINT ( 'NONE',  ( 5.155307176249795731, -29.05665538096915412, 7.776484688137381696 ) ) ;
#38888 = DIRECTION ( 'NONE',  ( 0.000000000000000000, 0.000000000000000000, 1.000000000000000000 ) ) ;
#38889 = DIRECTION ( 'NONE',  ( 0.000000000000000000, 0.000000000000000000, -1.000000000000000000 ) ) ;
#38890 = VERTEX_POINT ( 'NONE', #38856 ) ;
#38891 = CARTESIAN_POINT ( 'NONE',  ( 3.866188828012731893, -26.94898948837244035, 7.652160403243380316 ) ) ;
#38892 = CARTESIAN_POINT ( 'NONE',  ( 3.431406277207060818, -32.49629020484249509, 7.692469944509197077 ) ) ;
#38893 = AXIS2_PLACEMENT_3D ( 'NONE', #32319, #35807, #16631 ) ;
#38894 = CARTESIAN_POINT ( 'NONE',  ( 32.98767453130994909, -3.051313967188787668, -5.354922439171034831 ) ) ;
#38895 = ORIENTED_EDGE ( 'NONE', *, *, #3378, .F. ) ;
#38896 = VERTEX_POINT ( 'NONE', #10648 ) ;
#38897 = CARTESIAN_POINT ( 'NONE',  ( 36.87099407197327139, -2.087246581719376604, 5.864208482129122046 ) ) ;
#38898 = LINE ( 'NONE', #26365, #40253 ) ;
#38899 = CARTESIAN_POINT ( 'NONE',  ( 66.27376694609004915, 57.73522568913436004, -4.000000000000000000 ) ) ;
#38900 = CARTESIAN_POINT ( 'NONE',  ( 86.32543542292076211, -0.3344508995418832842, 5.872725293628850096 ) ) ;
#38901 = ADVANCED_FACE ( 'NONE', ( #36184 ), #29795, .F. ) ;
#38902 = VERTEX_POINT ( 'NONE', #7964 ) ;
#38903 = EDGE_CURVE ( 'NONE', #35504, #25345, #17222, .T. ) ;
#38904 = CARTESIAN_POINT ( 'NONE',  ( -1.432293644835494373, -27.47664038617742577, -1.000000000000000000 ) ) ;
#38905 = VERTEX_POINT ( 'NONE', #13947 ) ;
#38906 = CARTESIAN_POINT ( 'NONE',  ( -57.31959649706902127, 29.49889766843898187, -4.251262061546396076 ) ) ;
#38907 = LINE ( 'NONE', #14592, #30449 ) ;
#38908 = ORIENTED_EDGE ( 'NONE', *, *, #34628, .T. ) ;
#38909 = CARTESIAN_POINT ( 'NONE',  ( 21.80921096923039215, 5.240870915421466769, 3.636790624354177215 ) ) ;
#38910 = CARTESIAN_POINT ( 'NONE',  ( 78.98267122246090821, 66.20432814577485203, -1.134074597586744115 ) ) ;
#38911 = LINE ( 'NONE', #1074, #12071 ) ;
#38912 = ORIENTED_EDGE ( 'NONE', *, *, #35537, .F. ) ;
#38914 = CARTESIAN_POINT ( 'NONE',  ( -8.400069747914319152, -0.9236158798217076749, 2.500000000000000000 ) ) ;
#38913 = CARTESIAN_POINT ( 'NONE',  ( 2.487967551086643692, -26.15968826709010031, 6.993830769476427456 ) ) ;
#38915 = CARTESIAN_POINT ( 'NONE',  ( -70.92837670882107659, -65.19654454972992141, 0.000000000000000000 ) ) ;
#38916 = CARTESIAN_POINT ( 'NONE',  ( 75.43741953989470517, 63.08613174173238747, 3.462570962765048055 ) ) ;
#38917 = CARTESIAN_POINT ( 'NONE',  ( 21.85265456426768083, 2.967629154170456474, -5.140454503935664832 ) ) ;
#38918 = ORIENTED_EDGE ( 'NONE', *, *, #11255, .F. ) ;
#38919 = DIRECTION ( 'NONE',  ( -0.000000000000000000, 0.000000000000000000, -1.000000000000000000 ) ) ;
#38920 = LINE ( 'NONE', #6644, #36570 ) ;
#38921 = CARTESIAN_POINT ( 'NONE',  ( 24.21109618614866932, 2.662543315632417862, -3.985125126059221312 ) ) ;
#38922 = CARTESIAN_POINT ( 'NONE',  ( -0.4954141421830357550, -26.97407892422453202, 7.635761828346577573 ) ) ;
#38923 = DIRECTION ( 'NONE',  ( -0.000000000000000000, -0.000000000000000000, 1.000000000000000000 ) ) ;
#38924 = CARTESIAN_POINT ( 'NONE',  ( 79.21008177357740010, 66.23692415242767595, 1.465632304122485685 ) ) ;
#38925 = CARTESIAN_POINT ( 'NONE',  ( -0.2136480384828472467, -32.50019606712385212, 6.961115707816242448 ) ) ;
#38926 = CARTESIAN_POINT ( 'NONE',  ( 27.86875652909539980, 2.635651561731235493, 0.006556038081918813022 ) ) ;
#38927 = CARTESIAN_POINT ( 'NONE',  ( 4.372846383550529126, -27.30984669459420289, 7.635761828346578461 ) ) ;
#38928 = CARTESIAN_POINT ( 'NONE',  ( 11.65737507970504616, -38.28842912540938670, 6.800000000000000711 ) ) ;
#38929 = AXIS2_PLACEMENT_3D ( 'NONE', #37230, #40510, #9025 ) ;
#38930 = CARTESIAN_POINT ( 'NONE',  ( 6.112940767310136359, -27.90626689514689218, 7.695279973900954751 ) ) ;
#38931 = CARTESIAN_POINT ( 'NONE',  ( 4.932354078450567059, -25.52873147056503811, 7.754798119455333705 ) ) ;
#38932 = CARTESIAN_POINT ( 'NONE',  ( 34.95695827223672580, -1.636488140955191017, -5.662276794249945233 ) ) ;
#38933 = CARTESIAN_POINT ( 'NONE',  ( -42.34874870218063592, -26.64985754041175525, 6.700000000000000178 ) ) ;
#38934 = DIRECTION ( 'NONE',  ( -0.1736481776669240584, -0.9848077530122092416, 0.000000000000000000 ) ) ;
#38935 =( BOUNDED_CURVE ( )  B_SPLINE_CURVE ( 3, ( #17315, #7464, #20021, #19631 ),
 .UNSPECIFIED., .F., .T. ) 
 B_SPLINE_CURVE_WITH_KNOTS ( ( 4, 4 ),
 ( 1.347909859412853351, 1.534781240595298302 ),
 .UNSPECIFIED. ) 
 CURVE ( )  GEOMETRIC_REPRESENTATION_ITEM ( )  RATIONAL_B_SPLINE_CURVE ( ( 1.000000000000000000, 0.9970920404276226723, 0.9970920404276226723, 1.000000000000000000 ) ) 
 REPRESENTATION_ITEM ( '' )  );
#38936 = LINE ( 'NONE', #1300, #32567 ) ;
#38937 = CARTESIAN_POINT ( 'NONE',  ( -1.546934178659356451, -28.27117655838526389, 7.766640943994350010 ) ) ;
#38938 = CARTESIAN_POINT ( 'NONE',  ( -0.4574210171174859507, -32.19744825413003753, 7.695279973900954751 ) ) ;
#38939 = EDGE_LOOP ( 'NONE', ( #25129, #18877, #25550, #27201, #8193, #37298, #36436 ) ) ;
#38940 = CARTESIAN_POINT ( 'NONE',  ( 36.78034191296258371, -2.229234730061248282, 5.922124464258623711 ) ) ;
#38941 = CARTESIAN_POINT ( 'NONE',  ( -70.59363788503038961, 0.1660198011701667642, 6.003704795174114039 ) ) ;
#38942 = CARTESIAN_POINT ( 'NONE',  ( 67.64019463258649978, 58.53452770292938112, -3.982857479566666914 ) ) ;
#38943 = CARTESIAN_POINT ( 'NONE',  ( 4.713943603702952068, -27.78990194465062302, 7.678495282201405203 ) ) ;
#38944 = ORIENTED_EDGE ( 'NONE', *, *, #20897, .T. ) ;
#38945 = CARTESIAN_POINT ( 'NONE',  ( -0.9720661970843325062, -31.83001367219261013, 7.635761828346575797 ) ) ;
#38947 = EDGE_CURVE ( 'NONE', #31847, #38807, #30423, .T. ) ;
#38946 = CARTESIAN_POINT ( 'NONE',  ( 3.823592214863587913, -32.22550894298759516, 7.782034975670475418 ) ) ;
#38948 = CARTESIAN_POINT ( 'NONE',  ( 85.70685082919769116, 0.7924140212991883647, -5.893544677374721097 ) ) ;
#38949 = CARTESIAN_POINT ( 'NONE',  ( 2.326074584482883179, -32.91186359347347690, 7.691066658568947112 ) ) ;
#38950 = CARTESIAN_POINT ( 'NONE',  ( 3.598121943223039576, -26.62907708263870887, 7.009310105710485850 ) ) ;
#38951 = VECTOR ( 'NONE', #31336, 1000.000000000000000 ) ;
#38952 = CARTESIAN_POINT ( 'NONE',  ( 4.403765497540709895, -31.79293866618682785, 7.678495282201404315 ) ) ;
#38953 = EDGE_LOOP ( 'NONE', ( #31285, #4924, #29847, #11471 ) ) ;
#38954 = SURFACE_SIDE_STYLE ('',( #1513 ) ) ;
#38955 = CARTESIAN_POINT ( 'NONE',  ( 79.24015747652954644, 65.65980919716056974, 2.710038060602471877 ) ) ;
#38956 = CARTESIAN_POINT ( 'NONE',  ( 30.10909256169910364, -6.281120516155699995, -2.500000000000003997 ) ) ;
#38957 = ORIENTED_EDGE ( 'NONE', *, *, #8404, .T. ) ;
#38958 = CARTESIAN_POINT ( 'NONE',  ( 78.65659160455585663, 63.63274296288032161, -3.750642650174855319 ) ) ;
#38960 = CARTESIAN_POINT ( 'NONE',  ( -0.9352292415849461360, -31.71783863626873767, 6.894806418505345924 ) ) ;
#38959 = CARTESIAN_POINT ( 'NONE',  ( 26.74545741276980237, 0.9075178902881906318, 4.382577745642065814 ) ) ;
#38961 = CARTESIAN_POINT ( 'NONE',  ( 81.60109106392830824, 62.17032169346391157, -2.476693319882541378 ) ) ;
#38962 = CARTESIAN_POINT ( 'NONE',  ( 78.19628368166274868, 65.45398019160434444, 2.372109611208335078 ) ) ;
#38963 = DIRECTION ( 'NONE',  ( -0.8660254037844415942, 0.4999999999999950040, -0.000000000000000000 ) ) ;
#38964 = CARTESIAN_POINT ( 'NONE',  ( 82.59411735159427792, 63.56171878218358273, 1.145133701562419226 ) ) ;
#38965 = LINE ( 'NONE', #10764, #38032 ) ;
#38966 = CARTESIAN_POINT ( 'NONE',  ( 26.66483005201559564, 2.460286195115170216, -3.284910328407702806 ) ) ;
#38967 = ADVANCED_FACE ( 'NONE', ( #35790 ), #7568, .F. ) ;
#38968 = CARTESIAN_POINT ( 'NONE',  ( -64.35089310738592872, 36.57692748660996074, -5.628006413927908014 ) ) ;
#38969 = EDGE_LOOP ( 'NONE', ( #24119, #31138, #13086, #11707 ) ) ;
#38970 = CARTESIAN_POINT ( 'NONE',  ( -77.59921745286224848, -4.978234906976595653, 7.463450837162017848 ) ) ;
#38971 = CARTESIAN_POINT ( 'NONE',  ( 21.73405303197773009, 0.2198190191631417822, -9.095604756692427628 ) ) ;
#38972 = LINE ( 'NONE', #10771, #16266 ) ;
#38973 = LINE ( 'NONE', #32635, #19042 ) ;
#38974 = ORIENTED_EDGE ( 'NONE', *, *, #22628, .T. ) ;
#38975 = CARTESIAN_POINT ( 'NONE',  ( 33.11285781741161571, -0.1526090149532899065, -4.944069884480080113 ) ) ;
#38976 = CARTESIAN_POINT ( 'NONE',  ( 30.19238557334687911, -2.952639005720375742, -4.918649992961978690 ) ) ;
#38977 = CARTESIAN_POINT ( 'NONE',  ( 3.315058325667250116, -32.67523709003925347, 6.880828092187092793 ) ) ;
#38978 = CARTESIAN_POINT ( 'NONE',  ( -1.088725521452697409, -31.68436562166070658, 7.009310105710489402 ) ) ;
#38979 = DIRECTION ( 'NONE',  ( -0.000000000000000000, -0.000000000000000000, 1.000000000000000000 ) ) ;
#38980 = CARTESIAN_POINT ( 'NONE',  ( 2.812523938828905834, -32.78289859174327603, 6.889465824494257262 ) ) ;
#38981 = DIRECTION ( 'NONE',  ( 0.000000000000000000, 0.000000000000000000, 1.000000000000000000 ) ) ;
#38982 = AXIS2_PLACEMENT_3D ( 'NONE', #38104, #32359, #35051 ) ;
#38983 = ADVANCED_FACE ( 'NONE', ( #17415 ), #24380, .T. ) ;
#38984 = CARTESIAN_POINT ( 'NONE',  ( 1.871557904069252487, -26.07411760613849694, 7.011627023500182965 ) ) ;
#38985 = ORIENTED_EDGE ( 'NONE', *, *, #21544, .F. ) ;
#38986 = ORIENTED_EDGE ( 'NONE', *, *, #15363, .F. ) ;
#38987 = CARTESIAN_POINT ( 'NONE',  ( 66.42297474478721142, 57.78816748095999145, 4.000000000000013323 ) ) ;
#38988 = CARTESIAN_POINT ( 'NONE',  ( 72.70998213798715426, 61.65396340192921087, -3.619654763610430592 ) ) ;
#38989 = CARTESIAN_POINT ( 'NONE',  ( -64.08758708074093136, 38.76906266698302517, 2.999999999999999112 ) ) ;
#38990 = AXIS2_PLACEMENT_3D ( 'NONE', #24334, #36897, #33829 ) ;
#38991 = CARTESIAN_POINT ( 'NONE',  ( 88.11323260317807637, -2.391772166421624490, 1.226420884133070599 ) ) ;
#38992 = EDGE_CURVE ( 'NONE', #34807, #12332, #30834, .T. ) ;
#38993 = CARTESIAN_POINT ( 'NONE',  ( -81.15948786935145165, 10.50821952958543903, -3.991233431468591331 ) ) ;
#38994 = DIRECTION ( 'NONE',  ( 1.000000000000000000, 0.000000000000000000, 0.000000000000000000 ) ) ;
#38995 = CARTESIAN_POINT ( 'NONE',  ( 2.324907734538560256, -32.91208277201279486, 7.712764235869103757 ) ) ;
#38996 = FACE_OUTER_BOUND ( 'NONE', #36945, .T. ) ;
#38997 = CARTESIAN_POINT ( 'NONE',  ( 2.645388388363652865, -26.19285331904208647, 7.501983001166817822 ) ) ;
#38998 = VECTOR ( 'NONE', #9197, 1000.000000000000000 ) ;
#38999 = VERTEX_POINT ( 'NONE', #2643 ) ;
#39000 = ORIENTED_EDGE ( 'NONE', *, *, #21764, .T. ) ;
#39001 = CARTESIAN_POINT ( 'NONE',  ( 78.79414303495656213, 65.54496243570987701, -2.640205493567942874 ) ) ;
#39002 = CARTESIAN_POINT ( 'NONE',  ( 37.20094714327657215, -2.700959843830776919, 5.995701502916164216 ) ) ;
#39003 = CARTESIAN_POINT ( 'NONE',  ( 79.45016587565709187, 64.47252957033400378, 3.557377001560511509 ) ) ;
#39004 = CARTESIAN_POINT ( 'NONE',  ( 0.5751845763345247997, -26.36150267606116060, 7.784838882742139532 ) ) ;
#39005 = ADVANCED_FACE ( 'NONE', ( #40467 ), #33930, .T. ) ;
#39006 = PLANE ( 'NONE',  #40301 ) ;
#39007 = CARTESIAN_POINT ( 'NONE',  ( 3.558396595903837056, -26.60381962644626697, 7.750000000000000888 ) ) ;
#39008 = DIRECTION ( 'NONE',  ( -0.000000000000000000, -0.000000000000000000, 1.000000000000000000 ) ) ;
#39009 = CARTESIAN_POINT ( 'NONE',  ( 21.85643539959777470, 7.942361823516107755, 9.319573164223585948 ) ) ;
#39010 = ORIENTED_EDGE ( 'NONE', *, *, #16965, .F. ) ;
#39011 = CARTESIAN_POINT ( 'NONE',  ( 75.43605262791740529, 63.77904386412239290, -2.884284812001602027 ) ) ;
#39012 = VECTOR ( 'NONE', #25000, 1000.000000000000000 ) ;
#39013 = VECTOR ( 'NONE', #36102, 1000.000000000000000 ) ;
#39014 = CARTESIAN_POINT ( 'NONE',  ( -72.84104406220187400, 2.224784376281895071, -10.96219629948401675 ) ) ;
#39015 = CARTESIAN_POINT ( 'NONE',  ( -0.03065438358791858567, -26.64358689880297248, 7.693875151218752428 ) ) ;
#39016 = CARTESIAN_POINT ( 'NONE',  ( -53.21549048184568420, -38.28842912540938670, 6.000000000000000000 ) ) ;
#39017 = CARTESIAN_POINT ( 'NONE',  ( 80.45774067191288736, 64.33927723362793927, 3.562450064734662636 ) ) ;
#39018 = CARTESIAN_POINT ( 'NONE',  ( -1.511438080339128076, -30.68539464244183179, 7.785868773668302545 ) ) ;
#39019 = B_SPLINE_CURVE_WITH_KNOTS ( 'NONE', 3,
 ( #38146, #20022, #31789, #6872, #22331, #10353, #4195, #29303, #19224, #38545 ),
 .UNSPECIFIED., .F., .F.,
 ( 4, 3, 3, 4 ),
 ( 0.0001585009270395740699, 0.0001815657551981801556, 0.0002118214035944104455, 0.0002170292169044772744 ),
 .UNSPECIFIED. ) ;
#39020 = DIRECTION ( 'NONE',  ( -0.2312332387574689563, -0.9728983447892853853, -0.000000000000000000 ) ) ;
#39021 = FACE_OUTER_BOUND ( 'NONE', #39092, .T. ) ;
#39022 = CARTESIAN_POINT ( 'NONE',  ( 3.927859974615581340, -26.87023058389461738, 7.730015791551953619 ) ) ;
#39023 = CARTESIAN_POINT ( 'NONE',  ( 35.89208955089092967, -2.095693868708802921, 5.808226646519337955 ) ) ;
#39024 = EDGE_CURVE ( 'NONE', #6453, #19329, #31236, .T. ) ;
#39025 = ADVANCED_FACE ( 'NONE', ( #30630 ), #34142, .F. ) ;
#39026 = ADVANCED_FACE ( 'NONE', ( #5910 ), #15577, .F. ) ;
#39027 = AXIS2_PLACEMENT_3D ( 'NONE', #27717, #24429, #30197 ) ;
#39028 = CARTESIAN_POINT ( 'NONE',  ( 4.496857463589675419, -27.46522619576845869, 6.989977667959448304 ) ) ;
#39029 = CARTESIAN_POINT ( 'NONE',  ( -30.44874870218064089, -25.49307895267003587, 6.700000000000000178 ) ) ;
#39030 = CARTESIAN_POINT ( 'NONE',  ( 5.055212331642637835, -30.59122463574226103, 7.139344958878412584 ) ) ;
#39031 = CARTESIAN_POINT ( 'NONE',  ( 4.236974709687405749, -31.83396407781120274, 6.864651958020303368 ) ) ;
#39032 = AXIS2_PLACEMENT_3D ( 'NONE', #38510, #30477, #39520 ) ;
#39033 = CARTESIAN_POINT ( 'NONE',  ( 68.50220056233268906, 58.89075781393282227, 3.976359261632469444 ) ) ;
#39034 = CARTESIAN_POINT ( 'NONE',  ( 36.79789676325057712, -2.555714875043423095, 5.949599769038292685 ) ) ;
#39035 = VERTEX_POINT ( 'NONE', #28131 ) ;
#39036 = LINE ( 'NONE', #29782, #39145 ) ;
#39037 = CARTESIAN_POINT ( 'NONE',  ( 85.38594790374143884, 2.393190016811436394, 3.957880923259903927 ) ) ;
#39039 = CARTESIAN_POINT ( 'NONE',  ( 1.530267914844154253, -26.16714112483892762, 7.139196562012272373 ) ) ;
#39038 = CARTESIAN_POINT ( 'NONE',  ( 79.10769140560613266, 65.82222301601623826, -2.432199249741003211 ) ) ;
#39040 = CARTESIAN_POINT ( 'NONE',  ( 11.29080664838498649, 1.564594260697056104E-15, 6.000000000000000000 ) ) ;
#39041 = CARTESIAN_POINT ( 'NONE',  ( 2.372232459882097189, -26.14921434934317901, 7.784725160561909441 ) ) ;
#39042 = VERTEX_POINT ( 'NONE', #27311 ) ;
#39043 = CARTESIAN_POINT ( 'NONE',  ( -80.90861860399088812, 11.45717611192839591, 0.6283086135788885640 ) ) ;
#39044 = CARTESIAN_POINT ( 'NONE',  ( 24.80856304665041634, -5.882444228827781174, -2.847423770020717892 ) ) ;
#39045 = ORIENTED_EDGE ( 'NONE', *, *, #24551, .F. ) ;
#39046 = VECTOR ( 'NONE', #18137, 1000.000000000000000 ) ;
#39047 = AXIS2_PLACEMENT_3D ( 'NONE', #9659, #25719, #18931 ) ;
#39048 = CIRCLE ( 'NONE', #4881, 0.1000000000000028644 ) ;
#39049 = ORIENTED_EDGE ( 'NONE', *, *, #10460, .F. ) ;
#39050 = CARTESIAN_POINT ( 'NONE',  ( 79.86701161339750854, 64.38869582053065699, -3.619557188109182810 ) ) ;
#39051 = DIRECTION ( 'NONE',  ( 0.000000000000000000, 0.000000000000000000, 1.000000000000000000 ) ) ;
#39052 = CARTESIAN_POINT ( 'NONE',  ( 80.35739993109717716, 63.53218113005920742, 3.674973878998263555 ) ) ;
#39053 = CARTESIAN_POINT ( 'NONE',  ( 22.80473035351651134, 0.6264772378953792353, 6.107320914785919541 ) ) ;
#39054 = VERTEX_POINT ( 'NONE', #39872 ) ;
#39055 = LINE ( 'NONE', #20131, #36685 ) ;
#39056 = VECTOR ( 'NONE', #27195, 1000.000000000000114 ) ;
#39057 = MANIFOLD_SOLID_BREP ( 'Cut-Extrude12', #13048 ) ;
#39058 = CARTESIAN_POINT ( 'NONE',  ( 5.049922047023196470, -28.94623841263004138, 7.257242401810563237 ) ) ;
#39060 = CARTESIAN_POINT ( 'NONE',  ( 16.64247417493278292, 12.36459659649736409, 2.500000000000000888 ) ) ;
#39059 = CARTESIAN_POINT ( 'NONE',  ( 0.000000000000000000, 0.000000000000000000, 0.000000000000000000 ) ) ;
#39061 = LINE ( 'NONE', #38459, #6062 ) ;
#39062 = CARTESIAN_POINT ( 'NONE',  ( 3.926249267005272436, -32.27095793936597090, 6.894806418505347700 ) ) ;
#39063 = CARTESIAN_POINT ( 'NONE',  ( 24.29495741014220300, 3.123657746401501623, -3.464203466336227333 ) ) ;
#39064 = VERTEX_POINT ( 'NONE', #759 ) ;
#39065 = CARTESIAN_POINT ( 'NONE',  ( -70.92837670882012446, 0.2170085631207802901, 6.000000000001379341 ) ) ;
#39066 = ADVANCED_FACE ( 'NONE', ( #25057 ), #32060, .T. ) ;
#39067 = CARTESIAN_POINT ( 'NONE',  ( 22.43090457150155004, 1.240285785788341810, -8.908344141805525140 ) ) ;
#39068 = EDGE_CURVE ( 'NONE', #36841, #19982, #23071, .T. ) ;
#39069 = CARTESIAN_POINT ( 'NONE',  ( 18.14195397311778990, 13.68994309133309173, -3.806916816955884020 ) ) ;
#39070 = CARTESIAN_POINT ( 'NONE',  ( 15.71701927994473813, 8.042377773714102673, 3.484701592660909508 ) ) ;
#39071 = CARTESIAN_POINT ( 'NONE',  ( 0.3574051669894162675, -32.69345966426144656, 7.006423389747790331 ) ) ;
#39072 = CARTESIAN_POINT ( 'NONE',  ( 81.21919753139290776, 63.96565923609905013, 3.341858160559717295 ) ) ;
#39073 = CARTESIAN_POINT ( 'NONE',  ( 87.19696342060086636, -0.1553247823698818142, -5.755373573531420206 ) ) ;
#39074 = FACE_OUTER_BOUND ( 'NONE', #25752, .T. ) ;
#39075 = ORIENTED_EDGE ( 'NONE', *, *, #12083, .T. ) ;
#39076 = CARTESIAN_POINT ( 'NONE',  ( 24.12517570173129400, 0.5279882154166138930, -5.092426393238373983 ) ) ;
#39077 = EDGE_CURVE ( 'NONE', #5343, #1678, #21973, .T. ) ;
#39078 = CARTESIAN_POINT ( 'NONE',  ( 21.52094422564899290, -2.679845695244565729, 3.565261851052226483 ) ) ;
#39079 = AXIS2_PLACEMENT_3D ( 'NONE', #16115, #3396, #31167 ) ;
#39080 = CIRCLE ( 'NONE', #14100, 0.1000000000000028644 ) ;
#39081 = CARTESIAN_POINT ( 'NONE',  ( 5.150390093233091271, -29.56993018339339940, 6.850000000000000533 ) ) ;
#39082 = CARTESIAN_POINT ( 'NONE',  ( 16.01709162683344445, -3.387958631065356663, -2.706252541828943592 ) ) ;
#39083 = CARTESIAN_POINT ( 'NONE',  ( 36.97911392267047148, -2.955988235745242498, -5.977883089519319348 ) ) ;
#39084 = LINE ( 'NONE', #14567, #27300 ) ;
#39085 = CARTESIAN_POINT ( 'NONE',  ( -1.765272865745179498, -30.05733663009887024, 7.754798119455333705 ) ) ;
#39086 = CARTESIAN_POINT ( 'NONE',  ( -0.5125101069461960313, -26.98863734761392053, 7.703977250142846955 ) ) ;
#39087 = ORIENTED_EDGE ( 'NONE', *, *, #23159, .F. ) ;
#39088 = CARTESIAN_POINT ( 'NONE',  ( -32.97867591359219119, -26.64985754041175525, 6.700000000000000178 ) ) ;
#39089 = AXIS2_PLACEMENT_3D ( 'NONE', #25860, #35549, #6728 ) ;
#39090 = DIRECTION ( 'NONE',  ( 0.000000000000000000, 0.000000000000000000, 1.000000000000000000 ) ) ;
#39091 = CARTESIAN_POINT ( 'NONE',  ( -1.179709461578283269, -27.76296156357867417, 6.863904403958576594 ) ) ;
#39092 = EDGE_LOOP ( 'NONE', ( #27266, #14483, #12589, #22658 ) ) ;
#39093 = ORIENTED_EDGE ( 'NONE', *, *, #37075, .F. ) ;
#39094 = CARTESIAN_POINT ( 'NONE',  ( 33.11343782431677596, -0.1514955757993836083, 4.942505121863887574 ) ) ;
#39095 = CARTESIAN_POINT ( 'NONE',  ( 2.118382188679144296, -33.04488093583253061, 6.941203072598475465 ) ) ;
#39096 = CARTESIAN_POINT ( 'NONE',  ( -0.5243941317258925539, -32.27184342263215200, 7.670465701733752972 ) ) ;
#39097 = CARTESIAN_POINT ( 'NONE',  ( 33.44054677433027933, -3.435571797939218186, 5.408185224205094954 ) ) ;
#39098 = CYLINDRICAL_SURFACE ( 'NONE', #32346, 2.500000000000002220 ) ;
#39099 = ORIENTED_EDGE ( 'NONE', *, *, #23790, .T. ) ;
#39100 = EDGE_LOOP ( 'NONE', ( #4507, #6744, #30776, #7164 ) ) ;
#39101 = CARTESIAN_POINT ( 'NONE',  ( -70.92837670882107659, -60.53509472482660669, 0.000000000000000000 ) ) ;
#39102 = B_SPLINE_CURVE_WITH_KNOTS ( 'NONE', 3,
 ( #2704, #31094, #2905, #15424, #27984, #40531, #24912, #9245, #21822, #31701 ),
 .UNSPECIFIED., .F., .F.,
 ( 4, 2, 2, 2, 4 ),
 ( 0.001566336636202482393, 0.001957536639217858504, 0.002348736642233234181, 0.002739936645248610293, 0.003131136648263986404 ),
 .UNSPECIFIED. ) ;
#39103 = CARTESIAN_POINT ( 'NONE',  ( -6.448748702180637338, -25.49307895267003587, 6.700000000000000178 ) ) ;
#39105 = CARTESIAN_POINT ( 'NONE',  ( -9.796229648729232409, -33.54387950140292673, -2.500000000000000000 ) ) ;
#39104 = DIRECTION ( 'NONE',  ( -0.000000000000000000, -0.000000000000000000, -1.000000000000000000 ) ) ;
#39106 = ORIENTED_EDGE ( 'NONE', *, *, #13667, .T. ) ;
#39107 = CARTESIAN_POINT ( 'NONE',  ( 23.93134969406609969, 3.254905450091994279, 3.508261123597265385 ) ) ;
#39108 = CARTESIAN_POINT ( 'NONE',  ( 81.53194397951688188, 65.66224036380454265, -1.718006205139864795 ) ) ;
#39109 = AXIS2_PLACEMENT_3D ( 'NONE', #34787, #15399, #12310 ) ;
#39110 = CIRCLE ( 'NONE', #31918, 3.499999999999999556 ) ;
#39111 = DIRECTION ( 'NONE',  ( 1.000000000000000000, 0.000000000000000000, 0.000000000000000000 ) ) ;
#39112 = VERTEX_POINT ( 'NONE', #6320 ) ;
#39113 = VECTOR ( 'NONE', #4436, 1000.000000000000000 ) ;
#39115 = CARTESIAN_POINT ( 'NONE',  ( 16.15910822604420716, -3.328347674494501973, -2.728417666820209586 ) ) ;
#39114 = CARTESIAN_POINT ( 'NONE',  ( 0.1069670619869697303, -26.56643171602332032, 7.754798119455333705 ) ) ;
#39116 = CARTESIAN_POINT ( 'NONE',  ( 22.37801635562015079, 5.219640035649274701, -3.555971675700331680 ) ) ;
#39117 = CARTESIAN_POINT ( 'NONE',  ( 75.00613679496295561, 61.08591394029932076, 3.912919437578906035 ) ) ;
#39118 = CARTESIAN_POINT ( 'NONE',  ( 22.04692162351881279, 3.100284280110099377, -4.816771713714539160 ) ) ;
#39119 = CARTESIAN_POINT ( 'NONE',  ( -30.24874870218063450, -26.64985754041175525, 6.800000000000000711 ) ) ;
#39120 = AXIS2_PLACEMENT_3D ( 'NONE', #10794, #39615, #33477 ) ;
#39121 = DIRECTION ( 'NONE',  ( -1.000000000000000000, -5.786005779812646808E-17, 0.000000000000000000 ) ) ;
#39122 = CARTESIAN_POINT ( 'NONE',  ( 22.14407712215583501, 4.579442068576085489, -3.662516810078165097 ) ) ;
#39123 = DIRECTION ( 'NONE',  ( 1.000000000000000000, -0.000000000000000000, 0.000000000000000000 ) ) ;
#39124 = CARTESIAN_POINT ( 'NONE',  ( -20.24874870218063805, -25.49307895267003587, 6.700000000000000178 ) ) ;
#39125 = CARTESIAN_POINT ( 'NONE',  ( 80.84167751523420975, 65.66068717198515969, 2.558871340112365278 ) ) ;
#39126 = CARTESIAN_POINT ( 'NONE',  ( 86.56125476490799997, 1.128014799767447229, 4.962829853851403961 ) ) ;
#39127 = CARTESIAN_POINT ( 'NONE',  ( 32.22946493318451644, -2.099509172777830557, 5.989391533279509794 ) ) ;
#39128 = CARTESIAN_POINT ( 'NONE',  ( -0.4475183596422435683, -26.93431084857535751, 6.894806418505348589 ) ) ;
#39129 = EDGE_CURVE ( 'NONE', #22571, #39924, #10001, .T. ) ;
#39130 = EDGE_CURVE ( 'NONE', #18363, #9395, #31643, .T. ) ;
#39131 = FACE_OUTER_BOUND ( 'NONE', #21035, .T. ) ;
#39132 = CARTESIAN_POINT ( 'NONE',  ( -0.5240671274847170658, -32.14127148892561792, 6.892063359921933419 ) ) ;
#39133 = EDGE_CURVE ( 'NONE', #35180, #33558, #25418, .T. ) ;
#39134 = CARTESIAN_POINT ( 'NONE',  ( 21.48247305285511288, 3.876926268098481287, -3.508130033835277217 ) ) ;
#39135 = CARTESIAN_POINT ( 'NONE',  ( -70.92837670882107659, -56.35932253828836025, -5.950000000000010836 ) ) ;
#39136 = CARTESIAN_POINT ( 'NONE',  ( -1.713032059046489142, -28.79627056164295595, 7.013842709614101167 ) ) ;
#39137 = CARTESIAN_POINT ( 'NONE',  ( -63.35138607920025322, 42.45142311247835920, -3.729943156278033189 ) ) ;
#39138 = AXIS2_PLACEMENT_3D ( 'NONE', #2871, #8795, #28577 ) ;
#39139 = CARTESIAN_POINT ( 'NONE',  ( 5.651251297819362307, -25.49307895267003587, 6.700000000000000178 ) ) ;
#39140 = AXIS2_PLACEMENT_3D ( 'NONE', #29696, #1508, #24742 ) ;
#39141 = VERTEX_POINT ( 'NONE', #15978 ) ;
#39142 = CARTESIAN_POINT ( 'NONE',  ( 35.10416124133201521, -1.272529116935883442, 5.608947908793178172 ) ) ;
#39143 = CARTESIAN_POINT ( 'NONE',  ( -70.48694192573870509, 0.1213051481704135875, 3.984496351204983355 ) ) ;
#39144 = CARTESIAN_POINT ( 'NONE',  ( 67.08333554474984339, 58.24655189615426565, -3.990981480864018938 ) ) ;
#39145 = VECTOR ( 'NONE', #1598, 1000.000000000000000 ) ;
#39146 = CARTESIAN_POINT ( 'NONE',  ( -1.343227611574053348, -27.84180251125378902, 7.651421919295147589 ) ) ;
#39147 = ORIENTED_EDGE ( 'NONE', *, *, #3856, .F. ) ;
#39148 = LINE ( 'NONE', #7867, #22663 ) ;
#39149 = CARTESIAN_POINT ( 'NONE',  ( 86.01040231118156498, 0.2354137643325349138, -5.999916684876917650 ) ) ;
#39150 = CARTESIAN_POINT ( 'NONE',  ( 3.340113934647170435, -32.66206629357650115, 7.750000000000000888 ) ) ;
#39151 = DIRECTION ( 'NONE',  ( -0.000000000000000000, 1.000000000000000000, -0.000000000000000000 ) ) ;
#39152 = CARTESIAN_POINT ( 'NONE',  ( 0.4689551980386493235, -32.84614736048875017, 6.888594555015729703 ) ) ;
#39153 = CARTESIAN_POINT ( 'NONE',  ( 1.283089764802823218, -26.09489629076599115, 6.961115707816241560 ) ) ;
#39154 = ORIENTED_EDGE ( 'NONE', *, *, #7628, .T. ) ;
#39155 = CARTESIAN_POINT ( 'NONE',  ( 23.43424776407714916, 3.789913264566200368, 3.112445696235128345 ) ) ;
#39156 = FACE_OUTER_BOUND ( 'NONE', #18807, .T. ) ;
#39157 = CARTESIAN_POINT ( 'NONE',  ( 80.51591231855054787, 63.60920045316173344, 3.640670270625566030 ) ) ;
#39158 = DIRECTION ( 'NONE',  ( 0.000000000000000000, 0.000000000000000000, 1.000000000000000000 ) ) ;
#39159 = ORIENTED_EDGE ( 'NONE', *, *, #19993, .F. ) ;
#39160 = CARTESIAN_POINT ( 'NONE',  ( 78.61725963159940989, 63.00713372587870964, -3.804514705604311153 ) ) ;
#39162 = CARTESIAN_POINT ( 'NONE',  ( -1.737164628395478694, -28.91167429922809973, 6.877267274870244584 ) ) ;
#39161 = CARTESIAN_POINT ( 'NONE',  ( 24.12566071183585237, 0.5138664147065530319, 5.092652492612476323 ) ) ;
#39163 = CARTESIAN_POINT ( 'NONE',  ( 79.86705713782787086, 65.75210810416335505, -2.684801069570281751 ) ) ;
#39164 = CARTESIAN_POINT ( 'NONE',  ( 77.82439497328331868, 65.16220298991649429, 2.551779361026667470 ) ) ;
#39165 = VECTOR ( 'NONE', #9577, 1000.000000000000000 ) ;
#39166 = DIRECTION ( 'NONE',  ( -0.3754033771448320178, 0.6502177225477884237, -0.6605219282605403475 ) ) ;
#39167 = CIRCLE ( 'NONE', #14163, 2.500000000000000444 ) ;
#39168 = CARTESIAN_POINT ( 'NONE',  ( 82.26973386304365476, 64.90130211351629441, 1.165579324820864571 ) ) ;
#39169 =( BOUNDED_CURVE ( )  B_SPLINE_CURVE ( 3, ( #4633, #29732, #14281, #1159 ),
 .UNSPECIFIED., .F., .T. ) 
 B_SPLINE_CURVE_WITH_KNOTS ( ( 4, 4 ),
 ( 1.381924640371168245, 1.574767692156076038 ),
 .UNSPECIFIED. ) 
 CURVE ( )  GEOMETRIC_REPRESENTATION_ITEM ( )  RATIONAL_B_SPLINE_CURVE ( ( 1.000000000000000000, 0.9969033633783033199, 0.9969033633783033199, 1.000000000000000000 ) ) 
 REPRESENTATION_ITEM ( '' )  );
#39171 = EDGE_LOOP ( 'NONE', ( #26505, #38087, #15664, #27118 ) ) ;
#39170 = FACE_OUTER_BOUND ( 'NONE', #32565, .T. ) ;
#39172 = CARTESIAN_POINT ( 'NONE',  ( 23.92067639343244778, 4.177307434159622801, 1.236145424036337426 ) ) ;
#39173 = CARTESIAN_POINT ( 'NONE',  ( -64.09407456991024787, 35.62175799955578981, -4.126536650000701023 ) ) ;
#39174 = ORIENTED_EDGE ( 'NONE', *, *, #14815, .T. ) ;
#39175 = CARTESIAN_POINT ( 'NONE',  ( -80.93421692491173758, -5.699880070350716643, 0.2256805699841040458 ) ) ;
#39176 = CARTESIAN_POINT ( 'NONE',  ( 25.39387711625591848, 0.7059127421703671468, -4.600211075182401466 ) ) ;
#39177 = VECTOR ( 'NONE', #4805, 1000.000000000000000 ) ;
#39178 = CYLINDRICAL_SURFACE ( 'NONE', #28111, 117.6618724293813898 ) ;
#39179 = ORIENTED_EDGE ( 'NONE', *, *, #24723, .T. ) ;
#39180 = CARTESIAN_POINT ( 'NONE',  ( 5.171756705836403789, -29.12309438737783651, 6.887547729233691740 ) ) ;
#39181 = EDGE_CURVE ( 'NONE', #12640, #22571, #28544, .T. ) ;
#39182 = CARTESIAN_POINT ( 'NONE',  ( 34.78593673359796412, -3.774928924632479976, -5.430219759624750786 ) ) ;
#39183 = CARTESIAN_POINT ( 'NONE',  ( -4.224659823956008253, -51.67615071827237472, 6.000000000000000000 ) ) ;
#39184 = CARTESIAN_POINT ( 'NONE',  ( 5.112950570154877639, -30.34738380003949487, 7.009310105710484962 ) ) ;
#39186 = CARTESIAN_POINT ( 'NONE',  ( -71.02793705302472915, -48.61702805680359774, 6.000000000000004441 ) ) ;
#39185 = B_SPLINE_CURVE_WITH_KNOTS ( 'NONE', 3,
 ( #14196, #19781, #13803, #17269, #32552, #10497, #39306, #32950, #26370, #20368 ),
 .UNSPECIFIED., .F., .F.,
 ( 4, 3, 3, 4 ),
 ( 0.0001585009270395684592, 0.0001815657551981856850, 0.0002118214035944121260, 0.0002170292169044726936 ),
 .UNSPECIFIED. ) ;
#39187 = DIRECTION ( 'NONE',  ( 1.000000000000000000, 0.000000000000000000, 0.000000000000000000 ) ) ;
#39188 = PLANE ( 'NONE',  #719 ) ;
#39189 = CARTESIAN_POINT ( 'NONE',  ( 1.870087168943759703, -26.07404647501646622, 6.895394898881668233 ) ) ;
#39190 =( REPRESENTATION_RELATIONSHIP ('NONE','NONE', #24012, #131 ) REPRESENTATION_RELATIONSHIP_WITH_TRANSFORMATION ( #30577 )SHAPE_REPRESENTATION_RELATIONSHIP( ) );
#39191 = ORIENTED_EDGE ( 'NONE', *, *, #2114, .T. ) ;
#39192 = ORIENTED_EDGE ( 'NONE', *, *, #28084, .F. ) ;
#39193 = CARTESIAN_POINT ( 'NONE',  ( 66.27376694608996388, 57.73522568913447373, 4.000000000000000000 ) ) ;
#39194 = CARTESIAN_POINT ( 'NONE',  ( 71.23183612236115891, 58.76351790733232860, -3.862811858476256077 ) ) ;
#39195 = ORIENTED_EDGE ( 'NONE', *, *, #17982, .T. ) ;
#39196 = CARTESIAN_POINT ( 'NONE',  ( 86.38495421312710221, -0.4360953479145894263, -5.826368990767747391 ) ) ;
#39197 = CARTESIAN_POINT ( 'NONE',  ( -60.14275962559869981, 24.84364830758654108, 9.154021781743367114 ) ) ;
#39198 = PLANE ( 'NONE',  #27435 ) ;
#39199 = CARTESIAN_POINT ( 'NONE',  ( -1.015649984579921172, -27.51298068758381277, 7.139196562012270597 ) ) ;
#39200 = DIRECTION ( 'NONE',  ( -0.000000000000000000, -0.000000000000000000, 1.000000000000000000 ) ) ;
#39201 = EDGE_CURVE ( 'NONE', #13011, #6524, #16382, .T. ) ;
#39202 = APPLICATION_PROTOCOL_DEFINITION ( 'draft international standard', 'automotive_design', 1998, #33465 ) ;
#39203 = AXIS2_PLACEMENT_3D ( 'NONE', #26390, #32575, #3775 ) ;
#39204 = DIRECTION ( 'NONE',  ( -0.4690749385695702212, -0.8831583674550980145, 0.000000000000000000 ) ) ;
#39205 = CARTESIAN_POINT ( 'NONE',  ( -26.87867591359219333, -26.64985754041175525, 6.700000000000000178 ) ) ;
#39206 = CARTESIAN_POINT ( 'NONE',  ( -10.24874870218063450, -26.64985754041175525, 6.700000000000000178 ) ) ;
#39207 = CARTESIAN_POINT ( 'NONE',  ( 23.63366851782300770, -3.140391636472827930, 3.778057570207932425 ) ) ;
#39208 = ORIENTED_EDGE ( 'NONE', *, *, #34910, .T. ) ;
#39209 = CARTESIAN_POINT ( 'NONE',  ( 80.63281215842000904, 62.09153919268369037, -3.087291694836846290 ) ) ;
#39210 = CARTESIAN_POINT ( 'NONE',  ( 15.43177750874984433, 12.90197807773783367, -2.500000000000005773 ) ) ;
#39211 = CARTESIAN_POINT ( 'NONE',  ( 80.91431153141797950, 61.21107275232134981, 1.487544896895754309 ) ) ;
#39212 = DIRECTION ( 'NONE',  ( 1.000000000000000000, 0.000000000000000000, 0.000000000000000000 ) ) ;
#39213 = EDGE_CURVE ( 'NONE', #24867, #20522, #13559, .T. ) ;
#39214 = CARTESIAN_POINT ( 'NONE',  ( 0.3883083225179605469, -32.81460370194803744, 7.753200566781576875 ) ) ;
#39215 = CARTESIAN_POINT ( 'NONE',  ( 4.025803068412391106, -27.08951600530382464, 7.013842709614101167 ) ) ;
#39216 = FACE_OUTER_BOUND ( 'NONE', #37439, .T. ) ;
#39217 = CARTESIAN_POINT ( 'NONE',  ( 21.85643539959774273, -10.14878426894149221, 9.991042268249278990 ) ) ;
#39218 = LINE ( 'NONE', #11008, #5535 ) ;
#39219 = EDGE_LOOP ( 'NONE', ( #21148, #37214, #20173, #36835 ) ) ;
#39220 = CARTESIAN_POINT ( 'NONE',  ( -28.87867591359218977, -26.64985754041175525, 6.700000000000000178 ) ) ;
#39221 = CARTESIAN_POINT ( 'NONE',  ( 14.74185191083505231, -5.107022699585343162, 2.499999999999729106 ) ) ;
#39222 = AXIS2_PLACEMENT_3D ( 'NONE', #28776, #38630, #13122 ) ;
#39223 = CARTESIAN_POINT ( 'NONE',  ( -79.25808045669066360, 11.47437878731752647, -5.548284614561191042 ) ) ;
#39224 = EDGE_CURVE ( 'NONE', #39701, #38197, #36334, .T. ) ;
#39225 = CARTESIAN_POINT ( 'NONE',  ( 1.493817720656384518, -32.96364906610717327, 6.929923840112063971 ) ) ;
#39226 = CARTESIAN_POINT ( 'NONE',  ( 37.00891459296443031, -3.247065243002688284, -5.946827200946571246 ) ) ;
#39227 = CARTESIAN_POINT ( 'NONE',  ( 79.50768156050781954, 65.53910429656815495, 2.885071930847944444 ) ) ;
#39228 = DIRECTION ( 'NONE',  ( 0.000000000000000000, 0.000000000000000000, 1.000000000000000000 ) ) ;
#39229 = LINE ( 'NONE', #29576, #13469 ) ;
#39230 = CARTESIAN_POINT ( 'NONE',  ( 4.921324086407802056, -26.64985754041175525, 6.700000000000000178 ) ) ;
#39231 = CARTESIAN_POINT ( 'NONE',  ( 28.38512348074436886, 0.6183906642395941011, 4.636583034612477228 ) ) ;
#39232 = VECTOR ( 'NONE', #25232, 1000.000000000000000 ) ;
#39233 = VECTOR ( 'NONE', #22321, 1000.000000000000000 ) ;
#39234 = CARTESIAN_POINT ( 'NONE',  ( 3.975236603202493946, -32.22983402974450229, 7.720710062488896241 ) ) ;
#39235 = CARTESIAN_POINT ( 'NONE',  ( 87.35850478739605762, 0.2325057347401545127, 4.553521783490353414 ) ) ;
#39236 = CARTESIAN_POINT ( 'NONE',  ( 4.196096248743072188, -31.87893844532966980, 6.876076431790008492 ) ) ;
#39237 = CARTESIAN_POINT ( 'NONE',  ( 68.09143390058649459, 58.21448531840948704, 3.990965707299598098 ) ) ;
#39238 = CARTESIAN_POINT ( 'NONE',  ( 34.77301380135100572, -3.165686779924592020, 5.633567810854094304 ) ) ;
#39239 = EDGE_CURVE ( 'NONE', #30063, #9233, #25043, .T. ) ;
#39240 = CARTESIAN_POINT ( 'NONE',  ( 0.9419643339933850834, -26.24837854292180950, 7.139196562012272373 ) ) ;
#39241 = CARTESIAN_POINT ( 'NONE',  ( 84.79809517660038409, 3.058972130929652256, -0.4747855469284483210 ) ) ;
#39243 = DIRECTION ( 'NONE',  ( 0.000000000000000000, 0.000000000000000000, 1.000000000000000000 ) ) ;
#39242 = CARTESIAN_POINT ( 'NONE',  ( 80.30248525907990143, 64.25517361537380623, -3.614389211669654323 ) ) ;
#39244 = CARTESIAN_POINT ( 'NONE',  ( 5.198120437317888864, -29.69595573662939358, 7.750000000000000888 ) ) ;
#39245 = CARTESIAN_POINT ( 'NONE',  ( -58.56173084424084863, 30.28994157939056819, 5.156891857687778469 ) ) ;
#39246 = ORIENTED_EDGE ( 'NONE', *, *, #29433, .T. ) ;
#39247 = CARTESIAN_POINT ( 'NONE',  ( -80.14709680133751135, 11.51107841541166010, -3.897538531476514745 ) ) ;
#39248 = CARTESIAN_POINT ( 'NONE',  ( 1.317233406660536232, -26.19158762211118585, 6.939395833800440450 ) ) ;
#39249 = ORIENTED_EDGE ( 'NONE', *, *, #29895, .T. ) ;
#39250 = CARTESIAN_POINT ( 'NONE',  ( -71.92837670882107659, -20.89404664731295114, 3.916079783099609912 ) ) ;
#39251 = VECTOR ( 'NONE', #9207, 1000.000000000000000 ) ;
#39252 = CARTESIAN_POINT ( 'NONE',  ( 81.04993867939947449, 61.73413400689819497, -2.516896548562718383 ) ) ;
#39253 = EDGE_CURVE ( 'NONE', #30342, #35091, #34638, .T. ) ;
#39254 = CARTESIAN_POINT ( 'NONE',  ( 4.993907954365692348, -30.75430347691218813, 7.635761828346578461 ) ) ;
#39255 = EDGE_CURVE ( 'NONE', #33383, #2110, #31140, .T. ) ;
#39256 = VECTOR ( 'NONE', #18376, 1000.000000000000000 ) ;
#39257 = CARTESIAN_POINT ( 'NONE',  ( 78.97848303377290335, 65.71588112483786404, 2.516896548562567837 ) ) ;
#39258 = CARTESIAN_POINT ( 'NONE',  ( 24.77959113649616540, 1.432599100595700614, 4.541996434422298279 ) ) ;
#39260 = ORIENTED_EDGE ( 'NONE', *, *, #5391, .F. ) ;
#39259 = LINE ( 'NONE', #26916, #13801 ) ;
#39261 = AXIS2_PLACEMENT_3D ( 'NONE', #28948, #18645, #3050 ) ;
#39262 = EDGE_CURVE ( 'NONE', #12173, #11301, #15368, .T. ) ;
#39263 = PLANE ( 'NONE',  #21325 ) ;
#39265 = CARTESIAN_POINT ( 'NONE',  ( 15.70794464946376223, 12.77956130056348272, 2.499999999999996003 ) ) ;
#39264 = CARTESIAN_POINT ( 'NONE',  ( -4.108956827130609367E-15, 0.5999999999999995337, -3.779699080088179564 ) ) ;
#39266 = CARTESIAN_POINT ( 'NONE',  ( -1.181303964486304814, -27.76553572604635534, 7.754798119455333705 ) ) ;
#39267 = CARTESIAN_POINT ( 'NONE',  ( 4.651604549657131216, -31.25822317698004227, 7.635761828346577573 ) ) ;
#39268 = CARTESIAN_POINT ( 'NONE',  ( 23.70771619120949936, 3.501700497104693000, -3.333794200282627074 ) ) ;
#39269 = ORIENTED_EDGE ( 'NONE', *, *, #27126, .F. ) ;
#39270 = CARTESIAN_POINT ( 'NONE',  ( 5.121331332881381648, -30.25958242544057342, 7.780491323090173772 ) ) ;
#39271 = ORIENTED_EDGE ( 'NONE', *, *, #33943, .F. ) ;
#39272 = CARTESIAN_POINT ( 'NONE',  ( 22.31814515643556263, 6.191369071892208531, -1.397765879422002033 ) ) ;
#39273 = B_SPLINE_CURVE_WITH_KNOTS ( 'NONE', 3,
 ( #1022, #4508, #7180, #10260, #10854, #32714, #13555, #1229, #32316, #1423, #16629, #23627, #23433 ),
 .UNSPECIFIED., .F., .F.,
 ( 4, 3, 3, 3, 4 ),
 ( 0.0002076538946377561555, 0.0002109707048517078375, 0.0002426195318110312908, 0.0002740640997890035277, 0.0002849778069099851785 ),
 .UNSPECIFIED. ) ;
#39274 = CARTESIAN_POINT ( 'NONE',  ( 21.89858680184175199, 3.819795205001112137, 2.126311674330342072 ) ) ;
#39275 = CARTESIAN_POINT ( 'NONE',  ( 15.99304516048508340, 7.920163621858975489, 3.484773800358847318 ) ) ;
#39276 = EDGE_CURVE ( 'NONE', #5299, #29204, #32856, .T. ) ;
#39277 = ORIENTED_EDGE ( 'NONE', *, *, #21498, .T. ) ;
#39278 = CARTESIAN_POINT ( 'NONE',  ( 1.028547726584102762, -32.99064601744363046, 7.784725160561909441 ) ) ;
#39279 = CARTESIAN_POINT ( 'NONE',  ( 80.00444560209926692, 65.54189868873926628, 2.943961322784983459 ) ) ;
#39280 = CARTESIAN_POINT ( 'NONE',  ( 84.36655727669636917, 3.025886916471207222, -1.294691096651311435 ) ) ;
#39281 = CARTESIAN_POINT ( 'NONE',  ( 5.986119168300054305, -26.95491573082899706, 7.754798119455333705 ) ) ;
#39282 = VERTEX_POINT ( 'NONE', #1765 ) ;
#39283 = FACE_OUTER_BOUND ( 'NONE', #22723, .T. ) ;
#39284 = AXIS2_PLACEMENT_3D ( 'NONE', #33277, #21119, #27280 ) ;
#39285 = PLANE ( 'NONE',  #655 ) ;
#39286 = CARTESIAN_POINT ( 'NONE',  ( 23.82868741420347192, -2.964576112339935232, -3.895336304183651510 ) ) ;
#39287 = CARTESIAN_POINT ( 'NONE',  ( 37.04299532825181274, -2.892526904198844395, -5.987853327837934891 ) ) ;
#39288 = DIRECTION ( 'NONE',  ( 0.1542073060391599970, 0.000000000000000000, 0.9880385148181951571 ) ) ;
#39289 = CARTESIAN_POINT ( 'NONE',  ( 22.65759398342077091, 0.3095578120561012225, -6.438391604401149770 ) ) ;
#39290 = SHAPE_REPRESENTATION ( 'Triangular punching die', ( #30744 ), #15591 ) ;
#39291 = DIRECTION ( 'NONE',  ( 0.000000000000000000, 0.6834397476448857978, 0.7300069255418710767 ) ) ;
#39292 = ORIENTED_EDGE ( 'NONE', *, *, #811, .F. ) ;
#39293 = CARTESIAN_POINT ( 'NONE',  ( 35.86761721751184240, -2.089954870031187628, 5.804407147029888137 ) ) ;
#39294 = EDGE_CURVE ( 'NONE', #8622, #30983, #33259, .T. ) ;
#39295 = DIRECTION ( 'NONE',  ( 0.000000000000000000, 0.000000000000000000, 1.000000000000000000 ) ) ;
#39296 = CARTESIAN_POINT ( 'NONE',  ( 30.71212904023629520, -2.930635124035476657, -4.999768531013319084 ) ) ;
#39297 = ORIENTED_EDGE ( 'NONE', *, *, #3152, .F. ) ;
#39298 = ORIENTED_EDGE ( 'NONE', *, *, #8349, .T. ) ;
#39299 = CARTESIAN_POINT ( 'NONE',  ( 36.49335442002869456, -3.559127862921612984, 5.796824973035940687 ) ) ;
#39300 = DIRECTION ( 'NONE',  ( -0.000000000000000000, -0.000000000000000000, 1.000000000000000000 ) ) ;
#39301 = CARTESIAN_POINT ( 'NONE',  ( 33.45749450797183044, -3.829747548865578555, 5.093667367007288505 ) ) ;
#39302 = EDGE_CURVE ( 'NONE', #3866, #3076, #16835, .T. ) ;
#39303 = CARTESIAN_POINT ( 'NONE',  ( 86.10475594078930328, 0.05610482897665627217, 5.990085204934172403 ) ) ;
#39304 = ORIENTED_EDGE ( 'NONE', *, *, #2791, .F. ) ;
#39305 = EDGE_CURVE ( 'NONE', #22934, #36468, #1189, .T. ) ;
#39306 = CARTESIAN_POINT ( 'NONE',  ( 5.140819687086514378, -28.92693390833609612, 7.700536657684214248 ) ) ;
#39307 =( LENGTH_UNIT ( ) NAMED_UNIT ( * ) SI_UNIT ( .MILLI., .METRE. ) );
#39308 = LINE ( 'NONE', #10899, #19446 ) ;
#39309 = CARTESIAN_POINT ( 'NONE',  ( 4.763064956553218821, -27.87579221007247199, 6.870737987065014707 ) ) ;
#39310 = ORIENTED_EDGE ( 'NONE', *, *, #32681, .T. ) ;
#39311 = CARTESIAN_POINT ( 'NONE',  ( 23.41023413628745331, 3.546567081235476593, 3.496136802669740362 ) ) ;
#39312 = ADVANCED_FACE ( 'NONE', ( #16980 ), #26072, .F. ) ;
#39313 = CARTESIAN_POINT ( 'NONE',  ( 81.80771926544778694, 61.88353390887438366, -1.601045042264586771 ) ) ;
#39314 = CARTESIAN_POINT ( 'NONE',  ( -39.07867591359219261, -26.64985754041175525, 6.800000000000000711 ) ) ;
#39315 = CARTESIAN_POINT ( 'NONE',  ( -40.97867591359219119, -26.64985754041175525, 6.700000000000000178 ) ) ;
#39316 = ORIENTED_EDGE ( 'NONE', *, *, #15147, .T. ) ;
#39318 = CARTESIAN_POINT ( 'NONE',  ( 16.15328323628989082, -3.330670468083324565, -2.727508536291139762 ) ) ;
#39317 = CARTESIAN_POINT ( 'NONE',  ( 0.1010915821888478394, -26.56955616128021092, 7.761597726988854085 ) ) ;
#39319 = CARTESIAN_POINT ( 'NONE',  ( 4.651604549657131216, -31.25822317698004227, 7.635761828346577573 ) ) ;
#39320 = CARTESIAN_POINT ( 'NONE',  ( 75.20156067606269801, 62.14723293136128746, 3.810661578667819960 ) ) ;
#39321 = ORIENTED_EDGE ( 'NONE', *, *, #6084, .T. ) ;
#39322 = CARTESIAN_POINT ( 'NONE',  ( 23.94801143228027840, 2.553151854112576835, -4.127014578414197388 ) ) ;
#39323 = ORIENTED_EDGE ( 'NONE', *, *, #29394, .T. ) ;
#39324 = CARTESIAN_POINT ( 'NONE',  ( -63.03213158086111179, 38.26878225442446535, 4.032857076801017016 ) ) ;
#39325 = VECTOR ( 'NONE', #33904, 1000.000000000000000 ) ;
#39326 = CARTESIAN_POINT ( 'NONE',  ( -55.62677557291493713, 30.95433239688068738, -1.979412988903662463 ) ) ;
#39327 = CARTESIAN_POINT ( 'NONE',  ( -54.01549048184568846, -30.38627270959228710, 4.800000000000001599 ) ) ;
#39328 = CARTESIAN_POINT ( 'NONE',  ( 4.281682929012584182, -27.35702998321412593, 7.695279973900954751 ) ) ;
#39329 = CARTESIAN_POINT ( 'NONE',  ( 1.685959272703401401, -26.06995981023128905, 7.636816916992233750 ) ) ;
#39330 = CARTESIAN_POINT ( 'NONE',  ( 79.70081467235792161, 66.18075109116949761, 1.965143080302226952 ) ) ;
#39331 = CARTESIAN_POINT ( 'NONE',  ( 87.79476240240137486, -0.2575195244695515639, -3.704994186184041194 ) ) ;
#39332 = CARTESIAN_POINT ( 'NONE',  ( 29.60575365153160732, -0.8332953136462766253, 6.005451346670388268 ) ) ;
#39333 = CARTESIAN_POINT ( 'NONE',  ( 4.659413201177963870, -31.24450194833492489, 7.730758795053803034 ) ) ;
#39334 = CARTESIAN_POINT ( 'NONE',  ( -75.69582718456990733, -3.730213777768353722, -10.20091118747310510 ) ) ;
#39335 = CARTESIAN_POINT ( 'NONE',  ( 26.28311404583794086, -3.249458262315999768, 4.182437110436346472 ) ) ;
#39336 = CARTESIAN_POINT ( 'NONE',  ( -0.02262473055865150268, -26.52342071894167574, 6.894806418505347700 ) ) ;
#39337 = AXIS2_PLACEMENT_3D ( 'NONE', #7633, #29466, #10108 ) ;
#39338 = CARTESIAN_POINT ( 'NONE',  ( 34.38869957687920476, -1.330714714903810769, -5.573586281450729096 ) ) ;
#39339 = CARTESIAN_POINT ( 'NONE',  ( 4.976842733950424424, -28.33913446795707358, 7.697032948437508182 ) ) ;
#39340 = CARTESIAN_POINT ( 'NONE',  ( -1.181303964486304814, -27.76553572604635534, 7.754798119455333705 ) ) ;
#39341 = EDGE_CURVE ( 'NONE', #10467, #29737, #22986, .T. ) ;
#39342 = DIRECTION ( 'NONE',  ( 0.000000000000000000, 0.000000000000000000, 1.000000000000000000 ) ) ;
#39343 = ORIENTED_EDGE ( 'NONE', *, *, #1371, .F. ) ;
#39344 = CARTESIAN_POINT ( 'NONE',  ( 27.67012909237472584, 1.632019845528506208, 4.348991244234835740 ) ) ;
#39345 = CARTESIAN_POINT ( 'NONE',  ( -64.08758708074091714, 38.55573457772874946, -3.000000000000000444 ) ) ;
#39346 = CARTESIAN_POINT ( 'NONE',  ( 67.52644525400921793, 57.94193659033309274, -3.989212576213370109 ) ) ;
#39347 = VECTOR ( 'NONE', #34737, 1000.000000000000000 ) ;
#39348 = CARTESIAN_POINT ( 'NONE',  ( -1.340340806711404209, -27.83673787031249347, 7.643192810543823157 ) ) ;
#39349 = VERTEX_POINT ( 'NONE', #19879 ) ;
#39350 = CARTESIAN_POINT ( 'NONE',  ( -0.5008017999313679747, -32.16123271495482072, 7.779495906702011077 ) ) ;
#39351 = EDGE_CURVE ( 'NONE', #9389, #19164, #6967, .T. ) ;
#39352 = CARTESIAN_POINT ( 'NONE',  ( 3.796401147549515631, -32.24700651031859877, 7.761597726988847867 ) ) ;
#39353 = CARTESIAN_POINT ( 'NONE',  ( 4.269670580072574495, -31.94665014585129725, 7.013842709614101167 ) ) ;
#39354 = DIRECTION ( 'NONE',  ( 0.000000000000000000, 0.000000000000000000, 1.000000000000000000 ) ) ;
#39355 = CARTESIAN_POINT ( 'NONE',  ( 0.3325954124718418226, -32.79160147188828489, 6.993830769476427456 ) ) ;
#39356 = DIRECTION ( 'NONE',  ( -0.000000000000000000, -0.000000000000000000, 1.000000000000000000 ) ) ;
#39357 = ORIENTED_EDGE ( 'NONE', *, *, #24676, .T. ) ;
#39358 = EDGE_CURVE ( 'NONE', #21657, #25871, #26468, .T. ) ;
#39359 = CARTESIAN_POINT ( 'NONE',  ( -1.740011302788441183, -30.21307731605675073, 7.695279973900954751 ) ) ;
#39360 = CARTESIAN_POINT ( 'NONE',  ( 79.53763471700084153, 65.25825451995498838, 3.163072811751573177 ) ) ;
#39361 = EDGE_CURVE ( 'NONE', #31581, #21319, #20225, .T. ) ;
#39362 = VECTOR ( 'NONE', #5103, 1000.000000000000000 ) ;
#39363 = CARTESIAN_POINT ( 'NONE',  ( -0.01837800939314764015, -32.61883756299590686, 7.686927408461906808 ) ) ;
#39364 = ORIENTED_EDGE ( 'NONE', *, *, #30745, .T. ) ;
#39365 = CARTESIAN_POINT ( 'NONE',  ( 77.77823160594137164, 63.95155898497984026, -3.535928464255530645 ) ) ;
#39367 = CARTESIAN_POINT ( 'NONE',  ( 14.73431651683273991, -4.754725209805407360, -2.504653360488686253 ) ) ;
#39366 = CARTESIAN_POINT ( 'NONE',  ( 25.40612371031801331, 0.6579664209402951158, 4.600295987165074152 ) ) ;
#39368 = CARTESIAN_POINT ( 'NONE',  ( 81.41826528542581798, 63.68099735521261096, -3.235508711551935424 ) ) ;
#39369 = CARTESIAN_POINT ( 'NONE',  ( 78.19518920554678232, 64.50268734400745529, 3.317372267376125894 ) ) ;
#39370 = ORIENTED_EDGE ( 'NONE', *, *, #7217, .F. ) ;
#39371 = CARTESIAN_POINT ( 'NONE',  ( -0.8782802225456025624, -27.35395321429220061, 7.784838882742138644 ) ) ;
#39372 = CARTESIAN_POINT ( 'NONE',  ( 82.04611962119309965, 65.17642557464539266, 1.633153239554254732 ) ) ;
#39374 = ORIENTED_EDGE ( 'NONE', *, *, #25078, .F. ) ;
#39373 = CARTESIAN_POINT ( 'NONE',  ( 66.41194937274630661, -13.65448019739280028, 6.000000000000001776 ) ) ;
#39375 = CARTESIAN_POINT ( 'NONE',  ( 28.41236345070440805, -1.224654026667450157, -6.045523132457580218 ) ) ;
#39376 = CARTESIAN_POINT ( 'NONE',  ( -62.83712641625177753, 35.61106514070151263, -5.789832448495768169 ) ) ;
#39377 = ORIENTED_EDGE ( 'NONE', *, *, #6719, .T. ) ;
#39378 = CARTESIAN_POINT ( 'NONE',  ( 5.200390093233090205, -29.56993018339339940, 7.800000000000000711 ) ) ;
#39379 = CARTESIAN_POINT ( 'NONE',  ( 26.75738543021116200, 0.8858420045314591151, -4.383008446193700003 ) ) ;
#39380 = DIRECTION ( 'NONE',  ( 0.7394003126383904556, 0.1303762246624302623, -0.6605219282605401254 ) ) ;
#39381 = CARTESIAN_POINT ( 'NONE',  ( 5.175262448506648738, -29.15127664070277547, 6.971170733404104425 ) ) ;
#39382 = CARTESIAN_POINT ( 'NONE',  ( -71.67963774732312743, -48.41903106474732255, 9.972075897659857802 ) ) ;
#39383 = CARTESIAN_POINT ( 'NONE',  ( 32.06786553091724556, 0.2506460099112566287, -4.730677192303592626 ) ) ;
#39384 = CARTESIAN_POINT ( 'NONE',  ( 3.465471057152984091, -32.59226193070500699, 7.750000000000000000 ) ) ;
#39385 = B_SPLINE_CURVE_WITH_KNOTS ( 'NONE', 3,
 ( #26294, #35960, #1388, #19705, #35571, #26490, #4080, #16996, #23004, #13310 ),
 .UNSPECIFIED., .F., .F.,
 ( 4, 3, 3, 4 ),
 ( 0.0002170292169044726936, 0.0002420761345915969052, 0.0002723302478206978718, 0.0002816811360866732774 ),
 .UNSPECIFIED. ) ;
#39386 = CARTESIAN_POINT ( 'NONE',  ( 3.432076046773545386, -32.50414549462902158, 7.257242401810562349 ) ) ;
#39387 = CARTESIAN_POINT ( 'NONE',  ( -1.099610869996748841, -31.66993096438462629, 6.971170733404106201 ) ) ;
#39388 = FACE_OUTER_BOUND ( 'NONE', #15020, .T. ) ;
#39389 = CARTESIAN_POINT ( 'NONE',  ( 2.755104336738883219, -32.80220150006005753, 6.864276522220859711 ) ) ;
#39390 = CARTESIAN_POINT ( 'NONE',  ( 5.094108975946863183, -29.77650255597014350, 6.929923840112069300 ) ) ;
#39391 = CARTESIAN_POINT ( 'NONE',  ( 1.774512685358780928, -26.07070055451856305, 6.867280401193708528 ) ) ;
#39392 = CARTESIAN_POINT ( 'NONE',  ( 21.78485685878760947, 1.220823519683512437, -7.120777440962641869 ) ) ;
#39393 = CIRCLE ( 'NONE', #2644, 82.54614097552274643 ) ;
#39394 = VERTEX_POINT ( 'NONE', #6069 ) ;
#39395 = CARTESIAN_POINT ( 'NONE',  ( 66.27376694608996388, 57.73522568913447373, 4.000000000000000000 ) ) ;
#39396 = PRODUCT_DEFINITION ( 'UNKNOWN', '', #22862, #39452 ) ;
#39397 = CARTESIAN_POINT ( 'NONE',  ( 73.28086911227147482, 60.35416371166882499, -3.944160774611113585 ) ) ;
#39398 = ORIENTED_EDGE ( 'NONE', *, *, #5963, .T. ) ;
#39399 = MANIFOLD_SOLID_BREP ( 'Move Face3', #24234 ) ;
#39400 = CARTESIAN_POINT ( 'NONE',  ( 87.87138265328074738, -2.102315541244656583, 2.954904511526853295 ) ) ;
#39401 = CARTESIAN_POINT ( 'NONE',  ( 0.1848793752431239501, -26.52637391292726932, 6.939395833800441338 ) ) ;
#39402 = CARTESIAN_POINT ( 'NONE',  ( 0.4906401998943609177, -26.28564864924214461, 7.635761828346577573 ) ) ;
#39403 = PLANE ( 'NONE',  #3806 ) ;
#39404 = LINE ( 'NONE', #17992, #17259 ) ;
#39405 = DIRECTION ( 'NONE',  ( -0.000000000000000000, -0.000000000000000000, -1.000000000000000000 ) ) ;
#39406 = VECTOR ( 'NONE', #15986, 1000.000000000000000 ) ;
#39407 = EDGE_CURVE ( 'NONE', #28211, #16705, #8961, .T. ) ;
#39408 = CARTESIAN_POINT ( 'NONE',  ( 3.055030623276686619, -26.34271016697629619, 7.013842709614101167 ) ) ;
#39409 = EDGE_CURVE ( 'NONE', #5157, #30864, #8524, .T. ) ;
#39410 = ORIENTED_EDGE ( 'NONE', *, *, #25124, .F. ) ;
#39411 = CARTESIAN_POINT ( 'NONE',  ( 79.14523234120532891, 64.60782394083948077, -3.482780605906210525 ) ) ;
#39412 =( BOUNDED_CURVE ( )  B_SPLINE_CURVE ( 3, ( #10086, #7006, #10486, #13584 ),
 .UNSPECIFIED., .F., .T. ) 
 B_SPLINE_CURVE_WITH_KNOTS ( ( 4, 4 ),
 ( 4.748221474220560623, 4.941946782021394924 ),
 .UNSPECIFIED. ) 
 CURVE ( )  GEOMETRIC_REPRESENTATION_ITEM ( )  RATIONAL_B_SPLINE_CURVE ( ( 1.000000000000000000, 0.9968749865767494445, 0.9968749865767494445, 1.000000000000000000 ) ) 
 REPRESENTATION_ITEM ( '' )  );
#39413 = CARTESIAN_POINT ( 'NONE',  ( 17.53685894859813388, 11.96893683007039044, -2.499999999999995115 ) ) ;
#39414 = CARTESIAN_POINT ( 'NONE',  ( 80.53463578537552792, 62.06606814882641743, 3.115013800517338005 ) ) ;
#39415 = CARTESIAN_POINT ( 'NONE',  ( 0.6039493587051372181, -26.35155809456087184, 7.784476445165072533 ) ) ;
#39416 = DIRECTION ( 'NONE',  ( -0.000000000000000000, -0.000000000000000000, 1.000000000000000000 ) ) ;
#39417 = CIRCLE ( 'NONE', #21043, 0.1000000000000028644 ) ;
#39418 = CARTESIAN_POINT ( 'NONE',  ( 4.026613127742574960, -27.09026904771587851, 6.895222827070023541 ) ) ;
#39419 = CARTESIAN_POINT ( 'NONE',  ( 3.262282976461500894, -25.12033811116058502, 7.695279973900954751 ) ) ;
#39420 = CARTESIAN_POINT ( 'NONE',  ( 21.85643539959778892, 8.438975622634238505, -5.206363084432100052 ) ) ;
#39421 = ORIENTED_EDGE ( 'NONE', *, *, #15724, .T. ) ;
#39422 = CARTESIAN_POINT ( 'NONE',  ( -76.45965604259320969, 10.62460191217738448, 8.333162867111299832 ) ) ;
#39423 = CARTESIAN_POINT ( 'NONE',  ( 14.61823925964541004, -4.523600697705748352, 2.500000000000073275 ) ) ;
#39424 = CARTESIAN_POINT ( 'NONE',  ( -78.52362145773746249, 11.36409002021383330, -6.517339437912577971 ) ) ;
#39425 = LINE ( 'NONE', #14712, #12285 ) ;
#39426 = CARTESIAN_POINT ( 'NONE',  ( 37.17733778849484594, -2.564252759210302823, -5.980908861731766279 ) ) ;
#39427 = CARTESIAN_POINT ( 'NONE',  ( 81.14684024915200666, 61.29565758240214279, 1.145133111591830621 ) ) ;
#39428 = CARTESIAN_POINT ( 'NONE',  ( -36.24874870218063450, -26.64985754041175525, 6.800000000000000711 ) ) ;
#39429 = CARTESIAN_POINT ( 'NONE',  ( -62.92837670882106238, 10.37661300689600097, 6.000000000000000000 ) ) ;
#39430 = CARTESIAN_POINT ( 'NONE',  ( -0.07526459735246904259, -26.55379720668586430, 7.660770905198777569 ) ) ;
#39431 = DIRECTION ( 'NONE',  ( -0.000000000000000000, -0.000000000000000000, 1.000000000000000000 ) ) ;
#39432 = VECTOR ( 'NONE', #9987, 1000.000000000000000 ) ;
#39433 = CARTESIAN_POINT ( 'NONE',  ( 4.494099358499767938, -27.46156052226480071, 6.998987538705438993 ) ) ;
#39434 = CARTESIAN_POINT ( 'NONE',  ( 86.62098239308187431, 1.060925892958334060, 5.009353818272591852 ) ) ;
#39435 = CARTESIAN_POINT ( 'NONE',  ( 4.209064950534304295, -31.86482679551882313, 6.868387053540522480 ) ) ;
#39436 = DIRECTION ( 'NONE',  ( -0.000000000000000000, -0.000000000000000000, 1.000000000000000000 ) ) ;
#39437 = CARTESIAN_POINT ( 'NONE',  ( 67.42350544106223253, 58.22289815522609047, 3.997566301760141272 ) ) ;
#39438 = CARTESIAN_POINT ( 'NONE',  ( 35.89360613694101687, -2.027894626843364634, 5.808463346451208764 ) ) ;
#39439 = ORIENTED_EDGE ( 'NONE', *, *, #12924, .T. ) ;
#39440 = ADVANCED_FACE ( 'NONE', ( #9142 ), #24591, .F. ) ;
#39441 = DIRECTION ( 'NONE',  ( 1.000000000000000000, 0.000000000000000000, 0.000000000000000000 ) ) ;
#39442 = CARTESIAN_POINT ( 'NONE',  ( 88.53816506398004549, -1.092544677973264378, 2.020403607635292254 ) ) ;
#39443 = VECTOR ( 'NONE', #24963, 1000.000000000000000 ) ;
#39445 = CARTESIAN_POINT ( 'NONE',  ( 4.877469721015450510, -30.78078569709849788, 6.892063359921935195 ) ) ;
#39444 = CARTESIAN_POINT ( 'NONE',  ( 80.09489858828513320, 64.52483703883090982, -3.563857694938803444 ) ) ;
#39446 = CARTESIAN_POINT ( 'NONE',  ( 4.588767459758324848E-15, -39.37473357531881391, -6.000000000000000000 ) ) ;
#39447 = CARTESIAN_POINT ( 'NONE',  ( 2.290977028701361107, -26.12011756940199447, 7.750000000000000888 ) ) ;
#39448 = ORIENTED_EDGE ( 'NONE', *, *, #32993, .F. ) ;
#39449 = CARTESIAN_POINT ( 'NONE',  ( -0.6716104971371780197, -32.14357770917872870, 6.887547729233689964 ) ) ;
#39450 = VERTEX_POINT ( 'NONE', #11399 ) ;
#39451 = CARTESIAN_POINT ( 'NONE',  ( -1.722611958414476563, -28.83982133125606495, 7.751599049952172749 ) ) ;
#39452 = PRODUCT_DEFINITION_CONTEXT ( 'detailed design', #16583, 'design' ) ;
#39453 = EDGE_CURVE ( 'NONE', #15824, #30074, #5455, .T. ) ;
#39454 = ORIENTED_EDGE ( 'NONE', *, *, #12683, .T. ) ;
#39455 = CARTESIAN_POINT ( 'NONE',  ( 80.90366483818405641, 61.70104970548236167, -2.590854534519439145 ) ) ;
#39456 = CARTESIAN_POINT ( 'NONE',  ( 80.30571993285305155, 63.50758298881806496, 3.683925914261492629 ) ) ;
#39457 = CARTESIAN_POINT ( 'NONE',  ( 23.94017511164331680, 1.184131663965027670, 4.939058140371498595 ) ) ;
#39459 = VERTEX_POINT ( 'NONE', #5868 ) ;
#39458 = CARTESIAN_POINT ( 'NONE',  ( -65.15086340151077593, 36.36839105661640303, 8.980608347108747225 ) ) ;
#39460 = AXIS2_PLACEMENT_3D ( 'NONE', #17713, #5382, #39756 ) ;
#39461 = CARTESIAN_POINT ( 'NONE',  ( 76.54260510937174899, 60.74419326975380073, -3.642592851547832300 ) ) ;
#39462 = MANIFOLD_SOLID_BREP ( 'Slot', #20288 ) ;
#39463 = CARTESIAN_POINT ( 'NONE',  ( -69.95477047248566294, -21.04545455497950712, 5.920697336060226412 ) ) ;
#39464 = PRODUCT_DEFINITION_SHAPE ( 'NONE', 'NONE',  #39396 ) ;
#39466 = CARTESIAN_POINT ( 'NONE',  ( -64.08758708074093136, 38.76906266698303227, -3.000000000000000000 ) ) ;
#39465 = FACE_OUTER_BOUND ( 'NONE', #27009, .T. ) ;
#39467 = CYLINDRICAL_SURFACE ( 'NONE', #34999, 0.09010775117052832739 ) ;
#39468 = LINE ( 'NONE', #24026, #23220 ) ;
#39469 = CARTESIAN_POINT ( 'NONE',  ( 23.69871966413117548, 3.485273507834210527, -3.367185970104320525 ) ) ;
#39470 = VERTEX_POINT ( 'NONE', #14498 ) ;
#39471 = CARTESIAN_POINT ( 'NONE',  ( 5.200390093233090205, -29.62634814563647012, 7.139253571461096293 ) ) ;
#39472 = ORIENTED_EDGE ( 'NONE', *, *, #10415, .F. ) ;
#39473 = CARTESIAN_POINT ( 'NONE',  ( 21.85643539959775694, 1.480681348264278219, 12.33944218828100325 ) ) ;
#39474 = VECTOR ( 'NONE', #12567, 1000.000000000000000 ) ;
#39475 = LINE ( 'NONE', #5315, #4509 ) ;
#39476 = CARTESIAN_POINT ( 'NONE',  ( -2.878675913592191993, -24.55319635012989110, 6.700000000000000178 ) ) ;
#39477 = CARTESIAN_POINT ( 'NONE',  ( 81.38764266124185554, 63.30759111148522322, 3.202775791561840002 ) ) ;
#39478 = CARTESIAN_POINT ( 'NONE',  ( 86.19964454037233281, 1.163379821962233107, 5.771090254565081068 ) ) ;
#39479 = DIRECTION ( 'NONE',  ( -0.000000000000000000, -0.000000000000000000, 1.000000000000000000 ) ) ;
#39480 = ORIENTED_EDGE ( 'NONE', *, *, #37007, .F. ) ;
#39481 = ADVANCED_FACE ( 'NONE', ( #15118 ), #2388, .F. ) ;
#39482 = CARTESIAN_POINT ( 'NONE',  ( -2.508659216904252975, -30.29838823369475520, 7.635761828346577573 ) ) ;
#39483 = CARTESIAN_POINT ( 'NONE',  ( 21.51740365705089530, -3.014515692509022404, -3.492477130908738570 ) ) ;
#39484 = CARTESIAN_POINT ( 'NONE',  ( 25.29565861915397207, 1.734054340005127592, -4.154397323971344314 ) ) ;
#39485 = CARTESIAN_POINT ( 'NONE',  ( -17.07867591359219617, -24.55319635012989110, 6.800000000000000711 ) ) ;
#39486 = CARTESIAN_POINT ( 'NONE',  ( 22.02701140547943837, 0.2674203034431413828, -7.573749491548535495 ) ) ;
#39487 = EDGE_CURVE ( 'NONE', #1373, #31247, #32650, .T. ) ;
#39488 = CARTESIAN_POINT ( 'NONE',  ( 29.67411805608928077, -3.794755287726077064, -4.437710655330253218 ) ) ;
#39489 = ORIENTED_EDGE ( 'NONE', *, *, #7818, .F. ) ;
#39490 = CARTESIAN_POINT ( 'NONE',  ( 34.13650501603236620, -3.129963852335855723, 5.534225220880571783 ) ) ;
#39491 = EDGE_CURVE ( 'NONE', #24999, #26805, #14870, .T. ) ;
#39492 = CIRCLE ( 'NONE', #4043, 3.449999999999999734 ) ;
#39493 = ADVANCED_FACE ( 'NONE', ( #18816 ), #9758, .T. ) ;
#39494 = CARTESIAN_POINT ( 'NONE',  ( -1.145543808814603937, -27.70963634121479657, 6.895222827070022653 ) ) ;
#39495 = VERTEX_POINT ( 'NONE', #304 ) ;
#39496 = ORIENTED_EDGE ( 'NONE', *, *, #14563, .T. ) ;
#39497 = CARTESIAN_POINT ( 'NONE',  ( 37.21233496738312851, -2.743626844932671727, 6.000895157570843352 ) ) ;
#39498 = AXIS2_PLACEMENT_3D ( 'NONE', #32915, #35420, #29424 ) ;
#39499 = DIRECTION ( 'NONE',  ( 0.000000000000000000, 0.000000000000000000, -1.000000000000000000 ) ) ;
#39500 = CARTESIAN_POINT ( 'NONE',  ( 22.09538886637081134, -3.077477272664422614, -3.558916382092313757 ) ) ;
#39501 = CARTESIAN_POINT ( 'NONE',  ( -35.07867591359219972, -26.64985754041175525, 6.800000000000000711 ) ) ;
#39502 = EDGE_LOOP ( 'NONE', ( #9402, #32858, #25084, #7914 ) ) ;
#39503 = CARTESIAN_POINT ( 'NONE',  ( -1.740229416237445648, -30.21191358056005782, 7.678495282201406980 ) ) ;
#39504 = ORIENTED_EDGE ( 'NONE', *, *, #40102, .T. ) ;
#39505 = AXIS2_PLACEMENT_3D ( 'NONE', #36778, #18031, #8561 ) ;
#39506 = ORIENTED_EDGE ( 'NONE', *, *, #32242, .T. ) ;
#39507 = CARTESIAN_POINT ( 'NONE',  ( -77.95330471031414277, 33.71485196875532608, -8.800414904976364028 ) ) ;
#39508 = ADVANCED_FACE ( 'NONE', ( #25411 ), #19230, .F. ) ;
#39509 = CARTESIAN_POINT ( 'NONE',  ( -74.92283640148291113, 18.87330372387140187, 12.49999999999999645 ) ) ;
#39510 = ORIENTED_EDGE ( 'NONE', *, *, #40021, .F. ) ;
#39511 = CARTESIAN_POINT ( 'NONE',  ( 14.73406068751933162, -4.758336531859351126, 2.504581428669218734 ) ) ;
#39512 = ORIENTED_EDGE ( 'NONE', *, *, #25209, .F. ) ;
#39514 = PLANE ( 'NONE',  #8506 ) ;
#39513 = LINE ( 'NONE', #5145, #36355 ) ;
#39515 = ORIENTED_EDGE ( 'NONE', *, *, #8165, .F. ) ;
#39516 = CARTESIAN_POINT ( 'NONE',  ( 23.65346275343500437, 3.385680140419784934, 3.532840291856774062 ) ) ;
#39517 = CARTESIAN_POINT ( 'NONE',  ( 82.17930952126317834, 63.71034004053205280, -2.400449347018691171 ) ) ;
#39518 = CARTESIAN_POINT ( 'NONE',  ( -58.99872204295123623, 28.48507918597066180, 6.834244957304007606 ) ) ;
#39519 = ORIENTED_EDGE ( 'NONE', *, *, #31728, .T. ) ;
#39521 = CARTESIAN_POINT ( 'NONE',  ( 22.14253154251144551, -2.652528785423459823, -3.662275584994673316 ) ) ;
#39520 = DIRECTION ( 'NONE',  ( 1.000000000000000000, 0.000000000000000000, 0.000000000000000000 ) ) ;
#39522 = CARTESIAN_POINT ( 'NONE',  ( -1.797366426793039151, -29.44420554634202247, 6.867199677474203234 ) ) ;
#39523 = CARTESIAN_POINT ( 'NONE',  ( 74.11268706641025972, 61.54722250361106717, 3.856662941142631862 ) ) ;
#39524 = CARTESIAN_POINT ( 'NONE',  ( 24.39390220926783570, 2.657251210456484269, -3.945702052070736432 ) ) ;
#39525 = ORIENTED_EDGE ( 'NONE', *, *, #14221, .F. ) ;
#39526 = LINE ( 'NONE', #17287, #26074 ) ;
#39527 = EDGE_CURVE ( 'NONE', #6853, #33628, #34907, .T. ) ;
#39528 = CARTESIAN_POINT ( 'NONE',  ( 20.26403867649277046, -7.228813795793931796, 2.500000000000000000 ) ) ;
#39529 = CARTESIAN_POINT ( 'NONE',  ( 0.3856705772283747780, -32.81361829944838604, 7.750000000000000888 ) ) ;
#39530 = CARTESIAN_POINT ( 'NONE',  ( -63.25751591902427151, 35.57396452027732892, 6.629192056479301876 ) ) ;
#39531 = DIRECTION ( 'NONE',  ( 0.000000000000000000, 1.000000000000000000, 0.000000000000000000 ) ) ;
#39532 = CARTESIAN_POINT ( 'NONE',  ( 80.93893743487458892, 65.34845912995864126, 2.808566127056212114 ) ) ;
#39533 = SHAPE_REPRESENTATION ( 'Measuring Ruler', ( #30744 ), #40552 ) ;
#39534 = CARTESIAN_POINT ( 'NONE',  ( 85.56690561042726983, 2.244914964738076613, -3.295588454431229497 ) ) ;
#39535 = CARTESIAN_POINT ( 'NONE',  ( 33.89705139301766224, -5.463269898809035574, -0.9834710557593000502 ) ) ;
#39536 = CARTESIAN_POINT ( 'NONE',  ( 1.700390093233090871, -29.56993018339339940, 7.800000000000000711 ) ) ;
#39537 = CARTESIAN_POINT ( 'NONE',  ( 0.6255804977955936597, -26.34427047815355749, 6.866852738645443210 ) ) ;
#39538 = CARTESIAN_POINT ( 'NONE',  ( 0.1191028511967372472, -26.44750632012536329, 6.941203072598479018 ) ) ;
#39539 = AXIS2_PLACEMENT_3D ( 'NONE', #29032, #35624, #29627 ) ;
#39540 = CARTESIAN_POINT ( 'NONE',  ( 35.78807231114511467, -3.222432190208943226, -5.791992240590498220 ) ) ;
#39541 = CARTESIAN_POINT ( 'NONE',  ( 4.703888560603170177, -27.97650715214728123, 7.754798119455333705 ) ) ;
#39542 = CARTESIAN_POINT ( 'NONE',  ( 5.187224694358618216, -29.60529023175765673, 7.783750581861599294 ) ) ;
#39543 = EDGE_CURVE ( 'NONE', #24757, #33685, #25609, .T. ) ;
#39544 = DIRECTION ( 'NONE',  ( 1.000000000000000000, 1.385724075720358314E-16, -0.000000000000000000 ) ) ;
#39545 = EDGE_CURVE ( 'NONE', #13364, #31915, #24098, .T. ) ;
#39546 = CARTESIAN_POINT ( 'NONE',  ( 4.354978660100002230, -31.83382125611363378, 7.781480525794719050 ) ) ;
#39547 = DIRECTION ( 'NONE',  ( 1.000000000000000000, 0.000000000000000000, 0.000000000000000000 ) ) ;
#39548 = EDGE_LOOP ( 'NONE', ( #39147, #5090, #5909, #16810 ) ) ;
#39549 = CARTESIAN_POINT ( 'NONE',  ( 25.69800855216902846, 2.595871837028679963, 3.649274041461021856 ) ) ;
#39550 = CARTESIAN_POINT ( 'NONE',  ( -70.07498307583588826, -0.2501102476861906676, 3.939402591579944435 ) ) ;
#39551 = CARTESIAN_POINT ( 'NONE',  ( 67.18400333313441308, 57.97000644093014188, -3.997693602769901045 ) ) ;
#39552 = CARTESIAN_POINT ( 'NONE',  ( -71.05894754566223526, 0.2170085631127749437, 10.00000000000003197 ) ) ;
#39553 = CARTESIAN_POINT ( 'NONE',  ( -1.749609906766908640, -29.56993018339339940, 6.800000000000000711 ) ) ;
#39554 = ORIENTED_EDGE ( 'NONE', *, *, #29119, .T. ) ;
#39555 = CYLINDRICAL_SURFACE ( 'NONE', #18692, 3.399999999999999911 ) ;
#39556 = CARTESIAN_POINT ( 'NONE',  ( 3.900211856183038783, -32.16237771637295140, 7.748216051605122168 ) ) ;
#39557 = CARTESIAN_POINT ( 'NONE',  ( 85.39527935772777312, 1.303495358572782647, -5.575796090785288150 ) ) ;
#39558 = PLANE ( 'NONE',  #16902 ) ;
#39559 = CARTESIAN_POINT ( 'NONE',  ( -1.477562859369297987, -28.36137111117319520, 6.894806418505348589 ) ) ;
#39560 = CARTESIAN_POINT ( 'NONE',  ( 0.3325276087138285264, -32.79156831072005218, 6.916197352289366052 ) ) ;
#39561 = CARTESIAN_POINT ( 'NONE',  ( 1.265549882940071313, -26.09704752031474229, 7.006908160621415860 ) ) ;
#39562 = ORIENTED_EDGE ( 'NONE', *, *, #20377, .T. ) ;
#39563 = B_SPLINE_CURVE_WITH_KNOTS ( 'NONE', 3,
 ( #28910, #7080, #26027, #10368, #26234, #39162, #13664, #38768, #35507, #7882, #13865, #26628, #35904, #20038, #35310, #7481, #32414, #4209, #13455, #25823, #1131, #10156, #716, #26433, #10564, #23138, #3822, #32217, #35705, #32619, #32014, #4414, #36106, #16339 ),
 .UNSPECIFIED., .F., .F.,
 ( 4, 3, 3, 3, 3, 3, 3, 3, 3, 3, 3, 4 ),
 ( 0.0002070713223507422327, 0.0002134813625843692516, 0.0002436920583247462343, 0.0002744103412181350156, 0.0003056492822488889884, 0.0003371912505268163376, 0.0003686006886010369916, 0.0003994157908200238020, 0.0004294560467902368219, 0.0004589785222107595208, 0.0004885217042653181626, 0.0004917893847005023198 ),
 .UNSPECIFIED. ) ;
#39564 = CARTESIAN_POINT ( 'NONE',  ( 22.19187174190395240, 5.244396285582032746, 3.092647308070439305 ) ) ;
#39565 = CARTESIAN_POINT ( 'NONE',  ( 82.55792188592127445, 63.20960171500892955, -1.000000000000000000 ) ) ;
#39566 = CARTESIAN_POINT ( 'NONE',  ( 81.11292571623972947, 62.23233742369612997, 2.923497156821702525 ) ) ;
#39567 = DIRECTION ( 'NONE',  ( -0.000000000000000000, -1.000000000000000000, -0.000000000000000000 ) ) ;
#39568 = ORIENTED_EDGE ( 'NONE', *, *, #737, .T. ) ;
#39569 = CARTESIAN_POINT ( 'NONE',  ( 78.06740453511717703, 61.95427634543510464, -3.748203062644121619 ) ) ;
#39571 = FACE_OUTER_BOUND ( 'NONE', #16098, .T. ) ;
#39570 = CARTESIAN_POINT ( 'NONE',  ( 22.59969544733755953, 0.2728855050143408900, 6.520465242868895395 ) ) ;
#39572 = CARTESIAN_POINT ( 'NONE',  ( 81.38674634791389906, 61.68395714348710612, -2.028924249969755955 ) ) ;
#39573 = CARTESIAN_POINT ( 'NONE',  ( 79.88607388276625443, 61.09294650314146224, 2.551779361026688342 ) ) ;
#39574 = EDGE_LOOP ( 'NONE', ( #1657, #30883, #36634, #24396 ) ) ;
#39575 = AXIS2_PLACEMENT_3D ( 'NONE', #1499, #4981, #32797 ) ;
#39576 = CARTESIAN_POINT ( 'NONE',  ( -0.9124018737164114601, -27.39430309170973388, 7.756377446753158544 ) ) ;
#39577 = EDGE_LOOP ( 'NONE', ( #16138, #18086 ) ) ;
#39578 = CARTESIAN_POINT ( 'NONE',  ( 81.27149311957296618, 65.88890312491021461, 1.680016503630072489 ) ) ;
#39580 = CARTESIAN_POINT ( 'NONE',  ( 87.04213330793392345, 0.5878691963682337596, 6.000000000000000000 ) ) ;
#39579 = CARTESIAN_POINT ( 'NONE',  ( 4.333310421813720836, -31.87597283208960874, 6.867280401193706751 ) ) ;
#39581 = CARTESIAN_POINT ( 'NONE',  ( 29.75545004716739683, -3.157578436209982353, 4.923334784591472335 ) ) ;
#39582 = DIRECTION ( 'NONE',  ( -0.000000000000000000, 1.000000000000000000, -0.000000000000000000 ) ) ;
#39583 = CARTESIAN_POINT ( 'NONE',  ( 4.331203346590854153, -31.73491918113357357, 7.257242401810562349 ) ) ;
#39584 = VERTEX_POINT ( 'NONE', #106 ) ;
#39585 = CARTESIAN_POINT ( 'NONE',  ( -81.82390275669976631, -5.600668035901278152, 0.2449979024077967027 ) ) ;
#39586 = CARTESIAN_POINT ( 'NONE',  ( 21.78199703343759452, 0.2105167186554868786, -8.406929788681917870 ) ) ;
#39587 = EDGE_CURVE ( 'NONE', #29224, #23963, #14903, .T. ) ;
#39588 = CARTESIAN_POINT ( 'NONE',  ( 0.7753597313414962722, -32.84905728735835595, 7.505001789837629111 ) ) ;
#39589 = DIRECTION ( 'NONE',  ( -3.491481338843133750E-15, 1.000000000000000000, -0.000000000000000000 ) ) ;
#39590 = CARTESIAN_POINT ( 'NONE',  ( 5.156371316636622737, -29.01658238726313854, 6.875671892026062437 ) ) ;
#39591 = ADVANCED_FACE ( 'NONE', ( #3009 ), #40636, .F. ) ;
#39592 = DIRECTION ( 'NONE',  ( 0.000000000000000000, 1.000000000000000000, 0.000000000000000000 ) ) ;
#39593 = CARTESIAN_POINT ( 'NONE',  ( 36.71858516611970202, -3.456771977683057884, -5.861348970100675793 ) ) ;
#39594 = CARTESIAN_POINT ( 'NONE',  ( 3.343728876470205336, -32.65988526930982516, 7.754798119455333705 ) ) ;
#39595 = DIRECTION ( 'NONE',  ( -0.000000000000000000, -0.000000000000000000, 1.000000000000000000 ) ) ;
#39596 = CARTESIAN_POINT ( 'NONE',  ( -80.92837670882107659, 2.429809908903242555, -12.50000000000000000 ) ) ;
#39597 = CARTESIAN_POINT ( 'NONE',  ( -71.31807670174137570, -48.56883691054113683, 5.988105119137681065 ) ) ;
#39598 = DIRECTION ( 'NONE',  ( 0.6427876096865284827, 0.7660444431189872283, 0.000000000000000000 ) ) ;
#39599 = CARTESIAN_POINT ( 'NONE',  ( 4.630071603208546271, -27.84454145904519251, 7.661510568013100375 ) ) ;
#39600 = EDGE_CURVE ( 'NONE', #9594, #38454, #22167, .T. ) ;
#39601 = CARTESIAN_POINT ( 'NONE',  ( 23.16133184106407583, 1.224392961250923229, -5.385929051048157667 ) ) ;
#39602 = ADVANCED_FACE ( 'NONE', ( #31390 ), #31795, .F. ) ;
#39603 = EDGE_LOOP ( 'NONE', ( #3280, #4687, #38749, #7996, #8318 ) ) ;
#39604 = CARTESIAN_POINT ( 'NONE',  ( 66.43385761674670675, 57.75742247880102553, 4.000000000000003553 ) ) ;
#39605 = CARTESIAN_POINT ( 'NONE',  ( 71.32664523234116416, 58.52704510057537135, -3.775670717450666736 ) ) ;
#39606 = VECTOR ( 'NONE', #17320, 1000.000000000000114 ) ;
#39607 = ORIENTED_EDGE ( 'NONE', *, *, #27615, .F. ) ;
#39608 = LINE ( 'NONE', #27257, #15373 ) ;
#39609 = CARTESIAN_POINT ( 'NONE',  ( -6.248748702180631831, -26.64985754041175525, 6.700000000000000178 ) ) ;
#39610 = VERTEX_POINT ( 'NONE', #10148 ) ;
#39611 = CARTESIAN_POINT ( 'NONE',  ( -0.8650427792287253004, -27.18905761710760416, 7.006908160621412307 ) ) ;
#39612 = ITEM_DEFINED_TRANSFORMATION ( 'NONE', 'NONE', #17562,  #30744 ) ;
#39613 = CARTESIAN_POINT ( 'NONE',  ( -4.890026461918809630, -25.50263309590217276, 2.500000000000000000 ) ) ;
#39614 = ORIENTED_EDGE ( 'NONE', *, *, #39527, .T. ) ;
#39615 = DIRECTION ( 'NONE',  ( -0.000000000000000000, -0.000000000000000000, 1.000000000000000000 ) ) ;
#39616 =( LENGTH_UNIT ( ) NAMED_UNIT ( * ) SI_UNIT ( .MILLI., .METRE. ) );
#39617 = CARTESIAN_POINT ( 'NONE',  ( 23.16657086568211099, -3.117828266824798966, 3.711575906808437075 ) ) ;
#39618 = ORIENTED_EDGE ( 'NONE', *, *, #36400, .T. ) ;
#39619 = ORIENTED_EDGE ( 'NONE', *, *, #38506, .F. ) ;
#39620 = CARTESIAN_POINT ( 'NONE',  ( 78.80159527267854003, 65.27891740916034280, -2.934133054905260884 ) ) ;
#39621 = B_SPLINE_CURVE_WITH_KNOTS ( 'NONE', 3,
 ( #11917, #9042, #25323, #24492, #12543, #12339, #8833, #24703, #12746, #28185 ),
 .UNSPECIFIED., .F., .F.,
 ( 4, 3, 3, 4 ),
 ( 8.673617379884035472E-19, 3.025570593003056093E-05, 6.051145698344016094E-05, 6.468151674593633721E-05 ),
 .UNSPECIFIED. ) ;
#39622 = CARTESIAN_POINT ( 'NONE',  ( 16.55058197964011768, 7.675960740364504709, -3.484773916741207067 ) ) ;
#39623 = CARTESIAN_POINT ( 'NONE',  ( 78.91303721271684424, 66.16570306020605585, -1.285939662725172461 ) ) ;
#39624 = CARTESIAN_POINT ( 'NONE',  ( 78.99843287308405593, 65.13824187233507246, 3.101774481621351498 ) ) ;
#39625 = DIRECTION ( 'NONE',  ( 0.000000000000000000, 1.000000000000000000, 0.000000000000000000 ) ) ;
#39626 = CARTESIAN_POINT ( 'NONE',  ( 3.941824067710134383, -27.01335656366605420, 6.874555630061442102 ) ) ;
#39627 = DIRECTION ( 'NONE',  ( 0.000000000000000000, 0.000000000000000000, 1.000000000000000000 ) ) ;
#39628 = CARTESIAN_POINT ( 'NONE',  ( 21.85643539959776760, -12.33099359671888884, 6.023794913588264244 ) ) ;
#39629 = ORIENTED_EDGE ( 'NONE', *, *, #6666, .F. ) ;
#39630 = CARTESIAN_POINT ( 'NONE',  ( -80.92837670882107659, 2.429809908903242555, 15.50000000000000000 ) ) ;
#39631 = VECTOR ( 'NONE', #21293, 1000.000000000000000 ) ;
#39632 = CARTESIAN_POINT ( 'NONE',  ( 14.78265019125518975, -5.167055302568825503, 2.499999999999999556 ) ) ;
#39633 = B_SPLINE_CURVE_WITH_KNOTS ( 'NONE', 3,
 ( #16541, #1333, #524, #4611 ),
 .UNSPECIFIED., .F., .F.,
 ( 4, 4 ),
 ( 0.000000000000000000, 6.391136169994592770E-06 ),
 .UNSPECIFIED. ) ;
#39634 = CARTESIAN_POINT ( 'NONE',  ( -80.78529318222091149, 10.51041525961532663, -4.938515984036527584 ) ) ;
#39635 = CARTESIAN_POINT ( 'NONE',  ( 2.341155903240350167, -26.23085468064335046, 6.892063359921932530 ) ) ;
#39636 = CARTESIAN_POINT ( 'NONE',  ( 30.67349724481533002, -3.593355625737403525, 4.777428303402127874 ) ) ;
#39637 = FACE_OUTER_BOUND ( 'NONE', #12695, .T. ) ;
#39638 = DIRECTION ( 'NONE',  ( 1.000000000000000000, 0.000000000000000000, 0.000000000000000000 ) ) ;
#39639 = CARTESIAN_POINT ( 'NONE',  ( 0.6494831848250305351, -26.23141567014731734, 6.880828092187096345 ) ) ;
#39640 = ADVANCED_FACE ( 'NONE', ( #515 ), #22739, .F. ) ;
#39641 = EDGE_CURVE ( 'NONE', #32059, #30749, #15930, .T. ) ;
#39642 = VECTOR ( 'NONE', #21286, 1000.000000000000000 ) ;
#39643 = CARTESIAN_POINT ( 'NONE',  ( -64.08758708074094557, 35.89352542652032696, 3.939681497839040425 ) ) ;
#39644 = DIRECTION ( 'NONE',  ( 0.000000000000000000, 0.000000000000000000, 1.000000000000000000 ) ) ;
#39645 = ADVANCED_FACE ( 'NONE', ( #9341 ), #12842, .T. ) ;
#39646 = CARTESIAN_POINT ( 'NONE',  ( 5.097523595859303924, -28.69978428133380888, 7.501983001166817822 ) ) ;
#39647 = VERTEX_POINT ( 'NONE', #6269 ) ;
#39648 = CARTESIAN_POINT ( 'NONE',  ( 67.79930094788625183, 58.10454462619039617, 3.992148460412408895 ) ) ;
#39649 = CARTESIAN_POINT ( 'NONE',  ( 33.45622785515271147, -3.169918179184307849, 5.428051517361659251 ) ) ;
#39650 = B_SPLINE_CURVE_WITH_KNOTS ( 'NONE', 3,
 ( #38735, #23111, #20008, #32588, #4385, #16910, #39753, #36872, #8855, #36463, #12149, #30498, #20601, #21030, #30713, #34014, #2724, #30096, #8653, #8238, #20808, #11941, #14618, #18120, #27801, #5788, #11530, #27394, #18326, #36664, #33603 ),
 .UNSPECIFIED., .F., .F.,
 ( 4, 3, 3, 3, 3, 3, 3, 3, 3, 3, 4 ),
 ( 8.182674270850422113E-18, 3.077658087705610260E-05, 6.152638666999237784E-05, 9.267501192706366906E-05, 0.0001241882240135212313, 0.0001556618703051610537, 0.0001866161554452267488, 0.0002167966385861010473, 0.0002463805737537807963, 0.0002758761370306577485, 0.0002847094172290174090 ),
 .UNSPECIFIED. ) ;
#39651 = CARTESIAN_POINT ( 'NONE',  ( 0.7302373594189235373, -26.30393590818857064, 7.386948897581449458 ) ) ;
#39652 = CARTESIAN_POINT ( 'NONE',  ( 88.61980888719223515, -1.376070350315937940, 2.940712392697649058 ) ) ;
#39653 = CARTESIAN_POINT ( 'NONE',  ( 4.862263076544310003, -30.81999235699081652, 6.866852738645444099 ) ) ;
#39654 =( BOUNDED_CURVE ( )  B_SPLINE_CURVE ( 3, ( #15713, #28684, #9526, #494 ),
 .UNSPECIFIED., .F., .T. ) 
 B_SPLINE_CURVE_WITH_KNOTS ( ( 4, 4 ),
 ( 4.708531083176467291, 4.895802057644188743 ),
 .UNSPECIFIED. ) 
 CURVE ( )  GEOMETRIC_REPRESENTATION_ITEM ( )  RATIONAL_B_SPLINE_CURVE ( ( 1.000000000000000000, 0.9970795998553221295, 0.9970795998553221295, 1.000000000000000000 ) ) 
 REPRESENTATION_ITEM ( '' )  );
#39655 = DIRECTION ( 'NONE',  ( -0.000000000000000000, -0.000000000000000000, 1.000000000000000000 ) ) ;
#39656 = CIRCLE ( 'NONE', #9421, 98.38357402481355507 ) ;
#39657 = CARTESIAN_POINT ( 'NONE',  ( -59.35030935981329492, 27.06751177275602416, 5.142387704658994529 ) ) ;
#39658 = CARTESIAN_POINT ( 'NONE',  ( -0.6132364880641560934, -32.19616932755274519, 6.865554069792297653 ) ) ;
#39659 = EDGE_LOOP ( 'NONE', ( #33276, #26470, #22631, #25007 ) ) ;
#39660 = CARTESIAN_POINT ( 'NONE',  ( -71.46462112523092003, -21.62705418684702252, 3.975988782274377797 ) ) ;
#39661 = VERTEX_POINT ( 'NONE', #31595 ) ;
#39662 = CARTESIAN_POINT ( 'NONE',  ( 80.99919828920802445, 61.56308015027071434, -2.277920705665343437 ) ) ;
#39663 = DIRECTION ( 'NONE',  ( -0.5751513419797977811, 0.4826092789263575211, 0.6605219282605377940 ) ) ;
#39664 = CARTESIAN_POINT ( 'NONE',  ( 80.99395165659490203, 61.72087377645424056, 2.545842637937928643 ) ) ;
#39665 = CARTESIAN_POINT ( 'NONE',  ( 22.81843309643631201, 0.8035065468961524182, 5.971597756558487013 ) ) ;
#39667 = EDGE_LOOP ( 'NONE', ( #25507, #31059, #8110, #30852 ) ) ;
#39666 = CARTESIAN_POINT ( 'NONE',  ( -66.83699642652008777, 37.05199716444892744, 9.800414904976364028 ) ) ;
#39668 = CARTESIAN_POINT ( 'NONE',  ( 73.85752424338471656, 60.59307193704751882, -3.935025356177997757 ) ) ;
#39669 = AXIS2_PLACEMENT_3D ( 'NONE', #23201, #35772, #17204 ) ;
#39670 = MANIFOLD_SOLID_BREP ( 'Fillet13', #3249 ) ;
#39671 = CARTESIAN_POINT ( 'NONE',  ( -70.66674249470580094, -21.75688355017156184, 5.995522264747396690 ) ) ;
#39673 = PLANE ( 'NONE',  #30873 ) ;
#39672 = DIRECTION ( 'NONE',  ( 0.000000000000000000, 0.000000000000000000, -1.000000000000000000 ) ) ;
#39674 = CARTESIAN_POINT ( 'NONE',  ( -0.3487487021806359722, -26.64985754041175525, 6.700000000000000178 ) ) ;
#39675 = LINE ( 'NONE', #29809, #32713 ) ;
#39676 = CARTESIAN_POINT ( 'NONE',  ( 4.662641849846992592, -31.23878144412272206, 7.691066658568944447 ) ) ;
#39677 = CARTESIAN_POINT ( 'NONE',  ( 22.64349050896827009, 4.515835945530393580, -3.146491140164486833 ) ) ;
#39678 = ORIENTED_EDGE ( 'NONE', *, *, #3107, .T. ) ;
#39679 = DIRECTION ( 'NONE',  ( 0.000000000000000000, 1.000000000000000000, 0.000000000000000000 ) ) ;
#39680 = CARTESIAN_POINT ( 'NONE',  ( 21.85643539959777115, -1.513967970512005268, 12.69801924519992120 ) ) ;
#39681 = CARTESIAN_POINT ( 'NONE',  ( -0.9620374312546590145, -31.84181919407372163, 7.730015791551947402 ) ) ;
#39682 = ORIENTED_EDGE ( 'NONE', *, *, #32881, .T. ) ;
#39683 = CARTESIAN_POINT ( 'NONE',  ( 4.983270326624491098, -28.35638137736280484, 7.640616322432102869 ) ) ;
#39684 = CARTESIAN_POINT ( 'NONE',  ( 79.01071357413493956, 66.12284964548014443, 1.692865493182734271 ) ) ;
#39685 = CARTESIAN_POINT ( 'NONE',  ( 85.01740037914012760, 2.610285099004062470, -3.580537606963684283 ) ) ;
#39686 = LINE ( 'NONE', #36609, #25973 ) ;
#39687 = ORIENTED_EDGE ( 'NONE', *, *, #16571, .F. ) ;
#39688 = DIRECTION ( 'NONE',  ( -1.000000000000000000, 0.000000000000000000, 0.000000000000000000 ) ) ;
#39689 = CARTESIAN_POINT ( 'NONE',  ( 5.200252094213874798, -29.60101030711846448, 6.894806418505347700 ) ) ;
#39690 = CARTESIAN_POINT ( 'NONE',  ( 21.50588977098013999, -2.807818977413083950, -3.559126483975300292 ) ) ;
#39691 = ADVANCED_FACE ( 'NONE', ( #10748 ), #3215, .T. ) ;
#39692 = CARTESIAN_POINT ( 'NONE',  ( 22.91933720673384656, 2.648293172188526334, -3.783514896012181161 ) ) ;
#39693 = PLANE ( 'NONE',  #29290 ) ;
#39694 = CARTESIAN_POINT ( 'NONE',  ( 25.13440357308012807, 0.9923446184508544210, -4.613365629549119440 ) ) ;
#39695 = DIRECTION ( 'NONE',  ( 0.000000000000000000, 0.000000000000000000, 1.000000000000000000 ) ) ;
#39696 = EDGE_LOOP ( 'NONE', ( #26430, #3964, #7354, #239 ) ) ;
#39697 = CARTESIAN_POINT ( 'NONE',  ( 35.78603942060401977, -3.161145183569410211, 5.791674958855998590 ) ) ;
#39698 = AXIS2_PLACEMENT_3D ( 'NONE', #6061, #18595, #31181 ) ;
#39699 = VECTOR ( 'NONE', #23088, 1000.000000000000227 ) ;
#39700 = CARTESIAN_POINT ( 'NONE',  ( 5.028764603308605530, -28.48812247857538438, 7.754798119455333705 ) ) ;
#39701 = VERTEX_POINT ( 'NONE', #35898 ) ;
#39702 = ORIENTED_EDGE ( 'NONE', *, *, #35205, .F. ) ;
#39704 = CARTESIAN_POINT ( 'NONE',  ( 36.87235869322262261, -2.085126334481405497, 5.863268595800801286 ) ) ;
#39703 = CARTESIAN_POINT ( 'NONE',  ( 81.29933375999361544, 61.48586111389077757, -1.777114115212629075 ) ) ;
#39705 = DIRECTION ( 'NONE',  ( -1.000000000000000000, 0.000000000000000000, 0.000000000000000000 ) ) ;
#39706 = DIRECTION ( 'NONE',  ( 0.000000000000000000, 1.000000000000000000, 0.000000000000000000 ) ) ;
#39707 = DIRECTION ( 'NONE',  ( -0.000000000000000000, -0.000000000000000000, -1.000000000000000000 ) ) ;
#39708 = ORIENTED_EDGE ( 'NONE', *, *, #39866, .T. ) ;
#39709 = DIRECTION ( 'NONE',  ( 0.000000000000000000, 0.000000000000000000, 1.000000000000000000 ) ) ;
#39710 = AXIS2_PLACEMENT_3D ( 'NONE', #13753, #31535, #13943 ) ;
#39711 = VERTEX_POINT ( 'NONE', #17323 ) ;
#39713 = ORIENTED_EDGE ( 'NONE', *, *, #13339, .F. ) ;
#39712 = ORIENTED_EDGE ( 'NONE', *, *, #21963, .T. ) ;
#39714 = CARTESIAN_POINT ( 'NONE',  ( 0.01787935223071997204, -32.52445247686870289, 7.643333865083955736 ) ) ;
#39715 = AXIS2_PLACEMENT_3D ( 'NONE', #27778, #22031, #5968 ) ;
#39716 = CARTESIAN_POINT ( 'NONE',  ( 81.14230761098953337, 61.33243076862672183, -1.577285172236833288 ) ) ;
#39717 = CARTESIAN_POINT ( 'NONE',  ( -58.20517375958247897, 28.49598760833108813, -5.016376253474278180 ) ) ;
#39718 = ORIENTED_EDGE ( 'NONE', *, *, #22009, .T. ) ;
#39719 = EDGE_CURVE ( 'NONE', #34893, #15830, #12260, .T. ) ;
#39721 = DIRECTION ( 'NONE',  ( 0.000000000000000000, 0.000000000000000000, 1.000000000000000000 ) ) ;
#39720 = CARTESIAN_POINT ( 'NONE',  ( 4.813436497423070115, -27.97025956726023566, 7.011627023500182077 ) ) ;
#39722 = VERTEX_POINT ( 'NONE', #1717 ) ;
#39723 = CARTESIAN_POINT ( 'NONE',  ( 23.87861567317384015, 3.102426543664170033, 3.710302979149028957 ) ) ;
#39724 = CARTESIAN_POINT ( 'NONE',  ( 78.68944183191024422, 66.05792399308624852, -1.032522165606416298 ) ) ;
#39725 = DIRECTION ( 'NONE',  ( 0.000000000000000000, 1.000000000000000000, 0.000000000000000000 ) ) ;
#39726 = EDGE_LOOP ( 'NONE', ( #34106, #3741 ) ) ;
#39728 = CARTESIAN_POINT ( 'NONE',  ( 21.85643539959776760, -15.11427361947482062, -2.500000000000000000 ) ) ;
#39727 = CARTESIAN_POINT ( 'NONE',  ( 0.07058059489397008890, -26.58600545297078099, 7.782034975670478083 ) ) ;
#39729 = LINE ( 'NONE', #11512, #36936 ) ;
#39730 = CARTESIAN_POINT ( 'NONE',  ( 73.92749824250802249, 61.95374747488791201, 3.708893976703420137 ) ) ;
#39731 = VERTEX_POINT ( 'NONE', #4201 ) ;
#39732 = CARTESIAN_POINT ( 'NONE',  ( 22.74486227573763841, 2.267316151577437822, -4.906501245702026281 ) ) ;
#39733 = ORIENTED_EDGE ( 'NONE', *, *, #38674, .F. ) ;
#39734 = EDGE_CURVE ( 'NONE', #35457, #24696, #7074, .T. ) ;
#39735 = VECTOR ( 'NONE', #7262, 1000.000000000000000 ) ;
#39736 = CARTESIAN_POINT ( 'NONE',  ( -55.39244940828794483, 31.07786128219253996, -1.730094348643104185 ) ) ;
#39737 = VECTOR ( 'NONE', #17146, 1000.000000000000000 ) ;
#39738 = CYLINDRICAL_SURFACE ( 'NONE', #16391, 0.1000000000000028644 ) ;
#39739 = CARTESIAN_POINT ( 'NONE',  ( -1.260542631132519853, -27.89873549449913170, 7.670860738520326905 ) ) ;
#39740 = CARTESIAN_POINT ( 'NONE',  ( 6.149982165465896600, -31.13182306662183052, 7.695279973900954751 ) ) ;
#39742 = CARTESIAN_POINT ( 'NONE',  ( 81.87453109492318504, 63.55405699985837487, 2.808566127056211670 ) ) ;
#39741 = APPLICATION_CONTEXT ( 'automotive_design' ) ;
#39743 = CARTESIAN_POINT ( 'NONE',  ( 86.06238440510853138, 1.688369665709827272, 4.446988894268222303 ) ) ;
#39744 = CARTESIAN_POINT ( 'NONE',  ( -30.24874870218063450, -26.64985754041175525, 6.700000000000000178 ) ) ;
#39745 = LINE ( 'NONE', #2298, #11539 ) ;
#39746 = AXIS2_PLACEMENT_3D ( 'NONE', #25795, #279, #25391 ) ;
#39747 = CARTESIAN_POINT ( 'NONE',  ( -0.9271071152667473836, -27.41209366881661325, 7.692469944509192636 ) ) ;
#39748 = DIRECTION ( 'NONE',  ( 1.000000000000000000, 8.959828616340678715E-16, 0.000000000000000000 ) ) ;
#39749 = LINE ( 'NONE', #6195, #14402 ) ;
#39750 = EDGE_CURVE ( 'NONE', #17262, #23554, #22053, .T. ) ;
#39751 = CARTESIAN_POINT ( 'NONE',  ( 20.53310393597628192, 3.934805220908249801, -3.411085482841109240 ) ) ;
#39752 = CARTESIAN_POINT ( 'NONE',  ( -0.5145088012743496142, -26.98099630600513876, 7.257242401810563237 ) ) ;
#39753 = CARTESIAN_POINT ( 'NONE',  ( 4.688487803309406843, -31.39236593672921316, 6.865554069792297653 ) ) ;
#39754 = CARTESIAN_POINT ( 'NONE',  ( -27.07867591359219972, -26.64985754041175525, 6.700000000000000178 ) ) ;
#39755 = PLANE ( 'NONE',  #14369 ) ;
#39756 = DIRECTION ( 'NONE',  ( 1.000000000000000000, 0.000000000000000000, 0.000000000000000000 ) ) ;
#39757 = VERTEX_POINT ( 'NONE', #1125 ) ;
#39758 = CARTESIAN_POINT ( 'NONE',  ( 34.14209189958793900, -3.845064354223240333, 5.237926034909554218 ) ) ;
#39759 = CARTESIAN_POINT ( 'NONE',  ( 1.215732341648462000, -26.10364848027380447, 7.751599049952174525 ) ) ;
#39760 = CARTESIAN_POINT ( 'NONE',  ( 66.71755507405909214, 57.88420400998732163, -3.999756211082241109 ) ) ;
#39761 = CARTESIAN_POINT ( 'NONE',  ( 4.301450302647315205, -31.91148321001355370, 7.754798119455333705 ) ) ;
#39762 = ADVANCED_FACE ( 'NONE', ( #19835 ), #23131, .F. ) ;
#39763 = DIRECTION ( 'NONE',  ( 1.000000000000000000, 0.000000000000000000, 0.000000000000000000 ) ) ;
#39764 = AXIS2_PLACEMENT_3D ( 'NONE', #23308, #32190, #29679 ) ;
#39765 = ORIENTED_EDGE ( 'NONE', *, *, #31350, .F. ) ;
#39766 = AXIS2_PLACEMENT_3D ( 'NONE', #13735, #4478, #23399 ) ;
#39767 = FACE_OUTER_BOUND ( 'NONE', #7205, .T. ) ;
#39768 = CARTESIAN_POINT ( 'NONE',  ( 86.06519988977099445, 0.1302210779029090437, -5.995352467121073836 ) ) ;
#39769 = CARTESIAN_POINT ( 'NONE',  ( 75.43647511836071828, 63.77933554463422183, 2.884169428409014913 ) ) ;
#39770 = CARTESIAN_POINT ( 'NONE',  ( 1.062037487868057184, -32.90946697031814949, 6.894806418505346812 ) ) ;
#39771 = VECTOR ( 'NONE', #25393, 1000.000000000000000 ) ;
#39772 = CARTESIAN_POINT ( 'NONE',  ( -8.978675913592192970, -24.55319635012989110, 6.700000000000000178 ) ) ;
#39773 = CARTESIAN_POINT ( 'NONE',  ( -1.699406134149164416, -29.53190947434445235, 7.784295182778427247 ) ) ;
#39774 = ORIENTED_EDGE ( 'NONE', *, *, #14447, .T. ) ;
#39775 = CARTESIAN_POINT ( 'NONE',  ( 22.61643043036420053, 4.612325523533245430, 3.058534595953864343 ) ) ;
#39776 = CARTESIAN_POINT ( 'NONE',  ( 81.16957891225081312, 61.30398062001320625, -1.002944004955704127 ) ) ;
#39777 = VECTOR ( 'NONE', #32258, 1000.000000000000000 ) ;
#39778 = LINE ( 'NONE', #24331, #13010 ) ;
#39779 = CARTESIAN_POINT ( 'NONE',  ( 80.36137575039691683, 63.90592395025429795, 3.640670270625567362 ) ) ;
#39780 = CARTESIAN_POINT ( 'NONE',  ( 24.75839165839662925, 3.019244830385916956, -3.350409272483306111 ) ) ;
#39781 = ORIENTED_EDGE ( 'NONE', *, *, #6719, .F. ) ;
#39782 = CARTESIAN_POINT ( 'NONE',  ( 78.75717319332352417, 60.46956391627943361, -2.498359881428382057 ) ) ;
#39783 =( BOUNDED_CURVE ( )  B_SPLINE_CURVE ( 3, ( #19406, #6852, #16308, #685 ),
 .UNSPECIFIED., .F., .T. ) 
 B_SPLINE_CURVE_WITH_KNOTS ( ( 4, 4 ),
 ( 4.708531083176469068, 4.895802057644189631 ),
 .UNSPECIFIED. ) 
 CURVE ( )  GEOMETRIC_REPRESENTATION_ITEM ( )  RATIONAL_B_SPLINE_CURVE ( ( 1.000000000000000000, 0.9970795998553221295, 0.9970795998553221295, 1.000000000000000000 ) ) 
 REPRESENTATION_ITEM ( '' )  );
#39785 = CARTESIAN_POINT ( 'NONE',  ( 14.71768660209398583, -5.068519077135388073, -2.499999999999999556 ) ) ;
#39784 = CARTESIAN_POINT ( 'NONE',  ( 21.73396269091076860, 0.2160964541248809045, 9.105401517513902476 ) ) ;
#39786 = EDGE_CURVE ( 'NONE', #39282, #5089, #7013, .T. ) ;
#39787 = EDGE_CURVE ( 'NONE', #6937, #28759, #4013, .T. ) ;
#39788 = CARTESIAN_POINT ( 'NONE',  ( 81.15394892944708261, 63.54712375395006774, -3.396356880839461301 ) ) ;
#39789 = CARTESIAN_POINT ( 'NONE',  ( 79.97179536941432332, 60.87748285318664898, 2.061059937946318144 ) ) ;
#39790 = ORIENTED_EDGE ( 'NONE', *, *, #36997, .T. ) ;
#39791 = ADVANCED_FACE ( 'NONE', ( #39156 ), #20030, .T. ) ;
#39792 = DIRECTION ( 'NONE',  ( 0.000000000000000000, 0.7126435865141285131, 0.7015262779114406211 ) ) ;
#39793 = ORIENTED_EDGE ( 'NONE', *, *, #9581, .T. ) ;
#39794 = CARTESIAN_POINT ( 'NONE',  ( 82.36730661685074040, 64.56044919582443242, 1.633153239554254732 ) ) ;
#39796 = CARTESIAN_POINT ( 'NONE',  ( -63.08758708074093136, -21.25669541281728669, 4.000000000000000000 ) ) ;
#39795 = DIRECTION ( 'NONE',  ( 0.000000000000000000, 0.000000000000000000, 1.000000000000000000 ) ) ;
#39797 = CARTESIAN_POINT ( 'NONE',  ( 29.86640044794213011, -3.433240980530400499, 4.572246828724481738 ) ) ;
#39798 = DIRECTION ( 'NONE',  ( -1.000000000000000000, 0.000000000000000000, 0.000000000000000000 ) ) ;
#39799 = CARTESIAN_POINT ( 'NONE',  ( 5.042305363714541855, -28.94414881188822619, 7.695279973900954751 ) ) ;
#39800 = EDGE_LOOP ( 'NONE', ( #28445, #21566, #7010, #27424 ) ) ;
#39801 = CARTESIAN_POINT ( 'NONE',  ( 1.595260788587017586, -33.06836594711004551, 6.863784140767622333 ) ) ;
#39802 = CARTESIAN_POINT ( 'NONE',  ( 21.97057884596240740, 0.2201703367346467544, -7.735646635481312927 ) ) ;
#39803 = DIRECTION ( 'NONE',  ( -0.000000000000000000, -0.000000000000000000, 1.000000000000000000 ) ) ;
#39804 = CARTESIAN_POINT ( 'NONE',  ( -63.70768058868311812, 44.39675795731059793, 1.000000000000000000 ) ) ;
#39805 = CARTESIAN_POINT ( 'NONE',  ( 3.973866779147308570, -26.90885826429679284, 6.894806418505347700 ) ) ;
#39806 = VECTOR ( 'NONE', #36992, 1000.000000000000000 ) ;
#39807 = CARTESIAN_POINT ( 'NONE',  ( 5.174907696227332821, -29.14835287555633769, 6.980586498568971621 ) ) ;
#39808 = DIRECTION ( 'NONE',  ( 0.000000000000000000, 0.000000000000000000, -1.000000000000000000 ) ) ;
#39809 = CARTESIAN_POINT ( 'NONE',  ( 32.06722284780977361, 0.2495805760236646520, -4.732413161253986367 ) ) ;
#39810 = CARTESIAN_POINT ( 'NONE',  ( 3.378579686077430644, -32.62731885087992367, 7.782861076432731728 ) ) ;
#39811 = CARTESIAN_POINT ( 'NONE',  ( 1.135223716940237937, -32.92263077448382091, 7.652160403243382980 ) ) ;
#39812 = CARTESIAN_POINT ( 'NONE',  ( 5.045182535701832727, -28.95967786423770818, 7.643333865083955736 ) ) ;
#39813 = ADVANCED_FACE ( 'NONE', ( #19638 ), #18811, .T. ) ;
#39814 = CARTESIAN_POINT ( 'NONE',  ( -71.41359911753804113, -48.53977970579884982, 5.981042891625516056 ) ) ;
#39815 = DIRECTION ( 'NONE',  ( -0.000000000000000000, -1.000000000000000000, -0.000000000000000000 ) ) ;
#39816 = CARTESIAN_POINT ( 'NONE',  ( 5.100005351453509306, -29.62113694480887105, 6.892063359921934307 ) ) ;
#39817 = AXIS2_PLACEMENT_3D ( 'NONE', #14661, #2143, #30541 ) ;
#39818 = CARTESIAN_POINT ( 'NONE',  ( 4.878343045835490166, -30.77848925561357873, 6.894806418505348589 ) ) ;
#39819 = CARTESIAN_POINT ( 'NONE',  ( -1.583891440918162585, -30.77968007673214146, 7.635761828346579350 ) ) ;
#39820 = CARTESIAN_POINT ( 'NONE',  ( 23.04890016929587659, 1.973574480669345155, -4.925800778672301483 ) ) ;
#39821 = CARTESIAN_POINT ( 'NONE',  ( -70.44203116010082510, -48.53935907511377934, 5.980943839742335122 ) ) ;
#39822 = CARTESIAN_POINT ( 'NONE',  ( 66.58744840590414071, 57.78483400379950297, 3.999444518112384106 ) ) ;
#39823 = CARTESIAN_POINT ( 'NONE',  ( 69.11491457486368972, 59.02763561571557460, -3.981537309218733167 ) ) ;
#39824 = EDGE_CURVE ( 'NONE', #15453, #6853, #479, .T. ) ;
#39825 = VERTEX_POINT ( 'NONE', #35443 ) ;
#39826 = CARTESIAN_POINT ( 'NONE',  ( -0.9919418010453353585, -27.33356058713898307, 7.750000000000000888 ) ) ;
#39827 = DIRECTION ( 'NONE',  ( -0.9506097019758702471, 0.3103887796125167076, -7.179182702314986818E-16 ) ) ;
#39828 = CARTESIAN_POINT ( 'NONE',  ( -10.87867591359219155, -24.55319635012989110, 6.700000000000000178 ) ) ;
#39829 = FACE_BOUND ( 'NONE', #11474, .T. ) ;
#39830 = EDGE_CURVE ( 'NONE', #3023, #15769, #29406, .T. ) ;
#39831 = CARTESIAN_POINT ( 'NONE',  ( 2.177050749421512332, -32.93635181753877816, 7.761597726988850532 ) ) ;
#39832 = ORIENTED_EDGE ( 'NONE', *, *, #34488, .T. ) ;
#39833 = CARTESIAN_POINT ( 'NONE',  ( -64.08758708074093136, 38.76906266698302517, -3.000000000000000000 ) ) ;
#39834 = AXIS2_PLACEMENT_3D ( 'NONE', #14769, #30438, #11071 ) ;
#39835 = AXIS2_PLACEMENT_3D ( 'NONE', #403, #15829, #28384 ) ;
#39836 = EDGE_CURVE ( 'NONE', #33117, #28074, #15171, .T. ) ;
#39837 = EDGE_LOOP ( 'NONE', ( #18506, #10057, #28146, #14695 ) ) ;
#39838 = CARTESIAN_POINT ( 'NONE',  ( 78.92462413491021778, 65.07527128086411494, -3.128253119413328509 ) ) ;
#39839 = DIRECTION ( 'NONE',  ( -0.000000000000000000, -0.000000000000000000, 1.000000000000000000 ) ) ;
#39840 = CARTESIAN_POINT ( 'NONE',  ( 81.74240050578430328, 63.84683571418585046, -2.967158453529146200 ) ) ;
#39841 = CARTESIAN_POINT ( 'NONE',  ( 80.30026770407557990, 62.83227110018538042, 3.557377001560497742 ) ) ;
#39842 = ADVANCED_FACE ( 'NONE', ( #23468 ), #15561, .T. ) ;
#39843 = CARTESIAN_POINT ( 'NONE',  ( -66.99872204295122913, 28.48507918597134037, -9.800414904976365804 ) ) ;
#39845 = ORIENTED_EDGE ( 'NONE', *, *, #30918, .T. ) ;
#39844 = DIRECTION ( 'NONE',  ( -0.000000000000000000, -0.000000000000000000, -1.000000000000000000 ) ) ;
#39846 = CARTESIAN_POINT ( 'NONE',  ( 21.85643539959777115, 4.792808800112425160, -12.41435969090265523 ) ) ;
#39847 = ORIENTED_EDGE ( 'NONE', *, *, #18065, .T. ) ;
#39848 = CARTESIAN_POINT ( 'NONE',  ( -81.24663647081587214, 10.50463385007281936, 3.730473497536808125 ) ) ;
#39849 = CARTESIAN_POINT ( 'NONE',  ( 14.75140948485206316, -5.119342064155394390, 2.500052128446318189 ) ) ;
#39850 = CARTESIAN_POINT ( 'NONE',  ( -74.31397190940765540, 7.087263004850651527, -10.69992065686621352 ) ) ;
#39851 = CARTESIAN_POINT ( 'NONE',  ( 1.585995385899496846, -32.96800520477448515, 6.864276522220859711 ) ) ;
#39852 = CARTESIAN_POINT ( 'NONE',  ( 2.474049714983522108, -26.25912200567108457, 7.013842709614101167 ) ) ;
#39853 = CARTESIAN_POINT ( 'NONE',  ( -1.744021509508924206, -30.18346125941860336, 7.762796336881262249 ) ) ;
#39854 = CARTESIAN_POINT ( 'NONE',  ( 14.68017742504109613, 12.65464173479535859, 2.497594747247088520 ) ) ;
#39855 = CARTESIAN_POINT ( 'NONE',  ( 14.61802081865033820, 0.000000000000000000, 3.500000000000000000 ) ) ;
#39856 = LINE ( 'NONE', #40251, #29980 ) ;
#39857 = CARTESIAN_POINT ( 'NONE',  ( -0.03790328338398483987, -32.60774784362404688, 7.635761828346575797 ) ) ;
#39858 = CARTESIAN_POINT ( 'NONE',  ( 16.11725891507163766, 15.27317977277692052, -2.500000000000000000 ) ) ;
#39859 = CARTESIAN_POINT ( 'NONE',  ( -0.4205071184425808739, -26.91252637186863339, 6.870716933885664623 ) ) ;
#39860 = CARTESIAN_POINT ( 'NONE',  ( 4.165461883494793405, -31.91160235871856443, 6.939395833800444890 ) ) ;
#39861 = VERTEX_POINT ( 'NONE', #29450 ) ;
#39862=STYLED_ITEM('',(#40773),#39399);
#39863 = CARTESIAN_POINT ( 'NONE',  ( 67.66997365410338716, 58.45410198214950981, 3.990378031984447293 ) ) ;
#39864 = CARTESIAN_POINT ( 'NONE',  ( 20.42703419276611498, 3.672991389036573739, 3.394530734106728787 ) ) ;
#39865 = AXIS2_PLACEMENT_3D ( 'NONE', #7640, #21011, #1476 ) ;
#39866 = EDGE_CURVE ( 'NONE', #12570, #28242, #4927, .T. ) ;
#39867 = CARTESIAN_POINT ( 'NONE',  ( 87.00363285854439255, 0.09201467311058098009, -5.867932143725643535 ) ) ;
#39868 = CARTESIAN_POINT ( 'NONE',  ( -1.637662370169622461, -28.92386071996777375, 6.887041543973312585 ) ) ;
#39869 = CARTESIAN_POINT ( 'NONE',  ( 86.37929632089314680, 1.332399160353644696, 5.153246707575002361 ) ) ;
#39870 = CARTESIAN_POINT ( 'NONE',  ( -0.6653948319370099895, -32.14929951971039657, 6.880828092187096345 ) ) ;
#39871 = EDGE_LOOP ( 'NONE', ( #23724, #28820, #22069, #25727 ) ) ;
#39872 = CARTESIAN_POINT ( 'NONE',  ( -42.83131703149249603, -27.06993018339339585, 6.000000000000000000 ) ) ;
#39873 = UNCERTAINTY_MEASURE_WITH_UNIT (LENGTH_MEASURE( 1.000000000000000082E-05 ), #2598, 'distance_accuracy_value', 'NONE');
#39874 = CARTESIAN_POINT ( 'NONE',  ( 80.98923082824005348, 61.23822351929057106, -1.409197735201532131 ) ) ;
#39875 = CARTESIAN_POINT ( 'NONE',  ( -37.07867591359219261, -26.64985754041175525, 6.800000000000000711 ) ) ;
#39876 = CARTESIAN_POINT ( 'NONE',  ( 80.15465141033503471, 63.79803065853153754, 3.683925914261492185 ) ) ;
#39877 = CARTESIAN_POINT ( 'NONE',  ( 25.25995482075194332, 0.8517947254116883249, 4.614222942109635461 ) ) ;
#39879 = ORIENTED_EDGE ( 'NONE', *, *, #33298, .T. ) ;
#39878 = CARTESIAN_POINT ( 'NONE',  ( -0.7642813497525950961, -27.22783823854348384, 6.959317978105167946 ) ) ;
#39880 = EDGE_CURVE ( 'NONE', #18532, #561, #16618, .T. ) ;
#39881 = EDGE_CURVE ( 'NONE', #1672, #10219, #7412, .T. ) ;
#39882 = CARTESIAN_POINT ( 'NONE',  ( 74.91450450041774900, 59.74817859300107159, -3.564124015814033708 ) ) ;
#39884 = EDGE_CURVE ( 'NONE', #38896, #6366, #7204, .T. ) ;
#39883 = CARTESIAN_POINT ( 'NONE',  ( 3.234894228808482985, -32.60395886024767265, 6.895222827070022653 ) ) ;
#39886 = LINE ( 'NONE', #14549, #40693 ) ;
#39885 = DIRECTION ( 'NONE',  ( 0.3420201433256790380, -0.9396926207859046531, -0.000000000000000000 ) ) ;
#39887 = CARTESIAN_POINT ( 'NONE',  ( -1.223904788644516239, -27.83540028486481788, 7.784838882742139532 ) ) ;
#39888 = VECTOR ( 'NONE', #23534, 1000.000000000000000 ) ;
#39889 = DIRECTION ( 'NONE',  ( 0.000000000000000000, 1.000000000000000000, 0.000000000000000000 ) ) ;
#39890 = AXIS2_PLACEMENT_3D ( 'NONE', #17487, #29474, #30080 ) ;
#39891 = CARTESIAN_POINT ( 'NONE',  ( 21.85746124272390034, 5.806209280568897846, -3.202049940849499343 ) ) ;
#39892 = ORIENTED_EDGE ( 'NONE', *, *, #30189, .T. ) ;
#39893 = CARTESIAN_POINT ( 'NONE',  ( 5.200390093233090205, -29.56993018339339940, 7.202408869016171167 ) ) ;
#39894 = CARTESIAN_POINT ( 'NONE',  ( 25.50488203239457974, -4.522972804344248310, -2.044314315604920829 ) ) ;
#39895 = CARTESIAN_POINT ( 'NONE',  ( 3.462070670749302970, -32.59424523688933562, 7.635761828346575797 ) ) ;
#39896 = CARTESIAN_POINT ( 'NONE',  ( 1.010737851185899761, -32.99087142304168907, 7.780491323090171107 ) ) ;
#39897 = CARTESIAN_POINT ( 'NONE',  ( 79.61430779865300167, 65.89704723538268638, 2.499697124809921345 ) ) ;
#39898 = CARTESIAN_POINT ( 'NONE',  ( 85.83023444425720072, 0.8841707150779518631, 5.891289308415252890 ) ) ;
#39899 = CARTESIAN_POINT ( 'NONE',  ( 14.83041318099878048, 12.75128460074939163, 2.505930628224293244 ) ) ;
#39900 = ORIENTED_EDGE ( 'NONE', *, *, #23741, .F. ) ;
#39901 = CARTESIAN_POINT ( 'NONE',  ( 0.1833252022694565608, -32.73160443007695619, 7.501983001166818710 ) ) ;
#39902 = FACE_OUTER_BOUND ( 'NONE', #20125, .T. ) ;
#39903 = CARTESIAN_POINT ( 'NONE',  ( 14.70827183493699231, -5.600023334934355113, -2.501374264973752926 ) ) ;
#39904 = DIRECTION ( 'NONE',  ( -1.000000000000000000, 0.000000000000000000, 0.000000000000000000 ) ) ;
#39905 = FACE_OUTER_BOUND ( 'NONE', #34897, .T. ) ;
#39906 = B_SPLINE_CURVE_WITH_KNOTS ( 'NONE', 3,
 ( #12977, #38086, #9888, #4722, #7605, #26357, #10883, #29441, #17659, #7803, #30241, #26156, #17256, #7995, #14375, #4534, #17057, #39488, #20759, #36026, #20355, #10682 ),
 .UNSPECIFIED., .F., .F.,
 ( 4, 2, 1, 1, 2, 2, 2, 1, 1, 1, 1, 2, 2, 4 ),
 ( 0.000000000000000000, 0.1249999999999835132, 0.1874999999999753253, 0.2187499999999711897, 0.2343749999999692191, 0.2499999999999672484, 0.3749999999999468758, 0.4374999999999369393, 0.4687499999999320544, 0.4843749999999263367, 0.4921874999999268918, 0.4960937499999268363, 0.4999999999999268363, 1.000000000000000000 ),
 .UNSPECIFIED. ) ;
#39907 = CARTESIAN_POINT ( 'NONE',  ( -30.44874870218064089, -26.64985754041175525, 6.800000000000000711 ) ) ;
#39908 = ORIENTED_EDGE ( 'NONE', *, *, #2019, .T. ) ;
#39909 = CARTESIAN_POINT ( 'NONE',  ( -2.712160580843945734, -31.23359347163986399, 7.695279973900954751 ) ) ;
#39910 = VECTOR ( 'NONE', #31712, 1000.000000000000000 ) ;
#39911 = CARTESIAN_POINT ( 'NONE',  ( 87.00441857019603731, 0.6302321798448609069, -4.918210918608230564 ) ) ;
#39912 = EDGE_LOOP ( 'NONE', ( #15230, #1644, #15610, #2606, #17868, #33418 ) ) ;
#39913 = ORIENTED_EDGE ( 'NONE', *, *, #17819, .F. ) ;
#39915 = CARTESIAN_POINT ( 'NONE',  ( 34.79255493759018947, -3.835798378834245348, 5.376544616508660113 ) ) ;
#39914 = CARTESIAN_POINT ( 'NONE',  ( 78.67529526371438919, 66.04787469174289072, -1.130345937366645792 ) ) ;
#39916 = CARTESIAN_POINT ( 'NONE',  ( 22.13668169188128942, -2.652521926670949437, 3.661362574324665609 ) ) ;
#39917 = CARTESIAN_POINT ( 'NONE',  ( 14.68065631944763716, 12.91438177319697012, -2.499999999999999556 ) ) ;
#39918 = VECTOR ( 'NONE', #9730, 1000.000000000000114 ) ;
#39919 = CARTESIAN_POINT ( 'NONE',  ( -70.92837670882107659, -31.30579396504363388, 4.357836081054403010 ) ) ;
#39920 = AXIS2_PLACEMENT_3D ( 'NONE', #27712, #21141, #33707 ) ;
#39921 = ORIENTED_EDGE ( 'NONE', *, *, #34676, .F. ) ;
#39922 = CARTESIAN_POINT ( 'NONE',  ( -0.4513664592218429861, -26.80950562565463358, 7.750000000000000888 ) ) ;
#39923 = ORIENTED_EDGE ( 'NONE', *, *, #39129, .F. ) ;
#39924 = VERTEX_POINT ( 'NONE', #20561 ) ;
#39925 = DIRECTION ( 'NONE',  ( -0.000000000000000000, -0.000000000000000000, 1.000000000000000000 ) ) ;
#39926 = DIRECTION ( 'NONE',  ( -0.000000000000000000, -0.000000000000000000, 1.000000000000000000 ) ) ;
#39927 = CARTESIAN_POINT ( 'NONE',  ( 80.56654867478538051, 63.26449302893301052, -3.600689860192758385 ) ) ;
#39928 = DIRECTION ( 'NONE',  ( -1.000000000000000000, 0.000000000000000000, 0.000000000000000000 ) ) ;
#39929 = EDGE_LOOP ( 'NONE', ( #11606, #724, #3271, #31613 ) ) ;
#39931 = CARTESIAN_POINT ( 'NONE',  ( -20.34874870218063947, -26.64985754041175525, 6.800000000000000711 ) ) ;
#39930 = CARTESIAN_POINT ( 'NONE',  ( 22.04812685758551183, 2.736502322861370740, 5.115368073871701782 ) ) ;
#39932 = ORIENTED_EDGE ( 'NONE', *, *, #10577, .F. ) ;
#39933 = CARTESIAN_POINT ( 'NONE',  ( 82.22785179944503398, 62.76084426383153669, -1.971256063808603631 ) ) ;
#39934 = EDGE_CURVE ( 'NONE', #10017, #34818, #14143, .T. ) ;
#39936 = ADVANCED_FACE ( 'NONE', ( #11691 ), #2068, .F. ) ;
#39935 = DIRECTION ( 'NONE',  ( -0.000000000000000000, -0.000000000000000000, -1.000000000000000000 ) ) ;
#39937 = ORIENTED_EDGE ( 'NONE', *, *, #18126, .F. ) ;
#39939 = DIRECTION ( 'NONE',  ( -0.1736481776669340227, 0.9848077530122073542, -0.000000000000000000 ) ) ;
#39938 = DIRECTION ( 'NONE',  ( 0.000000000000000000, 0.000000000000000000, 1.000000000000000000 ) ) ;
#39940 = CARTESIAN_POINT ( 'NONE',  ( -1.794470407209020513, -29.38028857357967283, 6.931070083220557621 ) ) ;
#39941 = CARTESIAN_POINT ( 'NONE',  ( 75.06813672635826151, 59.39477395272206905, 3.294766324886222453 ) ) ;
#39942 = CARTESIAN_POINT ( 'NONE',  ( 23.95477519611412376, 2.905619892612372190, -3.859501322721603511 ) ) ;
#39943 = CARTESIAN_POINT ( 'NONE',  ( -56.10469124525552331, 30.75883671979822509, -2.489329600088171723 ) ) ;
#39944 = CARTESIAN_POINT ( 'NONE',  ( -17.07867591359219617, -26.64985754041175525, 6.800000000000000711 ) ) ;
#39945 = ORIENTED_EDGE ( 'NONE', *, *, #11883, .T. ) ;
#39946 = CARTESIAN_POINT ( 'NONE',  ( -1.653996770750948642, -29.01487273886056784, 7.691066658568944447 ) ) ;
#39947 = CARTESIAN_POINT ( 'NONE',  ( 81.76287911024846267, 64.24668757703155109, 2.864610283900509202 ) ) ;
#39948 = CARTESIAN_POINT ( 'NONE',  ( 85.18642856628412119, 2.672284839249654542, -1.189885989438959069 ) ) ;
#39949 = CARTESIAN_POINT ( 'NONE',  ( -8.878675913592189772, -26.64985754041175525, 6.700000000000000178 ) ) ;
#39950 = AXIS2_PLACEMENT_3D ( 'NONE', #34342, #755, #6113 ) ;
#39951 = DIRECTION ( 'NONE',  ( -0.000000000000000000, 1.000000000000000000, -0.000000000000000000 ) ) ;
#39952 = AXIS2_PLACEMENT_3D ( 'NONE', #28545, #28955, #38402 ) ;
#39953 = VECTOR ( 'NONE', #25459, 1000.000000000000000 ) ;
#39954 = CARTESIAN_POINT ( 'NONE',  ( -0.9205506017878787306, -27.40413144861377148, 7.652160403243376763 ) ) ;
#39955 = DIRECTION ( 'NONE',  ( -0.4999999999999918954, -0.8660254037844432595, -0.000000000000000000 ) ) ;
#39956 = CARTESIAN_POINT ( 'NONE',  ( -1.645585159361036220, -30.17362680341680203, 7.635761828346577573 ) ) ;
#39957 = CARTESIAN_POINT ( 'NONE',  ( 36.99319814093074399, -2.718620650874782108, -5.980081272406960302 ) ) ;
#39958 = LINE ( 'NONE', #11129, #2288 ) ;
#39959 = CARTESIAN_POINT ( 'NONE',  ( 5.185009940666303940, -29.62933811247615168, 7.785593909369614707 ) ) ;
#39960 = LINE ( 'NONE', #1907, #3996 ) ;
#39961 = EDGE_CURVE ( 'NONE', #33153, #2897, #38212, .T. ) ;
#39962 = CARTESIAN_POINT ( 'NONE',  ( 0.5371711504799139281, -32.87097875789517332, 7.695279973900954751 ) ) ;
#39963 = CARTESIAN_POINT ( 'NONE',  ( -0.4487487021806388365, -26.64985754041175525, 6.800000000000000711 ) ) ;
#39964 = VERTEX_POINT ( 'NONE', #24684 ) ;
#39965 = CARTESIAN_POINT ( 'NONE',  ( 34.78606437710333665, -3.774923618171289519, 5.430246727453117650 ) ) ;
#39966 = CIRCLE ( 'NONE', #10376, 0.1000000000000028644 ) ;
#39967 = CARTESIAN_POINT ( 'NONE',  ( -71.87513448197603338, -0.4420453205300980959, 5.937089484129752570 ) ) ;
#39968 = CARTESIAN_POINT ( 'NONE',  ( 66.74992980603514070, 57.79401841677491092, -3.997717836767872512 ) ) ;
#39969 = CARTESIAN_POINT ( 'NONE',  ( -70.92837670882107659, 13.87661300689600097, 0.000000000000000000 ) ) ;
#39970 = TOROIDAL_SURFACE ( 'NONE', #39284, 5.329987104167480894, 1.000000000000000000 ) ;
#39971 = EDGE_LOOP ( 'NONE', ( #11079, #21626, #24498, #27916, #32601, #36827 ) ) ;
#39972 = CARTESIAN_POINT ( 'NONE',  ( 4.550595850147784560, -31.61296642115005895, 7.501983001166816933 ) ) ;
#39973 = CARTESIAN_POINT ( 'NONE',  ( -71.75720568778372410, 2.602768977313620002, -9.965624305424430673 ) ) ;
#39974 = CARTESIAN_POINT ( 'NONE',  ( 15.58057500401926809, 10.76795092870248283, 2.638123565644369783 ) ) ;
#39975 = FACE_OUTER_BOUND ( 'NONE', #36216, .T. ) ;
#39976 = ORIENTED_EDGE ( 'NONE', *, *, #9324, .T. ) ;
#39977 = CYLINDRICAL_SURFACE ( 'NONE', #3691, 0.1000000000000028644 ) ;
#39978 = DIRECTION ( 'NONE',  ( 0.000000000000000000, 0.000000000000000000, 1.000000000000000000 ) ) ;
#39979 = ORIENTED_EDGE ( 'NONE', *, *, #13933, .F. ) ;
#39980 = CARTESIAN_POINT ( 'NONE',  ( 23.42804606522540212, 3.768913320211875195, 3.161532174550911289 ) ) ;
#39981 = CARTESIAN_POINT ( 'NONE',  ( 81.03660848153758423, 66.10018949144991041, -1.263752851813363387 ) ) ;
#39982 = CARTESIAN_POINT ( 'NONE',  ( 79.19089293128583051, 65.62284279856316971, 2.735335646780914676 ) ) ;
#39984 = EDGE_CURVE ( 'NONE', #7963, #33743, #10211, .T. ) ;
#39983 = LINE ( 'NONE', #24125, #262 ) ;
#39985 = ORIENTED_EDGE ( 'NONE', *, *, #32001, .T. ) ;
#39986 = CARTESIAN_POINT ( 'NONE',  ( 77.65795924533195205, 64.82981391430574547, -2.842954625922224476 ) ) ;
#39988 = CARTESIAN_POINT ( 'NONE',  ( 2.255350295996689347, -26.21552723005750352, 7.695279973900954751 ) ) ;
#39987 = CARTESIAN_POINT ( 'NONE',  ( 26.75722929591961474, 0.8862554030004115013, 4.383001231454183966 ) ) ;
#39989 = CARTESIAN_POINT ( 'NONE',  ( 81.27686174477108239, 61.37652599617193516, -1.416821487223366871 ) ) ;
#39990 = CARTESIAN_POINT ( 'NONE',  ( 79.07090634323701295, 63.55465448991838429, 3.774260586041105814 ) ) ;
#39991 = ORIENTED_EDGE ( 'NONE', *, *, #36748, .F. ) ;
#39992 = CARTESIAN_POINT ( 'NONE',  ( -0.8336107809199673202, -27.30301714566001792, 7.768425012602596880 ) ) ;
#39993 = ORIENTED_EDGE ( 'NONE', *, *, #38755, .T. ) ;
#39994 = CARTESIAN_POINT ( 'NONE',  ( 81.82660409393668033, 65.45354236959411764, 1.617049763655828531 ) ) ;
#39996 = CARTESIAN_POINT ( 'NONE',  ( 1.664433243520564876, -26.17012032033359148, 7.695279973900954751 ) ) ;
#39995 = DIRECTION ( 'NONE',  ( 0.7468947394616094471, 0.6649422893489137509, 0.000000000000000000 ) ) ;
#39997 = AXIS2_PLACEMENT_3D ( 'NONE', #3827, #23144, #29322 ) ;
#39998 = CARTESIAN_POINT ( 'NONE',  ( 31.96905077431594933, -4.633974458378385286, -3.035954366531696369 ) ) ;
#39999 = CARTESIAN_POINT ( 'NONE',  ( 14.61802081865033642, -4.461995682952384357, -2.500000000000000000 ) ) ;
#40000 = CARTESIAN_POINT ( 'NONE',  ( -1.315039247493585250, -27.79308300620435901, 6.894806418505347700 ) ) ;
#40001 = CARTESIAN_POINT ( 'NONE',  ( -80.93496385967344509, -5.699872886623274404, -0.1912487157657831449 ) ) ;
#40002 = CARTESIAN_POINT ( 'NONE',  ( 22.30956144702520660, 0.2684327122098100760, -7.077481357559062047 ) ) ;
#40003 = ORIENTED_EDGE ( 'NONE', *, *, #31587, .F. ) ;
#40004 = CARTESIAN_POINT ( 'NONE',  ( -0.4171441595639596156, -26.78316706317107787, 7.013842709614101167 ) ) ;
#40005 = CARTESIAN_POINT ( 'NONE',  ( 5.168232458229329751, -29.09648105291681475, 6.870724624169668893 ) ) ;
#40006 = FACE_OUTER_BOUND ( 'NONE', #9705, .T. ) ;
#40007 = CARTESIAN_POINT ( 'NONE',  ( 36.96506824942532177, -2.310990836009445548, -5.934258570784053610 ) ) ;
#40008 = CARTESIAN_POINT ( 'NONE',  ( 3.348332484698080425, -32.65674733949929731, 7.761113333117551250 ) ) ;
#40009 = FACE_BOUND ( 'NONE', #23568, .T. ) ;
#40010 = CARTESIAN_POINT ( 'NONE',  ( -24.34874870218063592, -26.64985754041175525, 6.700000000000000178 ) ) ;
#40011 = CARTESIAN_POINT ( 'NONE',  ( -71.92837670882107659, -20.78299143688747819, 5.916079783099620570 ) ) ;
#40012 = DIRECTION ( 'NONE',  ( 0.000000000000000000, 1.000000000000000000, 0.000000000000000000 ) ) ;
#40013 = CARTESIAN_POINT ( 'NONE',  ( 4.933620711012202342, -28.51815776361375754, 7.759451378593094972 ) ) ;
#40014 = AXIS2_PLACEMENT_3D ( 'NONE', #130, #28727, #28932 ) ;
#40015 = DIRECTION ( 'NONE',  ( 1.000000000000000000, 0.000000000000000000, 0.000000000000000000 ) ) ;
#40016 = CARTESIAN_POINT ( 'NONE',  ( 22.26933136229914822, 1.666440873335421013, -5.843949089993668800 ) ) ;
#40017 = ORIENTED_EDGE ( 'NONE', *, *, #25714, .T. ) ;
#40018 = EDGE_CURVE ( 'NONE', #38606, #23338, #8197, .T. ) ;
#40019 = CARTESIAN_POINT ( 'NONE',  ( 0.000000000000000000, 0.000000000000000000, 6.000000000000000000 ) ) ;
#40020 = CARTESIAN_POINT ( 'NONE',  ( 69.80049859759003539, 58.98221833774336176, -3.985452289341161691 ) ) ;
#40021 = EDGE_CURVE ( 'NONE', #28284, #2900, #11898, .T. ) ;
#40022 = VERTEX_POINT ( 'NONE', #18288 ) ;
#40023 = CARTESIAN_POINT ( 'NONE',  ( 85.08782340246310127, 1.754895396694989840, 5.093632142551737907 ) ) ;
#40024 = AXIS2_PLACEMENT_3D ( 'NONE', #35060, #32569, #32366 ) ;
#40025 = DIRECTION ( 'NONE',  ( -0.4826092789263618510, 0.5751513419797912308, -0.6605219282605402364 ) ) ;
#40026 = CARTESIAN_POINT ( 'NONE',  ( 3.043375019476788346, -26.44640070252536290, 7.006423389747791219 ) ) ;
#40027 =( BOUNDED_CURVE ( )  B_SPLINE_CURVE ( 3, ( #19160, #3345, #4137, #18956 ),
 .UNSPECIFIED., .F., .T. ) 
 B_SPLINE_CURVE_WITH_KNOTS ( ( 4, 4 ),
 ( 4.708531083176468179, 4.895802057644189631 ),
 .UNSPECIFIED. ) 
 CURVE ( )  GEOMETRIC_REPRESENTATION_ITEM ( )  RATIONAL_B_SPLINE_CURVE ( ( 1.000000000000000000, 0.9970795998553221295, 0.9970795998553221295, 1.000000000000000000 ) ) 
 REPRESENTATION_ITEM ( '' )  );
#40029 = DIRECTION ( 'NONE',  ( 1.000000000000000000, 0.000000000000000000, 0.000000000000000000 ) ) ;
#40028 = LINE ( 'NONE', #11194, #37946 ) ;
#40030 = CARTESIAN_POINT ( 'NONE',  ( 2.211347688137016210, -32.93132991176759106, 7.782034975670476307 ) ) ;
#40031 = ORIENTED_EDGE ( 'NONE', *, *, #13562, .F. ) ;
#40032 = CARTESIAN_POINT ( 'NONE',  ( 22.18571586291277598, 5.278230443170779829, 3.067113879996727022 ) ) ;
#40033 = EDGE_CURVE ( 'NONE', #29737, #12570, #27426, .T. ) ;
#40034 = EDGE_LOOP ( 'NONE', ( #39733, #21730, #24521, #25063 ) ) ;
#40035 = CARTESIAN_POINT ( 'NONE',  ( 80.76403243373638929, 61.15693784680268408, -1.612955153530313046 ) ) ;
#40036 = CARTESIAN_POINT ( 'NONE',  ( 16.10543327323123108, 10.11511941432178219, -2.500000000000563993 ) ) ;
#40037 = CARTESIAN_POINT ( 'NONE',  ( 81.89445579901081373, 62.31310441928815180, -2.222430037836082839 ) ) ;
#40038 = CARTESIAN_POINT ( 'NONE',  ( 79.36500080098821286, 64.41263654525117488, 3.571698303486884996 ) ) ;
#40039 = ORIENTED_EDGE ( 'NONE', *, *, #34058, .T. ) ;
#40040 = CARTESIAN_POINT ( 'NONE',  ( 22.81955182245838643, 3.687635531278536050, 3.767940973477740485 ) ) ;
#40041 = CARTESIAN_POINT ( 'NONE',  ( -33.07867591359219972, -24.55319635012989110, 6.700000000000000178 ) ) ;
#40042 = CARTESIAN_POINT ( 'NONE',  ( 22.45979449916501736, 0.3571986981647585768, -9.138524188866155029 ) ) ;
#40043 = ORIENTED_EDGE ( 'NONE', *, *, #3447, .F. ) ;
#40044 = CARTESIAN_POINT ( 'NONE',  ( -79.86115014363866749, 11.51025212515079943, 4.513412623698347836 ) ) ;
#40045 = LINE ( 'NONE', #2405, #20061 ) ;
#40046 = EDGE_CURVE ( 'NONE', #13553, #36097, #22813, .T. ) ;
#40047 = CARTESIAN_POINT ( 'NONE',  ( -1.320963929511134394, -31.33668423227719302, 7.643192810543818716 ) ) ;
#40048 = CARTESIAN_POINT ( 'NONE',  ( -73.50452121051399956, 5.643715073541963889, -9.720672664084132109 ) ) ;
#40049 = TOROIDAL_SURFACE ( 'NONE', #26883, 3.449999999999999289, 0.05000000000000000278 ) ;
#40050 = DIRECTION ( 'NONE',  ( -0.000000000000000000, -0.000000000000000000, 1.000000000000000000 ) ) ;
#40051 = PLANE ( 'NONE',  #26765 ) ;
#40052 = DIRECTION ( 'NONE',  ( -0.000000000000000000, 1.000000000000000000, -0.000000000000000000 ) ) ;
#40053 = CARTESIAN_POINT ( 'NONE',  ( 14.96508221674406336, 11.84948168787969180, 2.542061030440761815 ) ) ;
#40054 = CARTESIAN_POINT ( 'NONE',  ( 3.090657818664316103, -26.35045347725774434, 7.387053503561885393 ) ) ;
#40055 = CARTESIAN_POINT ( 'NONE',  ( 29.58369257489212956, 0.1927579767638456509, 4.823648729257316248 ) ) ;
#40056 = CARTESIAN_POINT ( 'NONE',  ( -0.5730865926811068434, -32.23100210249002373, 6.894806418505347700 ) ) ;
#40057 = LINE ( 'NONE', #12256, #25676 ) ;
#40058 = CARTESIAN_POINT ( 'NONE',  ( 87.34473703301738112, 0.2479703299153093454, 4.572837505533756897 ) ) ;
#40059 = CARTESIAN_POINT ( 'NONE',  ( 26.66739313631886432, 1.596111124545895210, -4.344095840588632740 ) ) ;
#40060 = ORIENTED_EDGE ( 'NONE', *, *, #39253, .T. ) ;
#40061 = CARTESIAN_POINT ( 'NONE',  ( 67.70975997764571730, 58.34660981014267378, 3.996132678073276878 ) ) ;
#40062 = CARTESIAN_POINT ( 'NONE',  ( 21.25554478757682730, 3.326128526321320500, 3.523839850031435628 ) ) ;
#40063 = CYLINDRICAL_SURFACE ( 'NONE', #19150, 0.09010775117052784167 ) ;
#40064 = EDGE_CURVE ( 'NONE', #25477, #28596, #21397, .T. ) ;
#40065 = VECTOR ( 'NONE', #22558, 1000.000000000000000 ) ;
#40066 = DIRECTION ( 'NONE',  ( 0.000000000000000000, 0.000000000000000000, -1.000000000000000000 ) ) ;
#40067 = CARTESIAN_POINT ( 'NONE',  ( 87.79537149936930973, -0.4305974645707495441, -5.064761461465907999 ) ) ;
#40069 = CARTESIAN_POINT ( 'NONE',  ( 4.828954996240010900, -30.90115017889735682, 6.887945620086116882 ) ) ;
#40068 = CARTESIAN_POINT ( 'NONE',  ( 33.87650332550894916, -5.319205609767368337, 2.014658837789633949 ) ) ;
#40070 = CARTESIAN_POINT ( 'NONE',  ( -1.547122796906874598, -30.57677098347808098, 6.876076431790006716 ) ) ;
#40071 = ORIENTED_EDGE ( 'NONE', *, *, #21724, .F. ) ;
#40072 = DIRECTION ( 'NONE',  ( 1.000000000000000000, 0.000000000000000000, 0.000000000000000000 ) ) ;
#40073 = EDGE_CURVE ( 'NONE', #14142, #35485, #1931, .T. ) ;
#40074 = CARTESIAN_POINT ( 'NONE',  ( -68.92837670882107659, -36.87473357531881391, 0.000000000000000000 ) ) ;
#40075 = CARTESIAN_POINT ( 'NONE',  ( -0.6847619013603313265, -32.13139149473335721, 6.998987538705432776 ) ) ;
#40076 = VERTEX_POINT ( 'NONE', #19320 ) ;
#40077 = CARTESIAN_POINT ( 'NONE',  ( -69.94873531773163222, -21.01309677555362398, 5.931544551966180912 ) ) ;
#40078 = AXIS2_PLACEMENT_3D ( 'NONE', #37507, #3575, #28246 ) ;
#40079 = CARTESIAN_POINT ( 'NONE',  ( 78.62745313524290225, 65.95871297147078849, -1.682919622592493614 ) ) ;
#40080 = CARTESIAN_POINT ( 'NONE',  ( -1.525418950806410212, -28.21191307850770258, 6.898188844117813190 ) ) ;
#40081 = CARTESIAN_POINT ( 'NONE',  ( 80.25680044982712502, 63.48435701671617437, 3.692178340560210437 ) ) ;
#40083 = VERTEX_POINT ( 'NONE', #16024 ) ;
#40082 = CARTESIAN_POINT ( 'NONE',  ( 4.790345179149528398, -27.92659140015631891, 7.754798119455333705 ) ) ;
#40084 = CARTESIAN_POINT ( 'NONE',  ( 75.06813672635826151, 59.39477395272206905, -3.294766324886222897 ) ) ;
#40085 = CARTESIAN_POINT ( 'NONE',  ( 3.215900811223072697, -32.61348645385951528, 6.939395833800443114 ) ) ;
#40087 = CARTESIAN_POINT ( 'NONE',  ( -1.225953191357326277, -31.30097466021442187, 7.695279973900954751 ) ) ;
#40086 = CARTESIAN_POINT ( 'NONE',  ( 4.976157933844921999, -30.80256632143474604, 6.887161170156908874 ) ) ;
#40088 = CARTESIAN_POINT ( 'NONE',  ( -1.188758931704360089, -27.77748128243219483, 7.768425012602592439 ) ) ;
#40089 = CARTESIAN_POINT ( 'NONE',  ( 22.24686819720471931, 5.023333803137271403, -3.219619871319814752 ) ) ;
#40090 = ORIENTED_EDGE ( 'NONE', *, *, #8165, .T. ) ;
#40091 = CARTESIAN_POINT ( 'NONE',  ( 5.016239155254060833, -30.32173691802341509, 6.876076431790006716 ) ) ;
#40092 = AXIS2_PLACEMENT_3D ( 'NONE', #18359, #1377, #13908 ) ;
#40093 = EDGE_CURVE ( 'NONE', #2900, #36291, #23467, .T. ) ;
#40094 = CARTESIAN_POINT ( 'NONE',  ( -0.9639628759317209195, -31.83956276478470926, 7.737115613922529000 ) ) ;
#40095 = CARTESIAN_POINT ( 'NONE',  ( 4.983950756172366603, -28.35822323759031605, 7.638132480492517473 ) ) ;
#40096 = CARTESIAN_POINT ( 'NONE',  ( 78.97265649164181411, 66.09949689503534387, 1.726519205789194045 ) ) ;
#40097 = CARTESIAN_POINT ( 'NONE',  ( 84.80660115723814840, 2.320002077609508717, 4.142190259225312587 ) ) ;
#40098 = CARTESIAN_POINT ( 'NONE',  ( 21.71182896267971074, 6.328908860361642574, -3.192117583127509928 ) ) ;
#40099 = VERTEX_POINT ( 'NONE', #38049 ) ;
#40100 = DIRECTION ( 'NONE',  ( 0.000000000000000000, 0.000000000000000000, -1.000000000000000000 ) ) ;
#40101 = DIRECTION ( 'NONE',  ( -0.7660444431189726844, -0.6427876096865458022, -0.000000000000000000 ) ) ;
#40102 = EDGE_CURVE ( 'NONE', #20830, #28641, #28799, .T. ) ;
#40103 = CARTESIAN_POINT ( 'NONE',  ( 86.00134810727946899, 0.2530519298808260320, -5.999722280616810899 ) ) ;
#40104 = ADVANCED_FACE ( 'NONE', ( #22015 ), #9426, .F. ) ;
#40105 = AXIS2_PLACEMENT_3D ( 'NONE', #967, #20475, #13906 ) ;
#40106 = CARTESIAN_POINT ( 'NONE',  ( 28.88853511041031652, -3.138669953830422354, -4.706520689280823788 ) ) ;
#40107 = CARTESIAN_POINT ( 'NONE',  ( -69.08758708074093136, 36.88538962427717394, -8.800414904976365804 ) ) ;
#40108 = DIRECTION ( 'NONE',  ( -1.000000000000000000, 0.000000000000000000, 0.000000000000000000 ) ) ;
#40109 = CARTESIAN_POINT ( 'NONE',  ( 1.894073117522566463, -26.17544468245638356, 7.006423389747790331 ) ) ;
#40110 = ORIENTED_EDGE ( 'NONE', *, *, #730, .F. ) ;
#40111 = CARTESIAN_POINT ( 'NONE',  ( 36.97894744516257504, -2.955629259446093116, 5.977857106677936905 ) ) ;
#40112 = EDGE_CURVE ( 'NONE', #22420, #40359, #10958, .T. ) ;
#40113 = EDGE_CURVE ( 'NONE', #4188, #31697, #34015, .T. ) ;
#40114 = CARTESIAN_POINT ( 'NONE',  ( 88.32659454254844889, -0.8548986265586405731, 1.105665148257566566 ) ) ;
#40115 = ORIENTED_EDGE ( 'NONE', *, *, #8921, .F. ) ;
#40116 = ORIENTED_EDGE ( 'NONE', *, *, #10188, .F. ) ;
#40118 = CARTESIAN_POINT ( 'NONE',  ( 33.45699141876632865, -3.835191985160780526, 5.087378379710845167 ) ) ;
#40117 = CARTESIAN_POINT ( 'NONE',  ( 78.77947119303418333, 66.08315628559921606, -1.459100623883114345 ) ) ;
#40119 = CARTESIAN_POINT ( 'NONE',  ( 24.40347370081251199, -3.150362192350396828, -3.888145324086332177 ) ) ;
#40120 = FACE_OUTER_BOUND ( 'NONE', #26007, .T. ) ;
#40121 = ORIENTED_EDGE ( 'NONE', *, *, #15727, .F. ) ;
#40122 = CARTESIAN_POINT ( 'NONE',  ( -1.740011302788441183, -30.21307731605675073, 7.695279973900954751 ) ) ;
#40123 = EDGE_LOOP ( 'NONE', ( #13656, #24938, #2343, #37802 ) ) ;
#40124 = VERTEX_POINT ( 'NONE', #10046 ) ;
#40125 = LINE ( 'NONE', #7518, #16757 ) ;
#40126 = CARTESIAN_POINT ( 'NONE',  ( 79.98933190693155382, 64.46315002137731653, -3.592474444481856821 ) ) ;
#40127 = CARTESIAN_POINT ( 'NONE',  ( 7.021324086407807030, -26.64985754041175525, 6.700000000000000178 ) ) ;
#40128 = ORIENTED_EDGE ( 'NONE', *, *, #3699, .F. ) ;
#40130 = CARTESIAN_POINT ( 'NONE',  ( 21.24912046457389891, 8.714595741889111125, -2.623796381800369115 ) ) ;
#40129 = CARTESIAN_POINT ( 'NONE',  ( 23.22046785484262799, 2.436457413438301689, 4.499336473899634647 ) ) ;
#40131 = ORIENTED_EDGE ( 'NONE', *, *, #33518, .F. ) ;
#40132 = CARTESIAN_POINT ( 'NONE',  ( 82.31242756469269750, 63.41700585080309338, -2.192618372227128631 ) ) ;
#40133 = CIRCLE ( 'NONE', #31604, 0.1000000000000028644 ) ;
#40134 = CARTESIAN_POINT ( 'NONE',  ( -63.08758708074093136, 41.61202515287869375, -4.000000000000000000 ) ) ;
#40135 = ORIENTED_EDGE ( 'NONE', *, *, #29249, .T. ) ;
#40137 = CARTESIAN_POINT ( 'NONE',  ( 85.20403636288057214, 2.652506926396006381, -1.368233707929553011 ) ) ;
#40136 = CYLINDRICAL_SURFACE ( 'NONE', #4241, 0.1000000000000028644 ) ;
#40138 = CARTESIAN_POINT ( 'NONE',  ( -1.795240888762144937, -29.39510444811675072, 7.006908160621414972 ) ) ;
#40139 = CARTESIAN_POINT ( 'NONE',  ( 74.03116782478153368, 60.19763641771454132, 3.876585409280477013 ) ) ;
#40140 = CARTESIAN_POINT ( 'NONE',  ( 24.37218514414048798, 2.867522109304287525, -3.798528098029286593 ) ) ;
#40141 = VERTEX_POINT ( 'NONE', #14961 ) ;
#40142 = CARTESIAN_POINT ( 'NONE',  ( 21.85643539959780313, -10.31987362501297056, 12.61309593674697993 ) ) ;
#40143 = CARTESIAN_POINT ( 'NONE',  ( -28.97867591359219475, -24.55319635012989110, 6.700000000000000178 ) ) ;
#40144 = ORIENTED_EDGE ( 'NONE', *, *, #26497, .T. ) ;
#40145 = CARTESIAN_POINT ( 'NONE',  ( -67.91293329751579222, 37.48821246049005396, 8.742028012086855426 ) ) ;
#40146 = ORIENTED_EDGE ( 'NONE', *, *, #17743, .F. ) ;
#40147 = CARTESIAN_POINT ( 'NONE',  ( 79.38089166731855073, 66.16750285958215727, 1.809109834152207164 ) ) ;
#40148 = CARTESIAN_POINT ( 'NONE',  ( 87.78348876263190448, -0.2448564372010923473, 4.525229423219702340 ) ) ;
#40149 = CARTESIAN_POINT ( 'NONE',  ( 5.140436678832947415, -30.21500869279741508, 6.887161170156907097 ) ) ;
#40150 = AXIS2_PLACEMENT_3D ( 'NONE', #26211, #16914, #29494 ) ;
#40151 = CARTESIAN_POINT ( 'NONE',  ( 3.555970037240517190, -26.60239115476207772, 7.753200566781577763 ) ) ;
#40152 = CARTESIAN_POINT ( 'NONE',  ( 33.96310664646391331, -3.802643679816640532, 5.242972732703274019 ) ) ;
#40153 = B_SPLINE_CURVE_WITH_KNOTS ( 'NONE', 3,
 ( #12196, #2763, #34264, #12407, #6650, #19200, #37920, #37706, #9111, #37512, #5831, #9726, #15491, #22096, #31562, #22307, #3580, #15288, #77, #40394, #2972, #34874, #24767, #481, #18782, #8897, #9307, #19002, #31766, #25175, #6238 ),
 .UNSPECIFIED., .F., .F.,
 ( 4, 3, 3, 3, 3, 3, 3, 3, 3, 3, 4 ),
 ( 8.055264624169107152E-18, 3.077658087705768824E-05, 6.152638666999025010E-05, 9.267501192706735535E-05, 0.0001241882240135194423, 0.0001556618703051683992, 0.0001866161554452216802, 0.0002167966385861003697, 0.0002463805737537802000, 0.0002758761370306561764, 0.0002847094172290048322 ),
 .UNSPECIFIED. ) ;
#40154 = CARTESIAN_POINT ( 'NONE',  ( 1.058406696066443331, -26.12931067392286266, 7.678495282201404315 ) ) ;
#40155 = CARTESIAN_POINT ( 'NONE',  ( 35.78609575529035425, -3.165688131210327771, -5.791683751246249123 ) ) ;
#40156 = FACE_OUTER_BOUND ( 'NONE', #38514, .T. ) ;
#40157 = CARTESIAN_POINT ( 'NONE',  ( 5.189124044873195452, -29.59783471987984171, 7.781480525794717273 ) ) ;
#40158 = PLANE ( 'NONE',  #12513 ) ;
#40159 = CARTESIAN_POINT ( 'NONE',  ( -64.08758708074093136, 36.14363715547680300, -3.800414904976364028 ) ) ;
#40160 = ADVANCED_FACE ( 'NONE', ( #18914 ), #40513, .F. ) ;
#40161 = CARTESIAN_POINT ( 'NONE',  ( 1.736346942945644400, -33.06974547922812491, 7.701614758090453705 ) ) ;
#40162 = VECTOR ( 'NONE', #9225, 1000.000000000000000 ) ;
#40163 = EDGE_CURVE ( 'NONE', #36954, #17549, #25469, .T. ) ;
#40164 = ORIENTED_EDGE ( 'NONE', *, *, #7304, .F. ) ;
#40165 = CARTESIAN_POINT ( 'NONE',  ( 37.13782911524162955, -2.596434994875571167, 5.986181626017550883 ) ) ;
#40166 = CARTESIAN_POINT ( 'NONE',  ( -71.03752578197757828, 0.2110339550563472832, 6.011051262898297942 ) ) ;
#40167 = B_SPLINE_CURVE_WITH_KNOTS ( 'NONE', 3,
 ( #29693, #7669, #7870, #1117, #17317, #13649 ),
 .UNSPECIFIED., .F., .F.,
 ( 4, 2, 4 ),
 ( 0.0002345877247508168376, 0.0005913096522288236161, 0.0009480315797068302863 ),
 .UNSPECIFIED. ) ;
#40168 = CARTESIAN_POINT ( 'NONE',  ( 66.88885785885000246, 57.86870549787170859, -3.998465113252547720 ) ) ;
#40169 = CARTESIAN_POINT ( 'NONE',  ( -89.00859394718983708, 2.429809908903242555, 12.50000000000000000 ) ) ;
#40170 = ORIENTED_EDGE ( 'NONE', *, *, #37038, .F. ) ;
#40171 = CARTESIAN_POINT ( 'NONE',  ( -38.44874870218063734, -26.64985754041175525, 6.700000000000000178 ) ) ;
#40172 = CARTESIAN_POINT ( 'NONE',  ( -74.40237796511935642, -4.238142967041890863, -9.381656193524049669 ) ) ;
#40173 = CARTESIAN_POINT ( 'NONE',  ( -1.346119371218626792, -31.29294500718514271, 6.894806418505347700 ) ) ;
#40174 = PLANE ( 'NONE',  #29320 ) ;
#40175 = CARTESIAN_POINT ( 'NONE',  ( 4.938390203311415748E-15, -42.37473357531882101, 2.500000000000000000 ) ) ;
#40176 = ORIENTED_EDGE ( 'NONE', *, *, #23793, .T. ) ;
#40177 = CARTESIAN_POINT ( 'NONE',  ( 22.41328823501740786, 4.823693133274301381, 3.136477976532023870 ) ) ;
#40178 = CIRCLE ( 'NONE', #18280, 0.1000000000000028644 ) ;
#40179 = CARTESIAN_POINT ( 'NONE',  ( 82.43037228308448050, 64.59322875725442259, -1.000000000000000000 ) ) ;
#40180 = CARTESIAN_POINT ( 'NONE',  ( 81.15619658878986797, 61.33623061796058806, 1.560659576774481971 ) ) ;
#40181 = CARTESIAN_POINT ( 'NONE',  ( -2.707143391484601924, -27.16588715693004730, 7.754798119455333705 ) ) ;
#40182 = VERTEX_POINT ( 'NONE', #28381 ) ;
#40183 = CARTESIAN_POINT ( 'NONE',  ( 76.11285053945336188, 63.10974250081550707, -3.590981437842944324 ) ) ;
#40185 = CARTESIAN_POINT ( 'NONE',  ( 14.72845434633629935, -4.936288270239374221, -2.501305200057243106 ) ) ;
#40184 = CARTESIAN_POINT ( 'NONE',  ( 3.883994185819156453, -32.28945568252876086, 7.782861076432730840 ) ) ;
#40186 = CARTESIAN_POINT ( 'NONE',  ( 5.118969260771242702, -33.45454016556441701, 7.754798119455333705 ) ) ;
#40187 = CARTESIAN_POINT ( 'NONE',  ( 81.26611686294326375, 61.37229692769314227, -1.428845309148531584 ) ) ;
#40188 = CARTESIAN_POINT ( 'NONE',  ( 76.31986902294670472, 64.06746608568100498, 3.012346708716361565 ) ) ;
#40189 = ORIENTED_EDGE ( 'NONE', *, *, #32111, .F. ) ;
#40190 = EDGE_LOOP ( 'NONE', ( #7276, #16619, #3178, #2543 ) ) ;
#40191 = DIRECTION ( 'NONE',  ( 0.000000000000000000, 0.000000000000000000, 1.000000000000000000 ) ) ;
#40192 = AXIS2_PLACEMENT_3D ( 'NONE', #13630, #38324, #7246 ) ;
#40193 = EDGE_LOOP ( 'NONE', ( #25829, #25851, #37563, #34181 ) ) ;
#40194 = CARTESIAN_POINT ( 'NONE',  ( 81.53194397951713768, 65.66224036380459950, 1.718006205139014364 ) ) ;
#40196 = FACE_OUTER_BOUND ( 'NONE', #5127, .T. ) ;
#40195 = CYLINDRICAL_SURFACE ( 'NONE', #32799, 3.399999999999999911 ) ;
#40197 = CARTESIAN_POINT ( 'NONE',  ( 33.19459970134796123, -3.309813850278316760, -5.543304389637502716 ) ) ;
#40198 = CARTESIAN_POINT ( 'NONE',  ( -1.773855778497440250, -29.99374101709560492, 6.921725064902953584 ) ) ;
#40199 = CARTESIAN_POINT ( 'NONE',  ( -59.93345510331042902, 24.73247967741478703, -12.49999999999999645 ) ) ;
#40200 = CARTESIAN_POINT ( 'NONE',  ( -64.38387608637887638, 34.70929407487223273, 5.501206404649374271 ) ) ;
#40201 = CARTESIAN_POINT ( 'NONE',  ( -69.92837670882107659, 28.72470171467712063, 3.916079783099620126 ) ) ;
#40202 = CARTESIAN_POINT ( 'NONE',  ( 5.001421652434105525, -30.73319741649938308, 7.698786668945012401 ) ) ;
#40203 = LINE ( 'NONE', #15706, #27580 ) ;
#40204 = CARTESIAN_POINT ( 'NONE',  ( 5.149536281657578485, -30.16439681061213918, 7.635761828346576685 ) ) ;
#40205 = CARTESIAN_POINT ( 'NONE',  ( 35.35501206519987960, -3.679878928346165701, -5.594686265449704266 ) ) ;
#40206 = FACE_OUTER_BOUND ( 'NONE', #12894, .T. ) ;
#40207 = CARTESIAN_POINT ( 'NONE',  ( 86.00134810727946899, 0.2530519298808260320, -5.999722280616810899 ) ) ;
#40208 = CARTESIAN_POINT ( 'NONE',  ( -0.08065709997538077214, -26.55697965350343281, 7.695279973900954751 ) ) ;
#40209 = CARTESIAN_POINT ( 'NONE',  ( 0.4745948466847342839, -32.83438907916249150, 7.783750581861599294 ) ) ;
#40210 = DIRECTION ( 'NONE',  ( 0.5000000000000101030, -0.8660254037844328234, -0.000000000000000000 ) ) ;
#40211 = CARTESIAN_POINT ( 'NONE',  ( 5.098465114614175064, -29.68432489072703717, 6.864276522220859711 ) ) ;
#40212 = DIRECTION ( 'NONE',  ( 0.000000000000000000, -1.000000000000000000, 0.000000000000000000 ) ) ;
#40213 = CYLINDRICAL_SURFACE ( 'NONE', #19767, 0.1000000000000028644 ) ;
#40214 = CARTESIAN_POINT ( 'NONE',  ( 21.82665949262245064, 2.023054712012288370, -6.063193687149706079 ) ) ;
#40215 = EDGE_CURVE ( 'NONE', #320, #32452, #17133, .T. ) ;
#40216 = ORIENTED_EDGE ( 'NONE', *, *, #14897, .T. ) ;
#40217 = ORIENTED_EDGE ( 'NONE', *, *, #27413, .F. ) ;
#40218 = EDGE_CURVE ( 'NONE', #28074, #3507, #20167, .T. ) ;
#40219 = CARTESIAN_POINT ( 'NONE',  ( 69.77571843317402056, 59.04509999696490041, -3.985452289341159915 ) ) ;
#40220 = ORIENTED_EDGE ( 'NONE', *, *, #27893, .F. ) ;
#40221 = FACE_OUTER_BOUND ( 'NONE', #34542, .T. ) ;
#40222 = AXIS2_PLACEMENT_3D ( 'NONE', #32911, #19550, #26334 ) ;
#40223 = DIRECTION ( 'NONE',  ( 0.000000000000000000, 0.000000000000000000, 1.000000000000000000 ) ) ;
#40224 = CARTESIAN_POINT ( 'NONE',  ( 69.92361841086972163, 58.66916198470556765, 3.954846139149858164 ) ) ;
#40225 = DIRECTION ( 'NONE',  ( 0.000000000000000000, 0.000000000000000000, 1.000000000000000000 ) ) ;
#40226 = LINE ( 'NONE', #12008, #26033 ) ;
#40227 = CARTESIAN_POINT ( 'NONE',  ( 5.037724831097187383, -30.21969694727531675, 7.785172627573962778 ) ) ;
#40228 = ORIENTED_EDGE ( 'NONE', *, *, #1083, .F. ) ;
#40229 = CARTESIAN_POINT ( 'NONE',  ( 22.87997942668749118, 4.340340381634286260, 3.050530276400981400 ) ) ;
#40230 = PRESENTATION_STYLE_ASSIGNMENT (( #11804 ) ) ;
#40231 = B_SPLINE_CURVE_WITH_KNOTS ( 'NONE', 3,
 ( #12497, #19288, #31854, #9815, #37804, #9196, #25066, #24648, #37600, #6330, #28140, #22394, #31046, #15586, #21984, #9609, #40692, #31450, #18460 ),
 .UNSPECIFIED., .F., .F.,
 ( 4, 3, 3, 3, 3, 3, 4 ),
 ( 1.143643797815609544E-18, 2.546128104244724791E-05, 5.711050680483827665E-05, 8.113074941675742821E-05, 0.0001053129305727045710, 0.0001360598016347049663, 0.0001612931755713734548 ),
 .UNSPECIFIED. ) ;
#40232 = ORIENTED_EDGE ( 'NONE', *, *, #29699, .T. ) ;
#40233 = CARTESIAN_POINT ( 'NONE',  ( 80.66846628934483476, 61.48471191768543775, -2.456741006817842798 ) ) ;
#40234 = CARTESIAN_POINT ( 'NONE',  ( 20.41154503683626942, 10.73873491509298006, -2.500000000000005773 ) ) ;
#40235 = CARTESIAN_POINT ( 'NONE',  ( 81.88105255503960223, 62.58610580235431087, -2.445541897054222868 ) ) ;
#40236 = EDGE_CURVE ( 'NONE', #2729, #3866, #4294, .T. ) ;
#40237 = CARTESIAN_POINT ( 'NONE',  ( 78.73387159939801450, 65.21990392541003700, 2.961936469198041433 ) ) ;
#40238 = PLANE ( 'NONE',  #26739 ) ;
#40239 = CARTESIAN_POINT ( 'NONE',  ( 4.667247927850000977, -31.42674373642585195, 7.751599049952172749 ) ) ;
#40240 = CARTESIAN_POINT ( 'NONE',  ( 21.85643539959776760, -10.46150609831112455, 5.349806725441734301 ) ) ;
#40241 = ORIENTED_EDGE ( 'NONE', *, *, #11054, .T. ) ;
#40242 = CARTESIAN_POINT ( 'NONE',  ( -80.34441969748445445, 11.50396638009181238, 3.391339543253393707 ) ) ;
#40243 = DIRECTION ( 'NONE',  ( -0.9848077530122091305, 0.1736481776669241417, -0.000000000000000000 ) ) ;
#40244 = EDGE_CURVE ( 'NONE', #6636, #13553, #26761, .T. ) ;
#40245 = CARTESIAN_POINT ( 'NONE',  ( -81.84931294303031279, 10.45753422446598790, -0.2086162088654086033 ) ) ;
#40246 = CARTESIAN_POINT ( 'NONE',  ( 28.70188943284334471, -3.562248915020447715, -4.654001059522564709 ) ) ;
#40247 = CARTESIAN_POINT ( 'NONE',  ( 36.71914689311213920, -3.458944023387923838, -5.860523124445346177 ) ) ;
#40248 = CARTESIAN_POINT ( 'NONE',  ( 1.062037487868057184, -32.90946697031814949, 6.894806418505346812 ) ) ;
#40249 = CARTESIAN_POINT ( 'NONE',  ( 14.67067001192470066, 13.26205651873949520, 2.496110885492619502 ) ) ;
#40250 = CARTESIAN_POINT ( 'NONE',  ( -40.34874870218063592, -26.64985754041175525, 6.800000000000000711 ) ) ;
#40251 = CARTESIAN_POINT ( 'NONE',  ( -2.253834945959114489, -26.23431501015891243, 7.635761828346577573 ) ) ;
#40252 = FACE_OUTER_BOUND ( 'NONE', #26950, .T. ) ;
#40253 = VECTOR ( 'NONE', #23074, 1000.000000000000000 ) ;
#40254 = CARTESIAN_POINT ( 'NONE',  ( 17.30847559132336144, 14.31944607823880844, -2.500000000000000444 ) ) ;
#40255 = CARTESIAN_POINT ( 'NONE',  ( 36.98394962418372245, -2.224080708393568973, -5.905313656129409061 ) ) ;
#40256 = CARTESIAN_POINT ( 'NONE',  ( 25.71016244533634065, 2.120338955733263031, -4.148448561564090475 ) ) ;
#40257 = EDGE_CURVE ( 'NONE', #20340, #5658, #40694, .T. ) ;
#40258 = VERTEX_POINT ( 'NONE', #13940 ) ;
#40259 =( BOUNDED_CURVE ( )  B_SPLINE_CURVE ( 3, ( #15912, #6858, #31571, #3591 ),
 .UNSPECIFIED., .F., .T. ) 
 B_SPLINE_CURVE_WITH_KNOTS ( ( 4, 4 ),
 ( 1.347909859412854683, 1.534781240595299634 ),
 .UNSPECIFIED. ) 
 CURVE ( )  GEOMETRIC_REPRESENTATION_ITEM ( )  RATIONAL_B_SPLINE_CURVE ( ( 1.000000000000000000, 0.9970920404276226723, 0.9970920404276226723, 1.000000000000000000 ) ) 
 REPRESENTATION_ITEM ( '' )  );
#40260 = CARTESIAN_POINT ( 'NONE',  ( 66.98331017875999294, 58.06610265625960210, 3.998453671246410046 ) ) ;
#40261 = CARTESIAN_POINT ( 'NONE',  ( 30.58586944111105055, 0.06670329603780118799, 4.980062666969890195 ) ) ;
#40262 = CARTESIAN_POINT ( 'NONE',  ( 4.986072540958928379, -30.76641830744928896, 7.767720160662274331 ) ) ;
#40263 = CARTESIAN_POINT ( 'NONE',  ( 2.495473842921097418, -33.76723158512031375, 7.695279973900954751 ) ) ;
#40264 = CARTESIAN_POINT ( 'NONE',  ( 85.76120202873109122, 1.723374722402979620, 5.285180586055219898 ) ) ;
#40266 = CARTESIAN_POINT ( 'NONE',  ( 37.03125091814749936, -2.782549409756239545, -5.986020328601505902 ) ) ;
#40265 = CARTESIAN_POINT ( 'NONE',  ( 33.51852797086635150, -3.949141208872448683, 4.993608438669980387 ) ) ;
#40267 = ORIENTED_EDGE ( 'NONE', *, *, #23146, .F. ) ;
#40268 = DIRECTION ( 'NONE',  ( 0.000000000000000000, 0.000000000000000000, 1.000000000000000000 ) ) ;
#40269 = DIRECTION ( 'NONE',  ( 0.000000000000000000, -0.000000000000000000, -1.000000000000000000 ) ) ;
#40270 = EDGE_CURVE ( 'NONE', #14835, #29836, #18487, .T. ) ;
#40271 = ORIENTED_EDGE ( 'NONE', *, *, #36241, .T. ) ;
#40272 = CARTESIAN_POINT ( 'NONE',  ( -70.40039547503687345, -21.63944369480664776, 3.977567636976454768 ) ) ;
#40273 = EDGE_CURVE ( 'NONE', #1813, #5958, #11035, .T. ) ;
#40274 = ORIENTED_EDGE ( 'NONE', *, *, #14347, .T. ) ;
#40275 = VERTEX_POINT ( 'NONE', #3912 ) ;
#40276 = CARTESIAN_POINT ( 'NONE',  ( 80.96252947514877008, 61.71397308826821870, -2.561782662428527146 ) ) ;
#40277 = CARTESIAN_POINT ( 'NONE',  ( -1.541782405220441410, -28.25144320491839878, 6.868546646838340486 ) ) ;
#40278 = CARTESIAN_POINT ( 'NONE',  ( 80.39951605126509548, 63.19197404919997751, 3.632888195267896858 ) ) ;
#40280 = VERTEX_POINT ( 'NONE', #16425 ) ;
#40279 = CARTESIAN_POINT ( 'NONE',  ( -0.8692302736362943483, -27.34348484300344850, 6.889465824494254598 ) ) ;
#40281 = CARTESIAN_POINT ( 'NONE',  ( 74.96893927862336682, 59.62365076172311262, -3.485789274173447083 ) ) ;
#40282 = CARTESIAN_POINT ( 'NONE',  ( 3.224946677277165552, -32.60896660074035225, 6.997764925645181933 ) ) ;
#40284 = CYLINDRICAL_SURFACE ( 'NONE', #3274, 3.399999999999999911 ) ;
#40283 = CYLINDRICAL_SURFACE ( 'NONE', #12717, 0.1000000000000028644 ) ;
#40285 = CARTESIAN_POINT ( 'NONE',  ( -68.71186372058383540, 37.81212149306784909, -9.800414904976365804 ) ) ;
#40286 = EDGE_CURVE ( 'NONE', #9808, #23165, #5746, .T. ) ;
#40287 = EDGE_CURVE ( 'NONE', #36231, #11923, #5084, .T. ) ;
#40288 = PLANE ( 'NONE',  #20880 ) ;
#40289 = CARTESIAN_POINT ( 'NONE',  ( 23.71667221069719744, 3.517694658488856430, -3.297412223443493495 ) ) ;
#40290 = EDGE_LOOP ( 'NONE', ( #15854, #16271, #39496, #16733 ) ) ;
#40291 = CARTESIAN_POINT ( 'NONE',  ( 2.431875535358183793, -26.14722233025152676, 7.750000000000000888 ) ) ;
#40292 = EDGE_CURVE ( 'NONE', #20694, #2944, #28764, .T. ) ;
#40293 = DIRECTION ( 'NONE',  ( 0.000000000000000000, 0.000000000000000000, 1.000000000000000000 ) ) ;
#40294 = CARTESIAN_POINT ( 'NONE',  ( 3.865379090973303011, -26.93911693003565944, 7.257242401810562349 ) ) ;
#40295 = CARTESIAN_POINT ( 'NONE',  ( 81.19366756170084898, 63.21158026472419067, 3.307636073424109924 ) ) ;
#40296 = CARTESIAN_POINT ( 'NONE',  ( 88.11323260317807637, -2.391772166421624490, 1.226420884133070599 ) ) ;
#40297 = CARTESIAN_POINT ( 'NONE',  ( 2.272716057154847924, -26.11704110451741556, 7.695279973900954751 ) ) ;
#40298 = ORIENTED_EDGE ( 'NONE', *, *, #21774, .F. ) ;
#40299 = CARTESIAN_POINT ( 'NONE',  ( -65.15514661499977933, 34.97220226750606997, 6.888442104241535802 ) ) ;
#40300 = CARTESIAN_POINT ( 'NONE',  ( 4.629620962406147733, -31.29608385994819741, 7.782167645815905033 ) ) ;
#40301 = AXIS2_PLACEMENT_3D ( 'NONE', #19495, #4066, #10417 ) ;
#40302 = CYLINDRICAL_SURFACE ( 'NONE', #36833, 0.1000000000000028644 ) ;
#40303 = CARTESIAN_POINT ( 'NONE',  ( 1.700390093233090871, -29.56993018339339940, 7.750000000000000888 ) ) ;
#40304 = CARTESIAN_POINT ( 'NONE',  ( 21.25143292528058225, 3.315796426267975328, -3.523198094474456532 ) ) ;
#40305 = CARTESIAN_POINT ( 'NONE',  ( -70.92837670882107659, -23.80776546975053165, 6.000000000000002665 ) ) ;
#40306 = CARTESIAN_POINT ( 'NONE',  ( -0.4306752572297538606, -26.92065449774550601, 7.784476445165073422 ) ) ;
#40307 = CARTESIAN_POINT ( 'NONE',  ( 31.71768278297239263, -0.5622167780584130803, 5.156709511976435678 ) ) ;
#40308 = VECTOR ( 'NONE', #9085, 1000.000000000000000 ) ;
#40309 = CARTESIAN_POINT ( 'NONE',  ( 4.327908163969745203, -31.72774129374396423, 7.703977250142846955 ) ) ;
#40310 = DIRECTION ( 'NONE',  ( 0.000000000000000000, 0.000000000000000000, 1.000000000000000000 ) ) ;
#40311 = VERTEX_POINT ( 'NONE', #36983 ) ;
#40313 = CARTESIAN_POINT ( 'NONE',  ( 37.10477226148266539, -3.126860894810321145, 5.976159207400391971 ) ) ;
#40312 = CARTESIAN_POINT ( 'NONE',  ( 79.98672868146590531, 65.19218680485843720, -3.233552917234638446 ) ) ;
#40314 = CARTESIAN_POINT ( 'NONE',  ( 26.94740486763593523, -2.794811601311201876, 4.412192273680850541 ) ) ;
#40315 = CARTESIAN_POINT ( 'NONE',  ( 22.11758564014485628, -3.078173236878668284, -3.562082636516995304 ) ) ;
#40316 = B_SPLINE_CURVE_WITH_KNOTS ( 'NONE', 3,
 ( #36170, #27908, #27705, #5277, #8756, #33247, #1966, #30358, #27057, #39821, #33661, #5438, #23497, #14417 ),
 .UNSPECIFIED., .F., .F.,
 ( 4, 2, 2, 2, 2, 2, 4 ),
 ( 0.007062463343506314266, 0.007356602418556547340, 0.007650741493606780415, 0.008239019643707230084, 0.008827297793807680620, 0.009121436868857905889, 0.009415575943908131157 ),
 .UNSPECIFIED. ) ;
#40317 = CARTESIAN_POINT ( 'NONE',  ( 4.851634552394991751, -30.84651091276440482, 7.754798119455333705 ) ) ;
#40318 = EDGE_LOOP ( 'NONE', ( #25914, #4252, #1563, #20510 ) ) ;
#40319 = EDGE_LOOP ( 'NONE', ( #37109, #25179, #18899, #8842 ) ) ;
#40320 = ORIENTED_EDGE ( 'NONE', *, *, #24928, .F. ) ;
#40321 = CARTESIAN_POINT ( 'NONE',  ( 81.11033257497912530, 61.28231361833088897, -1.235082213173757770 ) ) ;
#40322 = CARTESIAN_POINT ( 'NONE',  ( 14.76639648210999667, -4.521389705567960604, 2.511021882340067179 ) ) ;
#40324 = CARTESIAN_POINT ( 'NONE',  ( 29.33427167545534431, 1.276824085243427165, 4.194055504906347487 ) ) ;
#40323 = CARTESIAN_POINT ( 'NONE',  ( 23.31153495202840631, 2.940644873606350185, 4.073321330939048579 ) ) ;
#40325 = ORIENTED_EDGE ( 'NONE', *, *, #11768, .T. ) ;
#40326 = ADVANCED_FACE ( 'NONE', ( #12054 ), #27106, .T. ) ;
#40327 = CARTESIAN_POINT ( 'NONE',  ( 80.57628295459058165, 65.85481838934495613, -2.430878896394279565 ) ) ;
#40328 = VECTOR ( 'NONE', #17366, 1000.000000000000000 ) ;
#40329 = EDGE_CURVE ( 'NONE', #17714, #12496, #33926, .T. ) ;
#40330 = CARTESIAN_POINT ( 'NONE',  ( -59.01947560891952804, 27.90920910948504385, 6.147301388271928957 ) ) ;
#40331 = ORIENTED_EDGE ( 'NONE', *, *, #31072, .F. ) ;
#40333 = DIRECTION ( 'NONE',  ( 1.000000000000000000, 0.000000000000000000, 0.000000000000000000 ) ) ;
#40332 = CARTESIAN_POINT ( 'NONE',  ( -16.34874870218063592, -25.49307895267003587, 6.700000000000000178 ) ) ;
#40334 = DIRECTION ( 'NONE',  ( -0.000000000000000000, -0.000000000000000000, -1.000000000000000000 ) ) ;
#40335 = DIRECTION ( 'NONE',  ( -1.000000000000000000, 0.000000000000000000, 0.000000000000000000 ) ) ;
#40336 = CARTESIAN_POINT ( 'NONE',  ( 74.55930941259208566, 60.55296354997373953, 3.883841728571185481 ) ) ;
#40337 = CARTESIAN_POINT ( 'NONE',  ( 23.04763360661103988, 3.226630789359916651, -3.993616397825694442 ) ) ;
#40338 = ORIENTED_EDGE ( 'NONE', *, *, #6414, .F. ) ;
#40339 = FACE_OUTER_BOUND ( 'NONE', #1552, .T. ) ;
#40340 = ADVANCED_FACE ( 'NONE', ( #21143 ), #11236, .F. ) ;
#40341 = CARTESIAN_POINT ( 'NONE',  ( 21.85643539959773207, -10.94848525941816675, -12.02078412262589602 ) ) ;
#40342 = CARTESIAN_POINT ( 'NONE',  ( -58.83368549508428913, 29.29773222442904412, -5.899739961855157588 ) ) ;
#40343 = VERTEX_POINT ( 'NONE', #2432 ) ;
#40344 = CARTESIAN_POINT ( 'NONE',  ( 81.86163085503910963, 62.85586669281870087, 2.670779692148243178 ) ) ;
#40345 = CARTESIAN_POINT ( 'NONE',  ( 88.57583237253618336, -1.134854386742023546, -1.768762308819206375 ) ) ;
#40346 = CARTESIAN_POINT ( 'NONE',  ( 30.30396332325029718, -0.06004591992995000210, 5.542382567169830132 ) ) ;
#40347 = CARTESIAN_POINT ( 'NONE',  ( 2.736589650407802665, -32.91302612543738348, 6.895394898881668233 ) ) ;
#40348 = CARTESIAN_POINT ( 'NONE',  ( 16.24913492685886851, -3.406803814618201365, 2.736837790127818248 ) ) ;
#40349 = DIRECTION ( 'NONE',  ( 1.000000000000000000, 0.000000000000000000, 0.000000000000000000 ) ) ;
#40350 = CARTESIAN_POINT ( 'NONE',  ( 27.44843548912706765, 1.080599773242067574, -4.490390219635936653 ) ) ;
#40351 = CARTESIAN_POINT ( 'NONE',  ( 5.144801695975108835, -28.95639910736822031, 7.762796336881262249 ) ) ;
#40352 = CARTESIAN_POINT ( 'NONE',  ( 5.197623362990931639, -29.68617878646442421, 7.761113333117554802 ) ) ;
#40353 = B_SPLINE_CURVE_WITH_KNOTS ( 'NONE', 3,
 ( #17916, #31722, #27800, #9466, #22265, #9066, #25543, #3141, #34013, #34423, #3341, #6608, #16062, #2723, #22052, #21642, #34222, #8854, #5787, #34832, #21845, #19155, #24936, #36, #3536, #9265, #6197, #34630, #12148, #25133, #18742 ),
 .UNSPECIFIED., .F., .F.,
 ( 4, 3, 3, 3, 3, 3, 3, 3, 3, 3, 4 ),
 ( 0.000000000000000000, 3.025570593002915146E-05, 6.051145698343717938E-05, 9.076621574721707990E-05, 0.0001210204262067937246, 0.0001512763324577387405, 0.0001815301820994196414, 0.0002117781465860642275, 0.0002420274594459682145, 0.0002722905548971127528, 0.0002816827545175567822 ),
 .UNSPECIFIED. ) ;
#40354 = ORIENTED_EDGE ( 'NONE', *, *, #7073, .F. ) ;
#40355 = CARTESIAN_POINT ( 'NONE',  ( -10.44874870218064089, -26.64985754041175525, 6.700000000000000178 ) ) ;
#40356 = CARTESIAN_POINT ( 'NONE',  ( 5.200390093233090205, -29.56993018339339940, 7.620413589471895399 ) ) ;
#40357 = VECTOR ( 'NONE', #559, 1000.000000000000000 ) ;
#40358 = CARTESIAN_POINT ( 'NONE',  ( -2.664219611515487696, -32.04831937761618832, 7.695279973900954751 ) ) ;
#40359 = VERTEX_POINT ( 'NONE', #33710 ) ;
#40360 = CARTESIAN_POINT ( 'NONE',  ( 33.08016986529464276, -0.2095144213782778597, 5.024908790581100959 ) ) ;
#40361 = CARTESIAN_POINT ( 'NONE',  ( -8.448748702180639114, -26.64985754041175525, 6.800000000000000711 ) ) ;
#40362 = CARTESIAN_POINT ( 'NONE',  ( 67.03747645593968230, 57.91646344912344091, -3.998003515188802037 ) ) ;
#40363 = ORIENTED_EDGE ( 'NONE', *, *, #38192, .F. ) ;
#40364 = CARTESIAN_POINT ( 'NONE',  ( -71.81436415662651029, 1.349290789225021436, -9.960713035918328018 ) ) ;
#40365 = CARTESIAN_POINT ( 'NONE',  ( -71.05910886569641605, -21.78281089777250301, 5.999999999999995559 ) ) ;
#40366 = ORIENTED_EDGE ( 'NONE', *, *, #5532, .T. ) ;
#40367 = LINE ( 'NONE', #2121, #37180 ) ;
#40368 = LINE ( 'NONE', #30732, #18593 ) ;
#40369 = ORIENTED_EDGE ( 'NONE', *, *, #17357, .F. ) ;
#40370 = CARTESIAN_POINT ( 'NONE',  ( 23.14177627322540687, 4.014150865615426333, 3.136148348386343709 ) ) ;
#40371 = CARTESIAN_POINT ( 'NONE',  ( 79.00097698949592484, 66.21430696267364624, -1.024355359505926488 ) ) ;
#40373 = CIRCLE ( 'NONE', #33827, 3.000000000000002220 ) ;
#40372 = CARTESIAN_POINT ( 'NONE',  ( 80.94990806105060699, 62.43782317439323037, 3.178394274514596773 ) ) ;
#40374 = CARTESIAN_POINT ( 'NONE',  ( 21.71182896267971074, 6.328908860361642574, -3.192117583127509928 ) ) ;
#40375 = ORIENTED_EDGE ( 'NONE', *, *, #27284, .T. ) ;
#40376 = CARTESIAN_POINT ( 'NONE',  ( 76.98094665547928628, 64.12925941789167439, -3.220231295875725319 ) ) ;
#40378 = CARTESIAN_POINT ( 'NONE',  ( -18.34874870218063947, -25.49307895267003587, 6.700000000000000178 ) ) ;
#40377 = CARTESIAN_POINT ( 'NONE',  ( 2.323504162460518163, -33.01401688474696527, 7.638132480492516585 ) ) ;
#40379 = LINE ( 'NONE', #26476, #3957 ) ;
#40380 = CARTESIAN_POINT ( 'NONE',  ( 81.51347805234148325, 61.90211215308941206, -2.263370276487066679 ) ) ;
#40381 = CARTESIAN_POINT ( 'NONE',  ( 78.16578481971126280, 61.75018358139124786, 3.687756614093599783 ) ) ;
#40382 = VERTEX_POINT ( 'NONE', #5489 ) ;
#40383 = ADVANCED_FACE ( 'NONE', ( #20719 ), #33515, .F. ) ;
#40384 = EDGE_CURVE ( 'NONE', #30829, #4710, #7308, .T. ) ;
#40385 = AXIS2_PLACEMENT_3D ( 'NONE', #4581, #7451, #35678 ) ;
#40386 = DIRECTION ( 'NONE',  ( -0.000000000000000000, -0.000000000000000000, 1.000000000000000000 ) ) ;
#40387 = EDGE_CURVE ( 'NONE', #15332, #11154, #12290, .T. ) ;
#40388 = ORIENTED_EDGE ( 'NONE', *, *, #3402, .F. ) ;
#40389 = CARTESIAN_POINT ( 'NONE',  ( 3.628592791061993061, -26.64078201953907410, 7.387053503561886281 ) ) ;
#40390 = CARTESIAN_POINT ( 'NONE',  ( 80.61888529134442649, 66.16066543623880136, 1.646077502935600734 ) ) ;
#40392 = CARTESIAN_POINT ( 'NONE',  ( -1.699225164987326675, -29.51872342197794907, 6.892063359921933419 ) ) ;
#40391 = CARTESIAN_POINT ( 'NONE',  ( -64.08758708074094557, 42.86825253850305728, 2.416740211339933442 ) ) ;
#40393 = CARTESIAN_POINT ( 'NONE',  ( 28.89923929355584065, 0.07307017450661948410, 5.719397691353443669 ) ) ;
#40394 = CARTESIAN_POINT ( 'NONE',  ( -1.421068687739435177, -31.15312598190119431, 6.931070083220557621 ) ) ;
#40395 = LINE ( 'NONE', #12197, #33862 ) ;
#40396 = CARTESIAN_POINT ( 'NONE',  ( 1.531218635892081847, -33.06583936671340496, 7.013842709614101167 ) ) ;
#40397 = CARTESIAN_POINT ( 'NONE',  ( 22.62891770203226471, 0.3003589381232597000, -6.476356472173973700 ) ) ;
#40398 = CARTESIAN_POINT ( 'NONE',  ( 0.9267304714826859469, -32.88073836111571779, 7.013842709614101167 ) ) ;
#40399 = CYLINDRICAL_SURFACE ( 'NONE', #27675, 0.09010775117053086702 ) ;
#40400 = CARTESIAN_POINT ( 'NONE',  ( 81.16957891225059996, 61.30398062001309256, 1.000000000000000000 ) ) ;
#40401 = CARTESIAN_POINT ( 'NONE',  ( -60.75950795826495465, 23.17721540975219696, -46.17089178453873188 ) ) ;
#40402 = CARTESIAN_POINT ( 'NONE',  ( 36.48442795868031396, -3.515690391850441632, -5.817181155477498145 ) ) ;
#40403 = DIRECTION ( 'NONE',  ( 1.000000000000000000, 0.000000000000000000, -0.000000000000000000 ) ) ;
#40404 = CARTESIAN_POINT ( 'NONE',  ( 1.145332648700278844, -32.92431704737744269, 7.691066658568946224 ) ) ;
#40405 = DIRECTION ( 'NONE',  ( 1.000000000000000000, 0.000000000000000000, 0.000000000000000000 ) ) ;
#40406 = DIRECTION ( 'NONE',  ( 1.000000000000000000, 0.000000000000000000, -0.000000000000000000 ) ) ;
#40407 = CARTESIAN_POINT ( 'NONE',  ( 1.021324086407808585, -26.64985754041175525, 6.800000000000000711 ) ) ;
#40408 = CARTESIAN_POINT ( 'NONE',  ( -64.08758708074093136, 37.27332153486465671, -4.546479763848711109 ) ) ;
#40409 = CARTESIAN_POINT ( 'NONE',  ( 2.844292303360262064, -26.36812879825141920, 7.643333865083958401 ) ) ;
#40410 = CARTESIAN_POINT ( 'NONE',  ( 22.02569479573740452, 1.683627192489213442, -6.127589934087004586 ) ) ;
#40411 = DIRECTION ( 'NONE',  ( -0.000000000000000000, -1.000000000000000000, -0.000000000000000000 ) ) ;
#40413 = ORIENTED_EDGE ( 'NONE', *, *, #28450, .F. ) ;
#40412 = AXIS2_PLACEMENT_3D ( 'NONE', #17352, #36719, #39187 ) ;
#40414 = CARTESIAN_POINT ( 'NONE',  ( 69.75093826875801994, 59.10798165618643907, -3.985452289341158139 ) ) ;
#40415 = AXIS2_PLACEMENT_3D ( 'NONE', #7220, #1065, #7817 ) ;
#40416 = EDGE_LOOP ( 'NONE', ( #12767, #40241 ) ) ;
#40417 = CARTESIAN_POINT ( 'NONE',  ( -36.87867591359218977, -24.55319635012989110, 6.700000000000000178 ) ) ;
#40418 = CARTESIAN_POINT ( 'NONE',  ( 3.751251297819363728, -26.64985754041175525, 6.700000000000000178 ) ) ;
#40419 = CARTESIAN_POINT ( 'NONE',  ( 1.165815618567649148, -26.21221814525847904, 6.887041543973316138 ) ) ;
#40420 = EDGE_LOOP ( 'NONE', ( #11283, #4516, #38985, #4353, #6078 ) ) ;
#40421 = CARTESIAN_POINT ( 'NONE',  ( 22.88100581559600144, 4.343313832157520871, 3.044019733130736594 ) ) ;
#40422 = FILL_AREA_STYLE ('',( #15322 ) ) ;
#40423 = VERTEX_POINT ( 'NONE', #26903 ) ;
#40424 = CARTESIAN_POINT ( 'NONE',  ( 80.51696178947716476, 61.27878891920004634, -2.305838555345020247 ) ) ;
#40425 = CARTESIAN_POINT ( 'NONE',  ( -0.9974217071671265256, -27.34017228433088320, 7.737115613922534330 ) ) ;
#40426 = CARTESIAN_POINT ( 'NONE',  ( 81.85373309064766545, 62.29294994509992733, -2.264354540981538211 ) ) ;
#40427 = CARTESIAN_POINT ( 'NONE',  ( 79.10818533696262023, 64.58014521944369335, 3.489618106120226049 ) ) ;
#40428 = ORIENTED_EDGE ( 'NONE', *, *, #11831, .T. ) ;
#40429 = AXIS2_PLACEMENT_3D ( 'NONE', #11047, #38452, #4504 ) ;
#40430 = EDGE_CURVE ( 'NONE', #33628, #29749, #20930, .T. ) ;
#40431 = AXIS2_PLACEMENT_3D ( 'NONE', #17191, #29966, #10812 ) ;
#40432 = LINE ( 'NONE', #19044, #36043 ) ;
#40433 = CARTESIAN_POINT ( 'NONE',  ( 22.77977322753350720, -5.661609348961630594, -5.678499401198807917 ) ) ;
#40434 = ORIENTED_EDGE ( 'NONE', *, *, #4070, .F. ) ;
#40435 = CARTESIAN_POINT ( 'NONE',  ( -74.80457647086952022, 7.715846600713136105, 10.55247600905316574 ) ) ;
#40436 = CARTESIAN_POINT ( 'NONE',  ( 37.05408364730916304, -3.185536086795005328, 5.961296328585691029 ) ) ;
#40437 = VECTOR ( 'NONE', #10242, 1000.000000000000000 ) ;
#40438 = LINE ( 'NONE', #14928, #12949 ) ;
#40439 = CARTESIAN_POINT ( 'NONE',  ( 1.736346942945643512, -32.96974004645320377, 7.695279973900954751 ) ) ;
#40440 = DIRECTION ( 'NONE',  ( -0.000000000000000000, 0.000000000000000000, 1.000000000000000000 ) ) ;
#40441 = CARTESIAN_POINT ( 'NONE',  ( 34.63837955954176095, -0.7796828013290140191, -5.272681140724467141 ) ) ;
#40442 = CARTESIAN_POINT ( 'NONE',  ( 1.651251297819358754, -25.49307895267003587, 6.700000000000000178 ) ) ;
#40443 = CARTESIAN_POINT ( 'NONE',  ( 14.92554660196259775, 12.09598766256684499, 2.535890541581709456 ) ) ;
#40444 = CARTESIAN_POINT ( 'NONE',  ( -38.44874870218063734, -26.64985754041175525, 6.800000000000000711 ) ) ;
#40445 = CARTESIAN_POINT ( 'NONE',  ( 29.66023932424631226, -3.797131443868001721, 4.433517098046177551 ) ) ;
#40446 = FACE_OUTER_BOUND ( 'NONE', #37400, .T. ) ;
#40447 = CARTESIAN_POINT ( 'NONE',  ( -26.97867591359219475, -26.64985754041175525, 6.700000000000000178 ) ) ;
#40448 = CARTESIAN_POINT ( 'NONE',  ( 23.62484588740604607, 0.5005666067537509756, -5.479226438200067051 ) ) ;
#40449 = CARTESIAN_POINT ( 'NONE',  ( 36.83628562539227858, -2.061009687061731377, -5.854267444441933144 ) ) ;
#40450 = CARTESIAN_POINT ( 'NONE',  ( 24.72034790271620963, 2.638369506531949682, -3.924384734724444712 ) ) ;
#40451 = ORIENTED_EDGE ( 'NONE', *, *, #40512, .T. ) ;
#40452 = CARTESIAN_POINT ( 'NONE',  ( 66.97838688114072170, 58.07970146089488850, 3.998003515188801149 ) ) ;
#40453 = CARTESIAN_POINT ( 'NONE',  ( 36.94807309570725096, -2.593677492714873800, 5.973038417746441731 ) ) ;
#40454 = EDGE_CURVE ( 'NONE', #15393, #16288, #24515, .T. ) ;
#40455 = CARTESIAN_POINT ( 'NONE',  ( -58.99872204295123623, 28.48507918597134037, 12.49999999999999645 ) ) ;
#40456 = VECTOR ( 'NONE', #33081, 1000.000000000000000 ) ;
#40457 = CARTESIAN_POINT ( 'NONE',  ( -1.553683706606911130, -30.55532538593644176, 7.013842709614101167 ) ) ;
#40458 = AXIS2_PLACEMENT_3D ( 'NONE', #802, #10845, #7766 ) ;
#40459 = CARTESIAN_POINT ( 'NONE',  ( 87.33013056844055200, 0.1115698105147486796, -5.569409363020906056 ) ) ;
#40461 = CARTESIAN_POINT ( 'NONE',  ( 35.96180494042192066, -3.155136263811515018, -5.819107419128717318 ) ) ;
#40460 = CARTESIAN_POINT ( 'NONE',  ( 29.43591252028664584, 1.494051637964393553, 3.776330930280134002 ) ) ;
#40462 = ORIENTED_EDGE ( 'NONE', *, *, #32792, .F. ) ;
#40463 = CARTESIAN_POINT ( 'NONE',  ( 24.34570196473333681, 2.899197553801855065, 3.775102329553754021 ) ) ;
#40464 = CIRCLE ( 'NONE', #31275, 0.1000000000000028644 ) ;
#40465 = LINE ( 'NONE', #25656, #37070 ) ;
#40466 = ORIENTED_EDGE ( 'NONE', *, *, #18053, .F. ) ;
#40467 = FACE_OUTER_BOUND ( 'NONE', #29044, .T. ) ;
#40468 = EDGE_CURVE ( 'NONE', #32120, #16957, #474, .T. ) ;
#40469 = ORIENTED_EDGE ( 'NONE', *, *, #20769, .F. ) ;
#40470 = CARTESIAN_POINT ( 'NONE',  ( 78.85101321104539807, 65.59805058642685083, -2.603857329607544013 ) ) ;
#40471 = DIRECTION ( 'NONE',  ( 0.000000000000000000, 0.000000000000000000, 1.000000000000000000 ) ) ;
#40472 = CARTESIAN_POINT ( 'NONE',  ( 80.32629651820978722, 63.16159226777920566, 3.644176963625957111 ) ) ;
#40474 = EDGE_LOOP ( 'NONE', ( #22073, #30929, #15987, #37039 ) ) ;
#40473 = CARTESIAN_POINT ( 'NONE',  ( -1.330386342644613640, -31.11085822340198703, 6.887945620086118659 ) ) ;
#40475 = DIRECTION ( 'NONE',  ( 0.6427876096865369204, 0.7660444431189800119, 0.000000000000000000 ) ) ;
#40476 = ADVANCED_FACE ( 'NONE', ( #38396 ), #23368, .T. ) ;
#40477 = B_SPLINE_CURVE_WITH_KNOTS ( 'NONE', 3,
 ( #27208, #27011, #39149, #14240, #23322, #39768, #26814, #20220, #36092, #17121, #17931, #7668 ),
 .UNSPECIFIED., .F., .F.,
 ( 4, 2, 1, 1, 2, 2, 4 ),
 ( 0.9809184011985524476, 0.9815147011610976246, 0.9821110011236428017, 0.9833036010487331557, 0.9856888008989141969, 0.9904592005992760573, 1.000000000000000000 ),
 .UNSPECIFIED. ) ;
#40479 = FACE_OUTER_BOUND ( 'NONE', #32762, .T. ) ;
#40478 = DIRECTION ( 'NONE',  ( -0.9267318687906771491, 0.3757233601570964532, 0.000000000000000000 ) ) ;
#40480 = CYLINDRICAL_SURFACE ( 'NONE', #22879, 0.09010775117052932659 ) ;
#40481 = CARTESIAN_POINT ( 'NONE',  ( -81.78329181448161478, 33.71485196875532608, -9.800414904976365804 ) ) ;
#40482 = CARTESIAN_POINT ( 'NONE',  ( 22.90896498715502005, 4.192648223596282975, -3.220349011596035815 ) ) ;
#40483 = ORIENTED_EDGE ( 'NONE', *, *, #1049, .T. ) ;
#40484 = CARTESIAN_POINT ( 'NONE',  ( 25.50874925706157725, -4.568791516319697266, 1.869930813790659618 ) ) ;
#40485 = AXIS2_PLACEMENT_3D ( 'NONE', #2274, #14797, #39928 ) ;
#40486 = CARTESIAN_POINT ( 'NONE',  ( -77.50117670466831044, -4.927849438259591430, -7.545501454821059717 ) ) ;
#40487 = DIRECTION ( 'NONE',  ( -1.000000000000000000, 0.000000000000000000, 0.000000000000000000 ) ) ;
#40488 = CARTESIAN_POINT ( 'NONE',  ( 80.95544561733518663, 63.83034742112759830, 3.486376426170537002 ) ) ;
#40489 = CARTESIAN_POINT ( 'NONE',  ( 86.75210013534866960, -0.2795847087395720298, -5.842668109216860195 ) ) ;
#40490 =( BOUNDED_CURVE ( )  B_SPLINE_CURVE ( 3, ( #11580, #30554, #24570, #40207 ),
 .UNSPECIFIED., .F., .T. ) 
 B_SPLINE_CURVE_WITH_KNOTS ( ( 4, 4 ),
 ( 0.3200567940537017431, 0.9849192321825703811 ),
 .UNSPECIFIED. ) 
 CURVE ( )  GEOMETRIC_REPRESENTATION_ITEM ( )  RATIONAL_B_SPLINE_CURVE ( ( 0.9715283094173854384, 0.9610933789717652775, 0.9699361791336866823, 0.9980567099031494305 ) ) 
 REPRESENTATION_ITEM ( '' )  );
#40491 = CARTESIAN_POINT ( 'NONE',  ( 18.96867664023077893, 7.708620133838740784, 3.077328312083026152 ) ) ;
#40492 = ORIENTED_EDGE ( 'NONE', *, *, #7722, .T. ) ;
#40493 = CARTESIAN_POINT ( 'NONE',  ( -64.41585990636637860, 34.69667140566502894, -5.588029444252497591 ) ) ;
#40494 = CARTESIAN_POINT ( 'NONE',  ( -72.22997424438122493, -46.36506344532806168, 9.915082283677739028 ) ) ;
#40495 = VECTOR ( 'NONE', #29120, 1000.000000000000000 ) ;
#40496 = EDGE_CURVE ( 'NONE', #5343, #8047, #7718, .T. ) ;
#40497 = DIRECTION ( 'NONE',  ( -1.000000000000000000, 0.000000000000000000, 0.000000000000000000 ) ) ;
#40498 = LINE ( 'NONE', #182, #33770 ) ;
#40499 = CARTESIAN_POINT ( 'NONE',  ( -65.62105494223132496, 35.19887319331773767, -7.481751891074711835 ) ) ;
#40500 = FACE_OUTER_BOUND ( 'NONE', #26087, .T. ) ;
#40501 = CARTESIAN_POINT ( 'NONE',  ( 1.783834813784320295, -26.17095431136780803, 6.870716933885665512 ) ) ;
#40502 = CARTESIAN_POINT ( 'NONE',  ( 36.89707210798169257, -3.001693912205876114, 5.965078480148344298 ) ) ;
#40503 = B_SPLINE_CURVE_WITH_KNOTS ( 'NONE', 3,
 ( #31696, #26474, #1179, #23179, #23378, #23582, #35946, #38609, #32662, #10413, #36146, #26279, #7728, #22989, #33057, #32860, #4844, #7324, #26674, #35555, #19883, #38812, #10606 ),
 .UNSPECIFIED., .F., .F.,
 ( 4, 2, 2, 2, 1, 2, 2, 2, 2, 2, 2, 4 ),
 ( 0.06733963574726689605, 0.1651538230393540529, 0.2140609166853975620, 0.2385144635084192888, 0.2446278502141747135, 0.2476845435670523843, 0.2507412369199301105, 0.2629680103314415152, 0.3607821976235333628, 0.3852357444465562830, 0.4096892912695793143, 0.4585963849156251548 ),
 .UNSPECIFIED. ) ;
#40504 = CARTESIAN_POINT ( 'NONE',  ( 4.303098841883999270, -31.75760181544790584, 7.769368695748487319 ) ) ;
#40505 = CARTESIAN_POINT ( 'NONE',  ( 86.69860591627480062, 0.9737354674733970095, 5.003702464200671329 ) ) ;
#40506 = EDGE_LOOP ( 'NONE', ( #6632, #6817, #3569, #32439 ) ) ;
#40508 = CARTESIAN_POINT ( 'NONE',  ( -21.07867591359219617, -26.64985754041175525, 6.800000000000000711 ) ) ;
#40507 = CARTESIAN_POINT ( 'NONE',  ( 78.67345636894508232, 66.04656848779336542, -1.137963815189258598 ) ) ;
#40509 =( REPRESENTATION_RELATIONSHIP ('NONE','NONE', #24012, #29798 ) REPRESENTATION_RELATIONSHIP_WITH_TRANSFORMATION ( #8929 )SHAPE_REPRESENTATION_RELATIONSHIP( ) );
#40510 = DIRECTION ( 'NONE',  ( 0.000000000000000000, 0.000000000000000000, 1.000000000000000000 ) ) ;
#40511 = EDGE_CURVE ( 'NONE', #5237, #3514, #38724, .T. ) ;
#40512 = EDGE_CURVE ( 'NONE', #21149, #9410, #40028, .T. ) ;
#40513 = CYLINDRICAL_SURFACE ( 'NONE', #16237, 0.1000000000000028644 ) ;
#40514 = DIRECTION ( 'NONE',  ( 0.9396926207859082059, 0.3420201433256695456, -0.000000000000000000 ) ) ;
#40515 = VERTEX_POINT ( 'NONE', #20467 ) ;
#40516 = EDGE_CURVE ( 'NONE', #36812, #11880, #23764, .T. ) ;
#40517 = CARTESIAN_POINT ( 'NONE',  ( -1.653394165169625118, -29.01124319760426573, 7.721096864323898856 ) ) ;
#40518 = ORIENTED_EDGE ( 'NONE', *, *, #40329, .F. ) ;
#40519 = ORIENTED_EDGE ( 'NONE', *, *, #9288, .T. ) ;
#40520 = CARTESIAN_POINT ( 'NONE',  ( 81.06760980982289766, 61.95377044681377043, -2.747716423863113100 ) ) ;
#40521 = AXIS2_PLACEMENT_3D ( 'NONE', #37028, #24272, #11493 ) ;
#40522 = CARTESIAN_POINT ( 'NONE',  ( -1.506651383277110012, -28.44082214252960839, 7.691066658568946224 ) ) ;
#40523 = ORIENTED_EDGE ( 'NONE', *, *, #25014, .T. ) ;
#40525 = CARTESIAN_POINT ( 'NONE',  ( 32.56727300831884264, 0.05559756199407518001, 4.835980446979140090 ) ) ;
#40524 = CARTESIAN_POINT ( 'NONE',  ( 23.34681557898295168, 2.817057717204138445, 4.150130206757231655 ) ) ;
#40526 = ORIENTED_EDGE ( 'NONE', *, *, #27284, .F. ) ;
#40527 = CIRCLE ( 'NONE', #23442, 0.1000000000000028644 ) ;
#40528 = CARTESIAN_POINT ( 'NONE',  ( 81.94117896397179379, 62.33638752672998606, -2.166533184762309716 ) ) ;
#40529 = CARTESIAN_POINT ( 'NONE',  ( 4.743946363699223845, -28.05441946540344489, 6.939395833800440450 ) ) ;
#40530 = ADVANCED_FACE ( 'NONE', ( #2175, #39829 ), #39403, .F. ) ;
#40532 = CARTESIAN_POINT ( 'NONE',  ( 86.14290222033510247, 1.597928234041334106, -4.557262599208225851 ) ) ;
#40531 = CARTESIAN_POINT ( 'NONE',  ( -70.12833371007830863, -0.1687847323711494374, 5.947160319466099132 ) ) ;
#40533 = CARTESIAN_POINT ( 'NONE',  ( -70.92837670882107659, -27.85319909218681644, 6.138794830819693793 ) ) ;
#40534 = DIRECTION ( 'NONE',  ( 0.000000000000000000, 0.000000000000000000, 1.000000000000000000 ) ) ;
#40535 = CARTESIAN_POINT ( 'NONE',  ( 73.56486102181378328, 61.25343517167133456, 3.876585409328609177 ) ) ;
#40536 = CARTESIAN_POINT ( 'NONE',  ( 24.15427200232377913, 2.904266593399515983, -3.806858982482544729 ) ) ;
#40537 = EDGE_LOOP ( 'NONE', ( #26797, #31938, #6369, #31993 ) ) ;
#40538 = CARTESIAN_POINT ( 'NONE',  ( 21.85643539959776760, 7.606201961588627825, -9.696886732879795190 ) ) ;
#40539 = CARTESIAN_POINT ( 'NONE',  ( 16.14595902796557425, 15.25073734555082794, 3.865347545245052701E-13 ) ) ;
#40540 = VERTEX_POINT ( 'NONE', #14088 ) ;
#40541 = DIRECTION ( 'NONE',  ( 1.000000000000000000, 0.000000000000000000, 0.000000000000000000 ) ) ;
#40542 = CARTESIAN_POINT ( 'NONE',  ( 80.50371486736987947, 65.47929316355259743, 2.914706979937431885 ) ) ;
#40543 = CARTESIAN_POINT ( 'NONE',  ( 87.10491796770416784, 0.5173464865745804886, -5.275911943831619766 ) ) ;
#40544 = EDGE_LOOP ( 'NONE', ( #178, #17345, #22800, #34360 ) ) ;
#40545 = CARTESIAN_POINT ( 'NONE',  ( 2.714783994791350352, -32.91970706126133450, 6.961115707816238007 ) ) ;
#40546 = CARTESIAN_POINT ( 'NONE',  ( 28.89384288918207844, -3.006948380915847263, 4.715981001724134813 ) ) ;
#40547 = CIRCLE ( 'NONE', #13614, 2.499999999999996891 ) ;
#40548 = CARTESIAN_POINT ( 'NONE',  ( -1.699609906766908818, -29.56993018339339940, 6.949309202340325342 ) ) ;
#40549 = CARTESIAN_POINT ( 'NONE',  ( 36.99353526044117046, -2.718331692064833494, -5.980133888059827818 ) ) ;
#40550 = CARTESIAN_POINT ( 'NONE',  ( -14.44874870218064089, -26.64985754041175525, 6.700000000000000178 ) ) ;
#40551 = CARTESIAN_POINT ( 'NONE',  ( -42.83131703149249603, -29.56993018339339940, 6.800000000000000711 ) ) ;
#40552 =( GEOMETRIC_REPRESENTATION_CONTEXT ( 3 ) GLOBAL_UNCERTAINTY_ASSIGNED_CONTEXT ( ( #12276 ) ) GLOBAL_UNIT_ASSIGNED_CONTEXT ( ( #15675, #22683, #28646 ) ) REPRESENTATION_CONTEXT ( 'NONE', 'WORKASPACE' ) );
#40553 = FACE_OUTER_BOUND ( 'NONE', #772, .T. ) ;
#40554 = AXIS2_PLACEMENT_3D ( 'NONE', #14013, #20390, #19802 ) ;
#40555 = EDGE_CURVE ( 'NONE', #37478, #10099, #7918, .T. ) ;
#40556 = CIRCLE ( 'NONE', #14260, 0.1000000000000028644 ) ;
#40557 = DIRECTION ( 'NONE',  ( 1.000000000000000000, 0.000000000000000000, 0.000000000000000000 ) ) ;
#40558 = EDGE_CURVE ( 'NONE', #37250, #7879, #1555, .T. ) ;
#40559 = ORIENTED_EDGE ( 'NONE', *, *, #26938, .T. ) ;
#40560 = EDGE_LOOP ( 'NONE', ( #22241, #7310, #9497, #2486, #25837 ) ) ;
#40561 = CARTESIAN_POINT ( 'NONE',  ( 37.21137251006081215, -2.743940103560390753, 6.000897398658226578 ) ) ;
#40562 = B_SPLINE_CURVE_WITH_KNOTS ( 'NONE', 3,
 ( #33531, #39264, #30424, #4510, #4699, #1618 ),
 .UNSPECIFIED., .F., .F.,
 ( 4, 2, 4 ),
 ( 0.001097151095971008686, 0.001245689619143885377, 0.001394228142316762285 ),
 .UNSPECIFIED. ) ;
#40563 = CARTESIAN_POINT ( 'NONE',  ( -71.90801809991052096, -0.5528860982213333886, 5.931544551966187129 ) ) ;
#40564 = VERTEX_POINT ( 'NONE', #1975 ) ;
#40565 = CARTESIAN_POINT ( 'NONE',  ( 67.01285850879368411, 57.98447793263278527, -3.999354069328931782 ) ) ;
#40566 = ADVANCED_FACE ( 'NONE', ( #8518 ), #29945, .T. ) ;
#40567 = EDGE_LOOP ( 'NONE', ( #7009, #5587, #12371, #17611 ) ) ;
#40568 = CARTESIAN_POINT ( 'NONE',  ( -57.41832745699786500, 33.02173582530747353, 4.020356607641593527 ) ) ;
#40569 = CARTESIAN_POINT ( 'NONE',  ( -74.69374601795452406, -4.520613029625567769, -9.269913512513538123 ) ) ;
#40570 = DIRECTION ( 'NONE',  ( 0.000000000000000000, 0.000000000000000000, 1.000000000000000000 ) ) ;
#40571 = CARTESIAN_POINT ( 'NONE',  ( -64.94969918204330384, 34.86787045525706219, 6.612452343231767671 ) ) ;
#40572 = ORIENTED_EDGE ( 'NONE', *, *, #25016, .T. ) ;
#40573 = CARTESIAN_POINT ( 'NONE',  ( 1.300000000000000044, 0.000000000000000000, 0.000000000000000000 ) ) ;
#40574 = DIRECTION ( 'NONE',  ( -1.000000000000000000, -0.000000000000000000, -0.000000000000000000 ) ) ;
#40575 = EDGE_LOOP ( 'NONE', ( #3231, #2403, #35200, #3144 ) ) ;
#40576 = CARTESIAN_POINT ( 'NONE',  ( 22.89285562436331745, 4.257133708064684718, 3.156151907905176746 ) ) ;
#40577 = CARTESIAN_POINT ( 'NONE',  ( 81.16936534046872964, 61.30390240240431865, -1.014334479594669602 ) ) ;
#40578 = CARTESIAN_POINT ( 'NONE',  ( 80.15412116699829426, 64.17350884197745131, 3.654032574946332268 ) ) ;
#40579 = CARTESIAN_POINT ( 'NONE',  ( -0.1155882611554212708, -32.44435575052494869, 6.865312560952602894 ) ) ;
#40580 = ORIENTED_EDGE ( 'NONE', *, *, #15663, .T. ) ;
#40581 = CARTESIAN_POINT ( 'NONE',  ( 76.03108743707694828, 63.27561679962271057, -3.498861892150602060 ) ) ;
#40582 = CARTESIAN_POINT ( 'NONE',  ( 14.81709837128977014, 12.80649608571206599, -2.504134368729534543 ) ) ;
#40583 = B_SPLINE_CURVE_WITH_KNOTS ( 'NONE', 3,
 ( #2002, #33078, #14717, #17396, #7748, #24203, #26890, #30394, #20297, #5475 ),
 .UNSPECIFIED., .F., .F.,
 ( 4, 2, 2, 2, 4 ),
 ( 0.001564566806966613197, 0.001955354412007498290, 0.002346142017048383384, 0.002736929622089268477, 0.003127717227130153571 ),
 .UNSPECIFIED. ) ;
#40585 = DIRECTION ( 'NONE',  ( -1.000000000000000000, 0.000000000000000000, 0.000000000000000000 ) ) ;
#40584 = LINE ( 'NONE', #12795, #29849 ) ;
#40586 = CARTESIAN_POINT ( 'NONE',  ( 17.61407464359234609, 8.411925271401869963, -2.955500364774379385 ) ) ;
#40587 = AXIS2_PLACEMENT_3D ( 'NONE', #23370, #14293, #35938 ) ;
#40588 = CARTESIAN_POINT ( 'NONE',  ( 81.36347513509552698, 62.06248151587791995, -2.615128354545410705 ) ) ;
#40589 = CARTESIAN_POINT ( 'NONE',  ( -4.224659823956008253, -51.67615071827237472, 2.500000000000000000 ) ) ;
#40590 = CARTESIAN_POINT ( 'NONE',  ( 78.43336062804338837, 61.18469638573561298, 3.363831406680000136 ) ) ;
#40591 = AXIS2_PLACEMENT_3D ( 'NONE', #33849, #9116, #12411 ) ;
#40592 = ORIENTED_EDGE ( 'NONE', *, *, #25537, .F. ) ;
#40593 = VECTOR ( 'NONE', #11640, 1000.000000000000000 ) ;
#40594 = CARTESIAN_POINT ( 'NONE',  ( 0.6783104270758654186, -48.60743831809499227, -6.000000000000000000 ) ) ;
#40595 = CARTESIAN_POINT ( 'NONE',  ( -57.31086168400016589, 33.19661634462462274, 4.000000000000000000 ) ) ;
#40596 = CARTESIAN_POINT ( 'NONE',  ( 81.32635356316056630, 65.55379304840816701, 2.259066313177355401 ) ) ;
#40598 = CARTESIAN_POINT ( 'NONE',  ( -1.578260247530195670, -30.79486269434816492, 7.660770905198775793 ) ) ;
#40597 = CARTESIAN_POINT ( 'NONE',  ( -64.08758708074093136, 41.04287353446839148, 3.000000000000000000 ) ) ;
#40599 = CARTESIAN_POINT ( 'NONE',  ( 31.86155337613836380, -4.142523116122148963, 4.178567150506776962 ) ) ;
#40600 = LINE ( 'NONE', #34463, #35919 ) ;
#40601 = CARTESIAN_POINT ( 'NONE',  ( -62.75232748054406073, 36.25463151227798875, -4.889949273166490862 ) ) ;
#40602 = CARTESIAN_POINT ( 'NONE',  ( -64.52806261857489289, 36.37942767235070818, 5.858659361856595638 ) ) ;
#40603 = CARTESIAN_POINT ( 'NONE',  ( 22.32588140555700917, 0.2761883842276166012, -7.044564668695222132 ) ) ;
#40604 = FACE_OUTER_BOUND ( 'NONE', #25738, .T. ) ;
#40605 = EDGE_CURVE ( 'NONE', #3561, #24059, #20887, .T. ) ;
#40606 = LINE ( 'NONE', #12412, #36232 ) ;
#40607 = PLANE ( 'NONE',  #18195 ) ;
#40608 = CYLINDRICAL_SURFACE ( 'NONE', #8492, 2.500000000000000444 ) ;
#40609 = CARTESIAN_POINT ( 'NONE',  ( -0.3487487021806359722, -26.64985754041175525, 6.700000000000000178 ) ) ;
#40610 = CARTESIAN_POINT ( 'NONE',  ( 34.13092259911290682, -3.728237912347327043, -5.351359701968583238 ) ) ;
#40611 = CARTESIAN_POINT ( 'NONE',  ( -4.348748702180639469, -26.64985754041175525, 6.700000000000000178 ) ) ;
#40612 = CARTESIAN_POINT ( 'NONE',  ( 32.73787262251559582, -3.800317724956558063, 4.944879674104074141 ) ) ;
#40613 = CARTESIAN_POINT ( 'NONE',  ( -0.8809027425463861194, -31.78283038357269419, 7.703977250142849620 ) ) ;
#40614 = CARTESIAN_POINT ( 'NONE',  ( 28.61591789821288145, 47.14532032487838364, 1.000000000000000000 ) ) ;
#40615 = CARTESIAN_POINT ( 'NONE',  ( 2.183653651549320340, -33.03640625185305879, 7.750000000000000888 ) ) ;
#40616 = CARTESIAN_POINT ( 'NONE',  ( 1.671000381532037560, -26.17005720858299966, 7.661510568013097711 ) ) ;
#40617 = EDGE_CURVE ( 'NONE', #7083, #29790, #36939, .T. ) ;
#40618 = CARTESIAN_POINT ( 'NONE',  ( 87.09859342968812257, 0.5244505078549105415, -5.068689133590885909 ) ) ;
#40619 = AXIS2_PLACEMENT_3D ( 'NONE', #2039, #14554, #30430 ) ;
#40620 = CARTESIAN_POINT ( 'NONE',  ( 14.77222177532591196, -4.492696128702778680, -2.511960494210057959 ) ) ;
#40621 = EDGE_CURVE ( 'NONE', #29368, #18695, #29409, .T. ) ;
#40622 = CARTESIAN_POINT ( 'NONE',  ( -1.510909903798922427, -30.68686900403765705, 6.894806418505348589 ) ) ;
#40623 = VERTEX_POINT ( 'NONE', #36139 ) ;
#40624 = CYLINDRICAL_SURFACE ( 'NONE', #27174, 0.09010775117052870209 ) ;
#40625 = CARTESIAN_POINT ( 'NONE',  ( 69.52987064631375347, 59.66723168662304033, -3.901551322707137004 ) ) ;
#40626 = EDGE_CURVE ( 'NONE', #579, #28636, #26462, .T. ) ;
#40627 = ORIENTED_EDGE ( 'NONE', *, *, #11832, .F. ) ;
#40628 = DIRECTION ( 'NONE',  ( 0.3420201433256536139, 0.9396926207859139790, 0.000000000000000000 ) ) ;
#40629 = EDGE_CURVE ( 'NONE', #21561, #40359, #22280, .T. ) ;
#40630 = DIRECTION ( 'NONE',  ( -0.6427876096865179356, -0.7660444431189958880, 0.000000000000000000 ) ) ;
#40631 = CARTESIAN_POINT ( 'NONE',  ( -1.438163258879938455, -28.26242175678535418, 6.871394612369935651 ) ) ;
#40632 = CARTESIAN_POINT ( 'NONE',  ( 1.173600465780690438, -26.21097873563609326, 6.880147297696982633 ) ) ;
#40633 = CARTESIAN_POINT ( 'NONE',  ( -80.19065981525226050, 31.27226540113725406, -9.800414904976365804 ) ) ;
#40634 = ORIENTED_EDGE ( 'NONE', *, *, #12178, .F. ) ;
#40635 = CARTESIAN_POINT ( 'NONE',  ( 24.77632181662465172, 3.027756120316424049, 3.312394854541005795 ) ) ;
#40636 = PLANE ( 'NONE',  #11597 ) ;
#40637 = EDGE_LOOP ( 'NONE', ( #23228, #51, #9386, #17624 ) ) ;
#40638 = VERTEX_POINT ( 'NONE', #35247 ) ;
#40639 = CARTESIAN_POINT ( 'NONE',  ( 80.35854813638249539, 61.23284135048811549, -2.372109611208351954 ) ) ;
#40641 = CARTESIAN_POINT ( 'NONE',  ( -1.003736583562488072, -27.34783681995375915, 7.697032948437509070 ) ) ;
#40640 = CARTESIAN_POINT ( 'NONE',  ( 22.02793885145894492, 0.2684150387854475905, 7.571002712326798445 ) ) ;
#40642 = CARTESIAN_POINT ( 'NONE',  ( 81.65405438441118235, 61.80769279848058062, -1.809109834152291540 ) ) ;
#40643 = CARTESIAN_POINT ( 'NONE',  ( 80.72339804071911828, 61.33444547702554672, 2.197205184446166193 ) ) ;
#40644 = ORIENTED_EDGE ( 'NONE', *, *, #17922, .F. ) ;
#40645 = CARTESIAN_POINT ( 'NONE',  ( 6.040270069758088667, -32.09115252335679003, 7.635761828346577573 ) ) ;
#40646 = CARTESIAN_POINT ( 'NONE',  ( 82.10909544300281482, 65.20937546977818045, 1.000000000000000000 ) ) ;
#40647 = B_SPLINE_CURVE_WITH_KNOTS ( 'NONE', 3,
 ( #19185, #5816, #34658, #6225, #34043, #21671, #255, #12591, #31751, #31344, #28447, #3563, #16093, #18770, #62, #25158 ),
 .UNSPECIFIED., .F., .F.,
 ( 4, 2, 2, 2, 2, 2, 2, 4 ),
 ( 0.002354838921902799483, 0.002649036855363638438, 0.002943234788824477394, 0.003531630655746170917, 0.003825828589206996862, 0.004120026522667821940, 0.004414224456128647452, 0.004708422389589472963 ),
 .UNSPECIFIED. ) ;
#40648 = CARTESIAN_POINT ( 'NONE',  ( -0.7800240848564992113, -27.24451720821412337, 7.013842709614101167 ) ) ;
#40649 = CARTESIAN_POINT ( 'NONE',  ( 21.85643539959778181, 1.552649203755968488, -12.31912549844641447 ) ) ;
#40650 = CARTESIAN_POINT ( 'NONE',  ( 4.041943119853272037, -26.96886997397920638, 7.754798119455333705 ) ) ;
#40651 = VERTEX_POINT ( 'NONE', #34850 ) ;
#40652 = CARTESIAN_POINT ( 'NONE',  ( -72.84122331582933896, 2.640701540777562251, 10.96218028030935443 ) ) ;
#40653 = CARTESIAN_POINT ( 'NONE',  ( 37.09188196241630209, -3.135874510096115841, 5.972645679324628532 ) ) ;
#40654 = ORIENTED_EDGE ( 'NONE', *, *, #30751, .T. ) ;
#40655 = AXIS2_PLACEMENT_3D ( 'NONE', #36162, #39228, #23598 ) ;
#40656 = DIRECTION ( 'NONE',  ( -0.000000000000000000, 1.000000000000000000, 0.000000000000000000 ) ) ;
#40657 = DIRECTION ( 'NONE',  ( -1.000000000000000000, 0.000000000000000000, 0.000000000000000000 ) ) ;
#40658 = CARTESIAN_POINT ( 'NONE',  ( 1.607140144109659108, -32.96866533745306072, 6.866852738645442322 ) ) ;
#40659 = CARTESIAN_POINT ( 'NONE',  ( 36.68588390344509520, -1.914239285580463745, -5.802834115057662778 ) ) ;
#40660 = CARTESIAN_POINT ( 'NONE',  ( -1.743338437294067456, -30.17658229649751078, 7.767720160662275219 ) ) ;
#40661 = CARTESIAN_POINT ( 'NONE',  ( 14.77291369034715096, 13.25847280940105932, 2.500173083280071040 ) ) ;
#40662 = CARTESIAN_POINT ( 'NONE',  ( -17.27251170661583402, -8.656638842136340273, -2.500000000000000000 ) ) ;
#40663 = CARTESIAN_POINT ( 'NONE',  ( 4.198225232297463805, -33.92331276665304785, 7.635761828346577573 ) ) ;
#40664 = CARTESIAN_POINT ( 'NONE',  ( 3.478789117475594495, -32.58444706447512118, 7.720710062488893577 ) ) ;
#40665 = CARTESIAN_POINT ( 'NONE',  ( 3.977572546501454642, -32.22783162523180067, 7.695279973900954751 ) ) ;
#40666 = CARTESIAN_POINT ( 'NONE',  ( 24.10540974869017461, 0.6288044972621918971, -5.083578459613002032 ) ) ;
#40667 = CARTESIAN_POINT ( 'NONE',  ( -11.07867591359219794, -26.64985754041175525, 6.800000000000000711 ) ) ;
#40668 = VECTOR ( 'NONE', #32022, 1000.000000000000000 ) ;
#40669 = CARTESIAN_POINT ( 'NONE',  ( 24.36315553053532312, 2.932691449427110353, -3.734387699189308130 ) ) ;
#40670 = VERTEX_POINT ( 'NONE', #6419 ) ;
#40671 = CARTESIAN_POINT ( 'NONE',  ( 67.03747645593968230, 57.91646344912344091, 3.998003515188802037 ) ) ;
#40672 = CARTESIAN_POINT ( 'NONE',  ( 36.83721040901404820, -2.495908143111605249, 5.955735614263799604 ) ) ;
#40673 =( BOUNDED_CURVE ( )  B_SPLINE_CURVE ( 3, ( #37356, #12856, #8736, #18415 ),
 .UNSPECIFIED., .F., .T. ) 
 B_SPLINE_CURVE_WITH_KNOTS ( ( 4, 4 ),
 ( 1.381924640371169133, 1.574767692156077148 ),
 .UNSPECIFIED. ) 
 CURVE ( )  GEOMETRIC_REPRESENTATION_ITEM ( )  RATIONAL_B_SPLINE_CURVE ( ( 1.000000000000000000, 0.9969033633783032089, 0.9969033633783032089, 1.000000000000000000 ) ) 
 REPRESENTATION_ITEM ( '' )  );
#40674 = CARTESIAN_POINT ( 'NONE',  ( -1.651477885001130241, -30.14008421266758120, 7.779495906702013741 ) ) ;
#40675 = EDGE_CURVE ( 'NONE', #20764, #18601, #12231, .T. ) ;
#40676 = CYLINDRICAL_SURFACE ( 'NONE', #12213, 0.09010775117052992333 ) ;
#40677 = ADVANCED_FACE ( 'NONE', ( #13195, #16480 ), #3361, .T. ) ;
#40678 = CARTESIAN_POINT ( 'NONE',  ( 36.08735695191136017, -2.181264466747378616, -5.838702847008515384 ) ) ;
#40679 = EDGE_LOOP ( 'NONE', ( #17164, #25454, #9873, #39979 ) ) ;
#40680 = CARTESIAN_POINT ( 'NONE',  ( -81.07947155388369254, 30.81399289130168384, 12.49999999999999645 ) ) ;
#40681 = DIRECTION ( 'NONE',  ( 0.000000000000000000, 0.000000000000000000, 1.000000000000000000 ) ) ;
#40682 = PLANE ( 'NONE',  #31079 ) ;
#40683 = EDGE_LOOP ( 'NONE', ( #14035, #25258, #11332, #9396 ) ) ;
#40684 = CARTESIAN_POINT ( 'NONE',  ( -70.03118149891237465, -21.22462562410226994, 3.932540834694422838 ) ) ;
#40685 = VERTEX_POINT ( 'NONE', #15878 ) ;
#40686 = VERTEX_POINT ( 'NONE', #38300 ) ;
#40687 = CARTESIAN_POINT ( 'NONE',  ( 80.59739669508272186, 62.32949743464985204, -3.275607309966713565 ) ) ;
#40688 = CARTESIAN_POINT ( 'NONE',  ( -19.07867591359219972, -26.64985754041175525, 6.700000000000000178 ) ) ;
#40689 = CARTESIAN_POINT ( 'NONE',  ( 79.55161461803720613, 64.54397228415258780, 3.537885823842634725 ) ) ;
#40691 = VERTEX_POINT ( 'NONE', #28435 ) ;
#40690 = CARTESIAN_POINT ( 'NONE',  ( -0.8291548937095295502, -27.29805823298918455, 6.864276522220859711 ) ) ;
#40692 = CARTESIAN_POINT ( 'NONE',  ( 0.04761811793521757152, -26.48768737936845596, 7.766640943994350010 ) ) ;
#40693 = VECTOR ( 'NONE', #2233, 1000.000000000000000 ) ;
#40694 = B_SPLINE_CURVE_WITH_KNOTS ( 'NONE', 3,
 ( #17216, #32492, #32895, #1215, #29196, #7562, #35981, #38848, #1008, #19728, #1407, #6969, #4682, #26313, #16818, #32695, #10247, #7167, #7762, #38646, #13750, #22826, #13542, #10642, #23219, #26115, #14134, #35784, #4495, #29593, #17015 ),
 .UNSPECIFIED., .F., .F.,
 ( 4, 3, 3, 3, 3, 3, 3, 3, 3, 3, 4 ),
 ( 1.084202172485504434E-18, 3.077658087705639398E-05, 6.152638666998869155E-05, 9.267501192706414340E-05, 0.0001241882240135153224, 0.0001556618703051647400, 0.0001866161554452207315, 0.0002167966385860965208, 0.0002463805737537760258, 0.0002758761370306513517, 0.0002847094172290016881 ),
 .UNSPECIFIED. ) ;
#40696 = CARTESIAN_POINT ( 'NONE',  ( 23.71023650492422163, -7.011372125143266132, 2.558830977042959365 ) ) ;
#40695 = CARTESIAN_POINT ( 'NONE',  ( 4.951888024848370762, -30.86525491651966746, 6.863784140767622333 ) ) ;
#40697 = FACE_OUTER_BOUND ( 'NONE', #38863, .T. ) ;
#40698 = CARTESIAN_POINT ( 'NONE',  ( -55.09636020043951987, 31.27759585575460477, 1.408872394161159836 ) ) ;
#40699 = CARTESIAN_POINT ( 'NONE',  ( 21.83674782184219509, 5.925148072649942144, -3.152431264756139662 ) ) ;
#40700 = ORIENTED_EDGE ( 'NONE', *, *, #14342, .F. ) ;
#40701 = CARTESIAN_POINT ( 'NONE',  ( -63.99293516169446150, 35.89893413629674512, -7.506047544094580637 ) ) ;
#40702 = CARTESIAN_POINT ( 'NONE',  ( 24.19350110911862828, 1.223952504169800948, -6.554579921768042716 ) ) ;
#40703 = CARTESIAN_POINT ( 'NONE',  ( -76.47802091883025355, -4.341682083958475324, -8.338848444810246008 ) ) ;
#40704 = DIRECTION ( 'NONE',  ( 0.3420201433256790380, -0.9396926207859046531, -0.000000000000000000 ) ) ;
#40705 = CARTESIAN_POINT ( 'NONE',  ( 80.95699988731961128, 64.21667718577513995, 3.402511877379640559 ) ) ;
#40706 = CARTESIAN_POINT ( 'NONE',  ( 84.61114100273776728, 2.563204847888557403, 3.486439758113726306 ) ) ;
#40707 = CARTESIAN_POINT ( 'NONE',  ( 15.61612061779542060, 11.17844057676542846, 2.610974633258779765 ) ) ;
#40708 = ORIENTED_EDGE ( 'NONE', *, *, #19865, .T. ) ;
#40709 = DIRECTION ( 'NONE',  ( 0.1303762246624128318, 0.7394003126383930091, -0.6605219282605405695 ) ) ;
#40710 = DIRECTION ( 'NONE',  ( -0.000000000000000000, -0.000000000000000000, -1.000000000000000000 ) ) ;
#40711 = VECTOR ( 'NONE', #11728, 1000.000000000000000 ) ;
#40712 = ORIENTED_EDGE ( 'NONE', *, *, #19347, .T. ) ;
#40713 = EDGE_CURVE ( 'NONE', #19152, #12078, #6824, .T. ) ;
#40714 = DIRECTION ( 'NONE',  ( 0.000000000000000000, 1.000000000000000000, 0.000000000000000000 ) ) ;
#40715 = CARTESIAN_POINT ( 'NONE',  ( -1.781046303933295549, -29.98589987418001357, 7.398879060202668612 ) ) ;
#40716 = CARTESIAN_POINT ( 'NONE',  ( -1.722317759908783996, -28.83844474126830804, 7.750000000000000888 ) ) ;
#40717 = CARTESIAN_POINT ( 'NONE',  ( 85.57827979132923701, 1.010891326585220629, 5.785350395857181915 ) ) ;
#40718 = CARTESIAN_POINT ( 'NONE',  ( 36.97917538118862524, -2.955947328860137002, 5.977892681607455572 ) ) ;
#40719 = CARTESIAN_POINT ( 'NONE',  ( 4.259121667494660812, -31.80890180388914956, 7.784476445165073422 ) ) ;
#40720 = FACE_BOUND ( 'NONE', #39577, .T. ) ;
#40721 = NEXT_ASSEMBLY_USAGE_OCCURRENCE ( 'NAUO1', ' ', ' ', #11447, #15152, $ ) ;
#40722 = NEXT_ASSEMBLY_USAGE_OCCURRENCE ( 'NAUO2', ' ', ' ', #11447, #35317, $ ) ;
#40723 = NEXT_ASSEMBLY_USAGE_OCCURRENCE ( 'NAUO3', ' ', ' ', #11447, #21965, $ ) ;
#40724 = NEXT_ASSEMBLY_USAGE_OCCURRENCE ( 'NAUO4', ' ', ' ', #11447, #17491, $ ) ;
#40725 = NEXT_ASSEMBLY_USAGE_OCCURRENCE ( 'NAUO5', ' ', ' ', #11447, #17491, $ ) ;
#40726 = NEXT_ASSEMBLY_USAGE_OCCURRENCE ( 'NAUO6', ' ', ' ', #11447, #38149, $ ) ;
#40727 = NEXT_ASSEMBLY_USAGE_OCCURRENCE ( 'NAUO7', ' ', ' ', #11447, #32149, $ ) ;
#40728 = NEXT_ASSEMBLY_USAGE_OCCURRENCE ( 'NAUO8', ' ', ' ', #11447, #27315, $ ) ;
#40729 = NEXT_ASSEMBLY_USAGE_OCCURRENCE ( 'NAUO9', ' ', ' ', #11447, #39396, $ ) ;
#40730 = NEXT_ASSEMBLY_USAGE_OCCURRENCE ( 'NAUO10', ' ', ' ', #11447, #39396, $ ) ;
#40731 = NEXT_ASSEMBLY_USAGE_OCCURRENCE ( 'NAUO11', ' ', ' ', #11447, #8438, $ ) ;
#40732=COLOUR_RGB('Dark Blue',0.08,0.2,0.34);
#40733=FILL_AREA_STYLE_COLOUR('',#40732);
#40734=FILL_AREA_STYLE('',(#40733));
#40735=SURFACE_STYLE_FILL_AREA(#40734);
#40736=SURFACE_SIDE_STYLE('',(#40735));
#40737=SURFACE_STYLE_USAGE(.BOTH.,#40736);
#40738=PRESENTATION_STYLE_ASSIGNMENT((#40737));
#40739=COLOUR_RGB('Light Blue',0.38,0.62,0.78);
#40740=FILL_AREA_STYLE_COLOUR('',#40739);
#40741=FILL_AREA_STYLE('',(#40740));
#40742=SURFACE_STYLE_FILL_AREA(#40741);
#40743=SURFACE_SIDE_STYLE('',(#40742));
#40744=SURFACE_STYLE_USAGE(.BOTH.,#40743);
#40745=PRESENTATION_STYLE_ASSIGNMENT((#40744));
#40746=COLOUR_RGB('Sky Blue',0.24,0.69,0.87);
#40747=FILL_AREA_STYLE_COLOUR('',#40746);
#40748=FILL_AREA_STYLE('',(#40747));
#40749=SURFACE_STYLE_FILL_AREA(#40748);
#40750=SURFACE_SIDE_STYLE('',(#40749));
#40751=SURFACE_STYLE_USAGE(.BOTH.,#40750);
#40752=PRESENTATION_STYLE_ASSIGNMENT((#40751));
#40753=COLOUR_RGB('Grey',0.48,0.52,0.57);
#40754=FILL_AREA_STYLE_COLOUR('',#40753);
#40755=FILL_AREA_STYLE('',(#40754));
#40756=SURFACE_STYLE_FILL_AREA(#40755);
#40757=SURFACE_SIDE_STYLE('',(#40756));
#40758=SURFACE_STYLE_USAGE(.BOTH.,#40757);
#40759=PRESENTATION_STYLE_ASSIGNMENT((#40758));
#40760=COLOUR_RGB('Black',0.12,0.14,0.17);
#40761=FILL_AREA_STYLE_COLOUR('',#40760);
#40762=FILL_AREA_STYLE('',(#40761));
#40763=SURFACE_STYLE_FILL_AREA(#40762);
#40764=SURFACE_SIDE_STYLE('',(#40763));
#40765=SURFACE_STYLE_USAGE(.BOTH.,#40764);
#40766=PRESENTATION_STYLE_ASSIGNMENT((#40765));
#40767=COLOUR_RGB('Off White',0.89,0.88,0.83);
#40768=FILL_AREA_STYLE_COLOUR('',#40767);
#40769=FILL_AREA_STYLE('',(#40768));
#40770=SURFACE_STYLE_FILL_AREA(#40769);
#40771=SURFACE_SIDE_STYLE('',(#40770));
#40772=SURFACE_STYLE_USAGE(.BOTH.,#40771);
#40773=PRESENTATION_STYLE_ASSIGNMENT((#40772));
ENDSEC;
END-ISO-10303-21;
